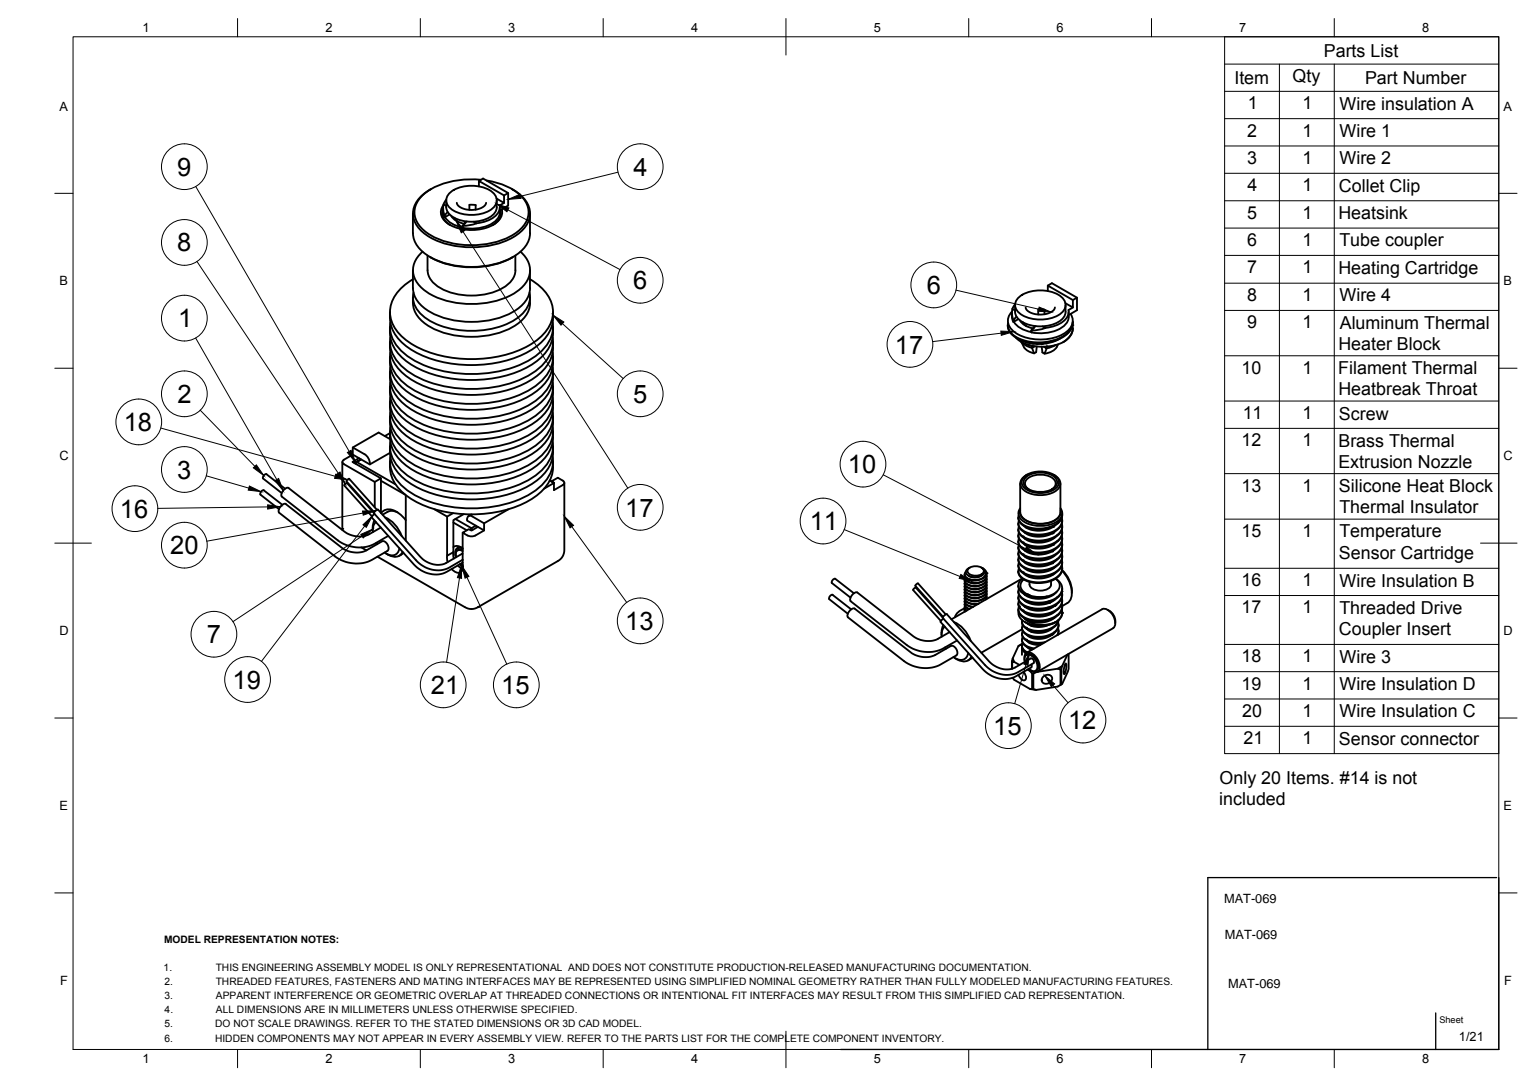
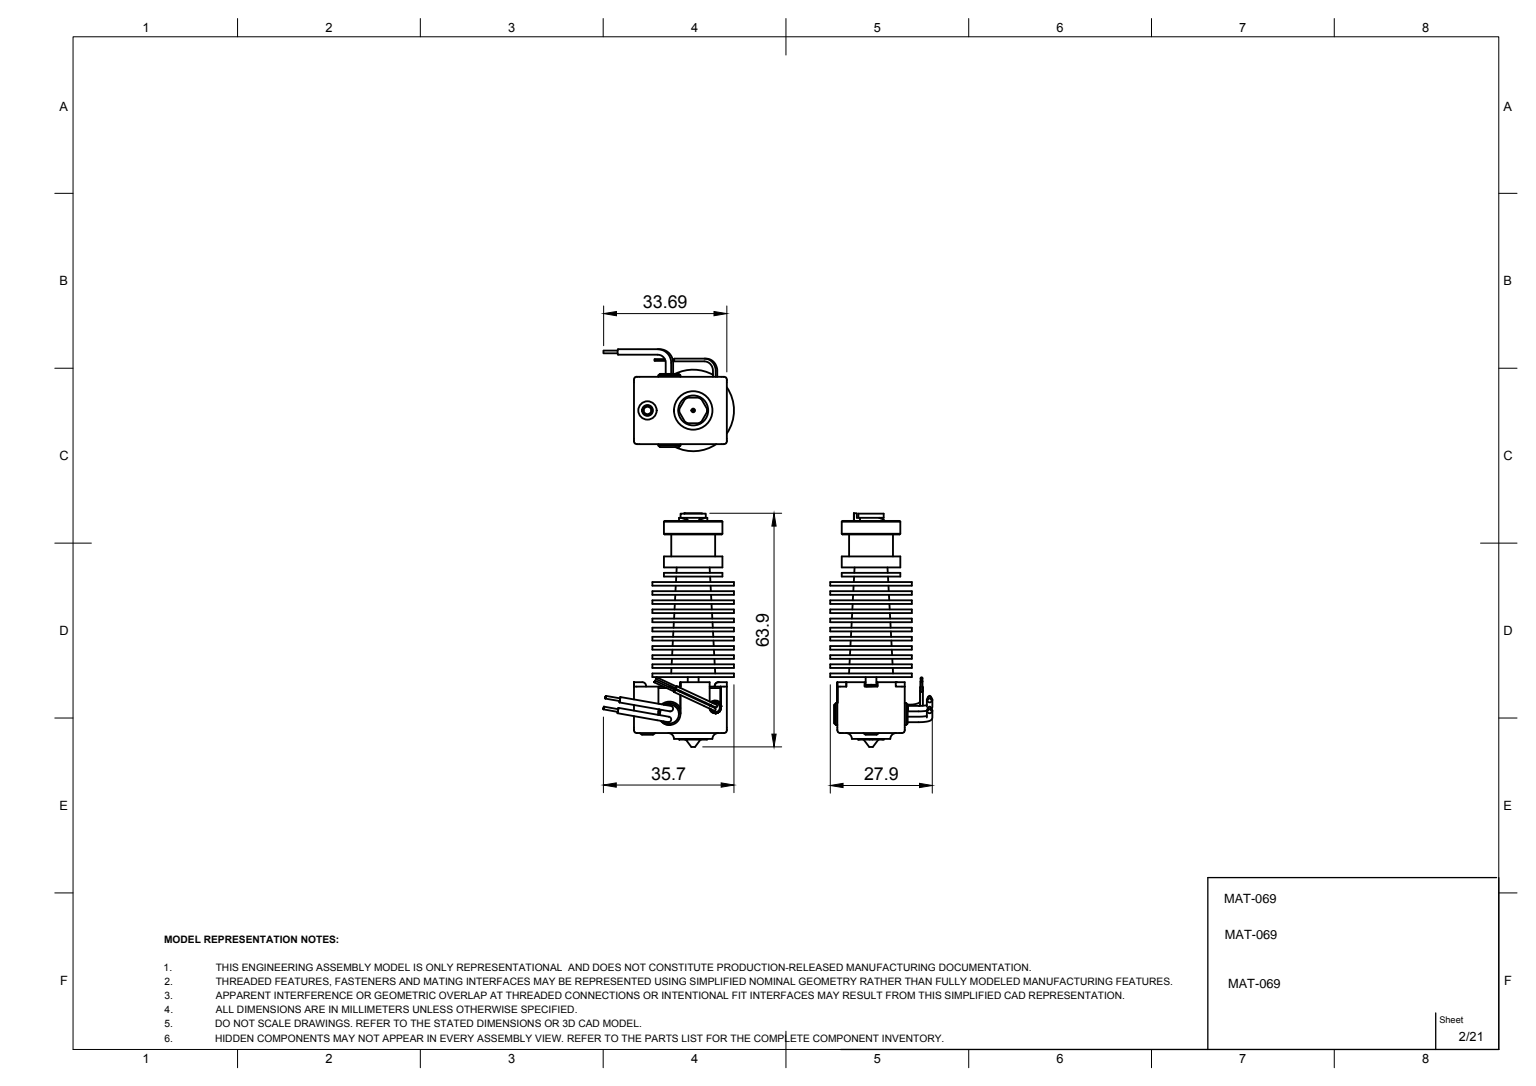
ISO-10303-21;
HEADER;
/* Generated by software containing ST-Developer
 * from STEP Tools, Inc. (www.steptools.com) 
 */

FILE_DESCRIPTION(
/* description */ ('CAx-IF Rec.Pracs.---Representation and Presentation of Product Manufa
cturing Information (PMI)---4.0---2014-10-13'),
/* implementation_level */ '2;1');

FILE_NAME(
/* name */ 'MAT-069',
/* time_stamp */ '2026-10-24T15:08:39-07:00',
/* author */ (''),
/* organization */ (''),
/* preprocessor_version */ 'ST-DEVELOPER v20.2',
/* originating_system */ 'Autodesk Translation Framework v15.17.0.0',
/* authorisation */ '');

FILE_SCHEMA (('AP242_MANAGED_MODEL_BASED_3D_ENGINEERING_MIM_LF { 1 0 10303 442 2 1 4 }'));
ENDSEC;

DATA;
#10=MECHANICAL_DESIGN_GEOMETRIC_PRESENTATION_REPRESENTATION('',(#820,#821,
#822,#823,#824,#825,#826,#827,#828,#829,#830,#831,#832,#833,#834,#835,#836,
#837,#838,#839),#50081);
#11=ITEM_DEFINED_TRANSFORMATION($,$,#10107,#11015);
#12=ITEM_DEFINED_TRANSFORMATION($,$,#10113,#11016);
#13=ITEM_DEFINED_TRANSFORMATION($,$,#10126,#11017);
#14=ITEM_DEFINED_TRANSFORMATION($,$,#10139,#11018);
#15=ITEM_DEFINED_TRANSFORMATION($,$,#10265,#11019);
#16=ITEM_DEFINED_TRANSFORMATION($,$,#10400,#11020);
#17=ITEM_DEFINED_TRANSFORMATION($,$,#10427,#11021);
#18=ITEM_DEFINED_TRANSFORMATION($,$,#10440,#11022);
#19=ITEM_DEFINED_TRANSFORMATION($,$,#10453,#11023);
#20=ITEM_DEFINED_TRANSFORMATION($,$,#10466,#11024);
#21=ITEM_DEFINED_TRANSFORMATION($,$,#10607,#11025);
#22=ITEM_DEFINED_TRANSFORMATION($,$,#10620,#11026);
#23=ITEM_DEFINED_TRANSFORMATION($,$,#10669,#11027);
#24=ITEM_DEFINED_TRANSFORMATION($,$,#10679,#11028);
#25=ITEM_DEFINED_TRANSFORMATION($,$,#10748,#11029);
#26=ITEM_DEFINED_TRANSFORMATION($,$,#10891,#11030);
#27=ITEM_DEFINED_TRANSFORMATION($,$,#10899,#11031);
#28=ITEM_DEFINED_TRANSFORMATION($,$,#10966,#11032);
#29=ITEM_DEFINED_TRANSFORMATION($,$,#10979,#11033);
#30=ITEM_DEFINED_TRANSFORMATION($,$,#10992,#11034);
#31=(
REPRESENTATION_RELATIONSHIP($,$,#50148,#50147)
REPRESENTATION_RELATIONSHIP_WITH_TRANSFORMATION(#11)
SHAPE_REPRESENTATION_RELATIONSHIP()
);
#32=(
REPRESENTATION_RELATIONSHIP($,$,#50149,#50147)
REPRESENTATION_RELATIONSHIP_WITH_TRANSFORMATION(#12)
SHAPE_REPRESENTATION_RELATIONSHIP()
);
#33=(
REPRESENTATION_RELATIONSHIP($,$,#50150,#50147)
REPRESENTATION_RELATIONSHIP_WITH_TRANSFORMATION(#13)
SHAPE_REPRESENTATION_RELATIONSHIP()
);
#34=(
REPRESENTATION_RELATIONSHIP($,$,#50151,#50147)
REPRESENTATION_RELATIONSHIP_WITH_TRANSFORMATION(#14)
SHAPE_REPRESENTATION_RELATIONSHIP()
);
#35=(
REPRESENTATION_RELATIONSHIP($,$,#50152,#50147)
REPRESENTATION_RELATIONSHIP_WITH_TRANSFORMATION(#15)
SHAPE_REPRESENTATION_RELATIONSHIP()
);
#36=(
REPRESENTATION_RELATIONSHIP($,$,#50153,#50147)
REPRESENTATION_RELATIONSHIP_WITH_TRANSFORMATION(#16)
SHAPE_REPRESENTATION_RELATIONSHIP()
);
#37=(
REPRESENTATION_RELATIONSHIP($,$,#50154,#50147)
REPRESENTATION_RELATIONSHIP_WITH_TRANSFORMATION(#17)
SHAPE_REPRESENTATION_RELATIONSHIP()
);
#38=(
REPRESENTATION_RELATIONSHIP($,$,#50155,#50147)
REPRESENTATION_RELATIONSHIP_WITH_TRANSFORMATION(#18)
SHAPE_REPRESENTATION_RELATIONSHIP()
);
#39=(
REPRESENTATION_RELATIONSHIP($,$,#50156,#50147)
REPRESENTATION_RELATIONSHIP_WITH_TRANSFORMATION(#19)
SHAPE_REPRESENTATION_RELATIONSHIP()
);
#40=(
REPRESENTATION_RELATIONSHIP($,$,#50157,#50147)
REPRESENTATION_RELATIONSHIP_WITH_TRANSFORMATION(#20)
SHAPE_REPRESENTATION_RELATIONSHIP()
);
#41=(
REPRESENTATION_RELATIONSHIP($,$,#50158,#50147)
REPRESENTATION_RELATIONSHIP_WITH_TRANSFORMATION(#21)
SHAPE_REPRESENTATION_RELATIONSHIP()
);
#42=(
REPRESENTATION_RELATIONSHIP($,$,#50159,#50147)
REPRESENTATION_RELATIONSHIP_WITH_TRANSFORMATION(#22)
SHAPE_REPRESENTATION_RELATIONSHIP()
);
#43=(
REPRESENTATION_RELATIONSHIP($,$,#50160,#50147)
REPRESENTATION_RELATIONSHIP_WITH_TRANSFORMATION(#23)
SHAPE_REPRESENTATION_RELATIONSHIP()
);
#44=(
REPRESENTATION_RELATIONSHIP($,$,#50161,#50147)
REPRESENTATION_RELATIONSHIP_WITH_TRANSFORMATION(#24)
SHAPE_REPRESENTATION_RELATIONSHIP()
);
#45=(
REPRESENTATION_RELATIONSHIP($,$,#50162,#50147)
REPRESENTATION_RELATIONSHIP_WITH_TRANSFORMATION(#25)
SHAPE_REPRESENTATION_RELATIONSHIP()
);
#46=(
REPRESENTATION_RELATIONSHIP($,$,#50163,#50147)
REPRESENTATION_RELATIONSHIP_WITH_TRANSFORMATION(#26)
SHAPE_REPRESENTATION_RELATIONSHIP()
);
#47=(
REPRESENTATION_RELATIONSHIP($,$,#50164,#50147)
REPRESENTATION_RELATIONSHIP_WITH_TRANSFORMATION(#27)
SHAPE_REPRESENTATION_RELATIONSHIP()
);
#48=(
REPRESENTATION_RELATIONSHIP($,$,#50165,#50147)
REPRESENTATION_RELATIONSHIP_WITH_TRANSFORMATION(#28)
SHAPE_REPRESENTATION_RELATIONSHIP()
);
#49=(
REPRESENTATION_RELATIONSHIP($,$,#50166,#50147)
REPRESENTATION_RELATIONSHIP_WITH_TRANSFORMATION(#29)
SHAPE_REPRESENTATION_RELATIONSHIP()
);
#50=(
REPRESENTATION_RELATIONSHIP($,$,#50167,#50147)
REPRESENTATION_RELATIONSHIP_WITH_TRANSFORMATION(#30)
SHAPE_REPRESENTATION_RELATIONSHIP()
);
#51=CONTEXT_DEPENDENT_SHAPE_REPRESENTATION(#31,#50127);
#52=CONTEXT_DEPENDENT_SHAPE_REPRESENTATION(#32,#50128);
#53=CONTEXT_DEPENDENT_SHAPE_REPRESENTATION(#33,#50129);
#54=CONTEXT_DEPENDENT_SHAPE_REPRESENTATION(#34,#50130);
#55=CONTEXT_DEPENDENT_SHAPE_REPRESENTATION(#35,#50131);
#56=CONTEXT_DEPENDENT_SHAPE_REPRESENTATION(#36,#50132);
#57=CONTEXT_DEPENDENT_SHAPE_REPRESENTATION(#37,#50133);
#58=CONTEXT_DEPENDENT_SHAPE_REPRESENTATION(#38,#50134);
#59=CONTEXT_DEPENDENT_SHAPE_REPRESENTATION(#39,#50135);
#60=CONTEXT_DEPENDENT_SHAPE_REPRESENTATION(#40,#50136);
#61=CONTEXT_DEPENDENT_SHAPE_REPRESENTATION(#41,#50137);
#62=CONTEXT_DEPENDENT_SHAPE_REPRESENTATION(#42,#50138);
#63=CONTEXT_DEPENDENT_SHAPE_REPRESENTATION(#43,#50139);
#64=CONTEXT_DEPENDENT_SHAPE_REPRESENTATION(#44,#50140);
#65=CONTEXT_DEPENDENT_SHAPE_REPRESENTATION(#45,#50141);
#66=CONTEXT_DEPENDENT_SHAPE_REPRESENTATION(#46,#50142);
#67=CONTEXT_DEPENDENT_SHAPE_REPRESENTATION(#47,#50143);
#68=CONTEXT_DEPENDENT_SHAPE_REPRESENTATION(#48,#50144);
#69=CONTEXT_DEPENDENT_SHAPE_REPRESENTATION(#49,#50145);
#70=CONTEXT_DEPENDENT_SHAPE_REPRESENTATION(#50,#50146);
#71=NEXT_ASSEMBLY_USAGE_OCCURRENCE('Sensor connector:1',
'Sensor connector:1','Sensor connector:1',#50169,#50170,
'Sensor connector:1');
#72=NEXT_ASSEMBLY_USAGE_OCCURRENCE('Wire Insulation D:1',
'Wire Insulation D:1','Wire Insulation D:1',#50169,#50171,
'Wire Insulation D:1');
#73=NEXT_ASSEMBLY_USAGE_OCCURRENCE('Wire Insulation C:1',
'Wire Insulation C:1','Wire Insulation C:1',#50169,#50172,
'Wire Insulation C:1');
#74=NEXT_ASSEMBLY_USAGE_OCCURRENCE('Tube coupler:1','Tube coupler:1',
'Tube coupler:1',#50169,#50173,'Tube coupler:1');
#75=NEXT_ASSEMBLY_USAGE_OCCURRENCE('Heatsink:1','Heatsink:1',
'Heatsink:1',#50169,#50174,'Heatsink:1');
#76=NEXT_ASSEMBLY_USAGE_OCCURRENCE('Collet Clip:1','Collet Clip:1',
'Collet Clip:1',#50169,#50175,'Collet Clip:1');
#77=NEXT_ASSEMBLY_USAGE_OCCURRENCE('Wire insulation A:1',
'Wire insulation A:1','Wire insulation A:1',#50169,#50176,
'Wire insulation A:1');
#78=NEXT_ASSEMBLY_USAGE_OCCURRENCE('Wire 2:1','Wire 2:1','Wire 2:1',#50169,
#50177,'Wire 2:1');
#79=NEXT_ASSEMBLY_USAGE_OCCURRENCE('Wire 1:1','Wire 1:1','Wire 1:1',#50169,
#50178,'Wire 1:1');
#80=NEXT_ASSEMBLY_USAGE_OCCURRENCE('Aluminum Thermal Heater Block:1',
'Aluminum Thermal Heater Block:1','Aluminum Thermal Heater Block:1',#50169,
#50179,'Aluminum Thermal Heater Block:1');
#81=NEXT_ASSEMBLY_USAGE_OCCURRENCE('Wire 4:1','Wire 4:1','Wire 4:1',#50169,
#50180,'Wire 4:1');
#82=NEXT_ASSEMBLY_USAGE_OCCURRENCE(
'Filament Thermal Heatbreak Throat:1',
'Filament Thermal Heatbreak Throat:1',
'Filament Thermal Heatbreak Throat:1',#50169,#50181,
'Filament Thermal Heatbreak Throat:1');
#83=NEXT_ASSEMBLY_USAGE_OCCURRENCE('Heating Cartridge:1',
'Heating Cartridge:1','Heating Cartridge:1',#50169,#50182,
'Heating Cartridge:1');
#84=NEXT_ASSEMBLY_USAGE_OCCURRENCE('Brass Thermal Extrusion Nozzle:1',
'Brass Thermal Extrusion Nozzle:1','Brass Thermal Extrusion Nozzle:1',#50169,
#50183,'Brass Thermal Extrusion Nozzle:1');
#85=NEXT_ASSEMBLY_USAGE_OCCURRENCE(
'Silicone Heat Block Thermal Insulator:1',
'Silicone Heat Block Thermal Insulator:1',
'Silicone Heat Block Thermal Insulator:1',#50169,#50184,
'Silicone Heat Block Thermal Insulator:1');
#86=NEXT_ASSEMBLY_USAGE_OCCURRENCE('Temperature Sensor Cartridge:1',
'Temperature Sensor Cartridge:1','Temperature Sensor Cartridge:1',#50169,
#50185,'Temperature Sensor Cartridge:1');
#87=NEXT_ASSEMBLY_USAGE_OCCURRENCE('Screw:1','Screw:1','Screw:1',#50169,
#50186,'Screw:1');
#88=NEXT_ASSEMBLY_USAGE_OCCURRENCE('Wire Insulation B:1',
'Wire Insulation B:1','Wire Insulation B:1',#50169,#50187,
'Wire Insulation B:1');
#89=NEXT_ASSEMBLY_USAGE_OCCURRENCE('Wire 3:1','Wire 3:1','Wire 3:1',#50169,
#50188,'Wire 3:1');
#90=NEXT_ASSEMBLY_USAGE_OCCURRENCE('Threaded Drive Coupler Insert:1',
'Threaded Drive Coupler Insert:1','Threaded Drive Coupler Insert:1',#50169,
#50189,'Threaded Drive Coupler Insert:1');
#91=(
BOUNDED_SURFACE()
B_SPLINE_SURFACE(1,2,((#48380,#48381,#48382,#48383,#48384,#48385,#48386,
#48387,#48388,#48389,#48390,#48391,#48392,#48393,#48394,#48395,#48396,#48397,
#48398,#48399,#48400,#48401,#48402,#48403,#48404,#48405,#48406,#48407,#48408,
#48409,#48410,#48411,#48412,#48413,#48414,#48415,#48416,#48417,#48418,#48419,
#48420,#48421,#48422,#48423,#48424,#48425,#48426,#48427,#48428,#48429,#48430,
#48431,#48432,#48433,#48434,#48435,#48436,#48437,#48438,#48439,#48440,#48441,
#48442,#48443,#48444,#48445,#48446,#48447,#48448,#48449,#48450,#48451,#48452,
#48453,#48454,#48455,#48456,#48457,#48458,#48459,#48460,#48461,#48462,#48463,
#48464,#48465,#48466,#48467,#48468,#48469,#48470,#48471,#48472,#48473,#48474,
#48475,#48476,#48477,#48478,#48479,#48480,#48481,#48482,#48483,#48484,#48485,
#48486,#48487,#48488,#48489,#48490,#48491,#48492,#48493,#48494,#48495,#48496,
#48497,#48498,#48499,#48500,#48501,#48502,#48503,#48504,#48505,#48506,#48507,
#48508,#48509,#48510,#48511,#48512,#48513,#48514,#48515,#48516,#48517,#48518,
#48519,#48520,#48521,#48522,#48523,#48524,#48525,#48526,#48527,#48528,#48529,
#48530,#48531,#48532,#48533,#48534,#48535,#48536,#48537,#48538,#48539,#48540,
#48541,#48542,#48543,#48544,#48545,#48546,#48547,#48548,#48549,#48550,#48551,
#48552,#48553,#48554,#48555,#48556,#48557,#48558,#48559,#48560,#48561,#48562,
#48563,#48564,#48565,#48566,#48567,#48568,#48569,#48570,#48571,#48572,#48573,
#48574,#48575,#48576,#48577,#48578),(#48579,#48580,#48581,#48582,#48583,
#48584,#48585,#48586,#48587,#48588,#48589,#48590,#48591,#48592,#48593,#48594,
#48595,#48596,#48597,#48598,#48599,#48600,#48601,#48602,#48603,#48604,#48605,
#48606,#48607,#48608,#48609,#48610,#48611,#48612,#48613,#48614,#48615,#48616,
#48617,#48618,#48619,#48620,#48621,#48622,#48623,#48624,#48625,#48626,#48627,
#48628,#48629,#48630,#48631,#48632,#48633,#48634,#48635,#48636,#48637,#48638,
#48639,#48640,#48641,#48642,#48643,#48644,#48645,#48646,#48647,#48648,#48649,
#48650,#48651,#48652,#48653,#48654,#48655,#48656,#48657,#48658,#48659,#48660,
#48661,#48662,#48663,#48664,#48665,#48666,#48667,#48668,#48669,#48670,#48671,
#48672,#48673,#48674,#48675,#48676,#48677,#48678,#48679,#48680,#48681,#48682,
#48683,#48684,#48685,#48686,#48687,#48688,#48689,#48690,#48691,#48692,#48693,
#48694,#48695,#48696,#48697,#48698,#48699,#48700,#48701,#48702,#48703,#48704,
#48705,#48706,#48707,#48708,#48709,#48710,#48711,#48712,#48713,#48714,#48715,
#48716,#48717,#48718,#48719,#48720,#48721,#48722,#48723,#48724,#48725,#48726,
#48727,#48728,#48729,#48730,#48731,#48732,#48733,#48734,#48735,#48736,#48737,
#48738,#48739,#48740,#48741,#48742,#48743,#48744,#48745,#48746,#48747,#48748,
#48749,#48750,#48751,#48752,#48753,#48754,#48755,#48756,#48757,#48758,#48759,
#48760,#48761,#48762,#48763,#48764,#48765,#48766,#48767,#48768,#48769,#48770,
#48771,#48772,#48773,#48774,#48775,#48776,#48777)),.UNSPECIFIED.,.F.,.F.,
 .F.)
B_SPLINE_SURFACE_WITH_KNOTS((2,2),(3,2,2,2,2,2,2,2,2,2,2,2,2,2,2,2,2,2,
2,2,2,2,2,2,2,2,2,2,2,2,2,2,2,2,2,2,2,2,2,2,2,2,2,2,2,2,2,2,2,2,2,2,2,2,
2,2,2,2,2,2,2,2,2,2,2,2,2,2,2,2,2,2,2,2,2,2,2,2,2,2,2,2,2,2,2,2,2,2,2,2,
2,2,2,2,2,2,2,2,2,3),(0.,1.00004093151987),(0.0295122414599334,0.0392156862745098,
0.0490196078431373,0.0588235294117647,0.0686274509803922,0.0784313725490196,
0.0882352941176471,0.0980392156862745,0.107843137254902,0.117647058823529,
0.127450980392157,0.137254901960784,0.147058823529412,0.156862745098039,
0.166666666666667,0.176470588235294,0.186274509803922,0.196078431372549,
0.205882352941176,0.215686274509804,0.225490196078431,0.235294117647059,
0.245098039215686,0.254901960784314,0.264705882352941,0.274509803921569,
0.284313725490196,0.294117647058824,0.303921568627451,0.313725490196078,
0.323529411764706,0.333333333333333,0.343137254901961,0.352941176470588,
0.362745098039216,0.372549019607843,0.382352941176471,0.392156862745098,
0.401960784313726,0.411764705882353,0.42156862745098,0.431372549019608,
0.441176470588235,0.450980392156863,0.46078431372549,0.470588235294118,
0.480392156862745,0.490196078431373,0.5,0.509803921568627,0.519607843137255,
0.529411764705882,0.53921568627451,0.549019607843137,0.558823529411765,
0.568627450980392,0.57843137254902,0.588235294117647,0.598039215686274,
0.607843137254902,0.617647058823529,0.627450980392157,0.637254901960784,
0.647058823529412,0.656862745098039,0.666666666666667,0.676470588235294,
0.686274509803922,0.696078431372549,0.705882352941177,0.715686274509804,
0.725490196078431,0.735294117647059,0.745098039215686,0.754901960784314,
0.764705882352941,0.774509803921569,0.784313725490196,0.794117647058823,
0.803921568627451,0.813725490196078,0.823529411764706,0.833333333333333,
0.843137254901961,0.852941176470588,0.862745098039216,0.872549019607843,
0.882352941176471,0.892156862745098,0.901960784313726,0.911764705882353,
0.92156862745098,0.931372549019608,0.941176470588235,0.950980392156863,
0.96078431372549,0.970588235294118,0.980392156862745,0.990196078431373,
0.998519452012734),.UNSPECIFIED.)
GEOMETRIC_REPRESENTATION_ITEM()
RATIONAL_B_SPLINE_SURFACE(((0.997282032040392,0.867398459704848,1.,0.866025403784439,
1.,0.866025403784439,1.,0.866025403784439,1.,0.866025403784439,1.,0.866025403784439,
1.,0.866025403784439,1.,0.866025403784439,1.,0.866025403784439,1.,0.866025403784439,
1.,0.866025403784439,1.,0.866025403784439,1.,0.866025403784439,1.,0.866025403784439,
1.,0.866025403784439,1.,0.866025403784439,1.,0.866025403784439,1.,0.866025403784439,
1.,0.866025403784439,1.,0.866025403784439,1.,0.866025403784439,1.,0.866025403784439,
1.,0.866025403784439,1.,0.866025403784439,1.,0.866025403784439,1.,0.866025403784439,
1.,0.866025403784439,1.,0.866025403784439,1.,0.866025403784439,1.,0.866025403784439,
1.,0.866025403784439,1.,0.866025403784439,1.,0.866025403784439,1.,0.866025403784439,
1.,0.866025403784439,1.,0.866025403784439,1.,0.866025403784439,1.,0.866025403784439,
1.,0.866025403784439,1.,0.866025403784439,1.,0.866025403784439,1.,0.866025403784439,
1.,0.866025403784439,1.,0.866025403784439,1.,0.866025403784439,1.,0.866025403784439,
1.,0.866025403784439,1.,0.866025403784439,1.,0.866025403784439,1.,0.866025403784439,
1.,0.866025403784439,1.,0.866025403784439,1.,0.866025403784439,1.,0.866025403784439,
1.,0.866025403784439,1.,0.866025403784439,1.,0.866025403784439,1.,0.866025403784439,
1.,0.866025403784439,1.,0.866025403784439,1.,0.866025403784439,1.,0.866025403784439,
1.,0.866025403784439,1.,0.866025403784439,1.,0.866025403784439,1.,0.866025403784439,
1.,0.866025403784439,1.,0.866025403784439,1.,0.866025403784439,1.,0.866025403784439,
1.,0.866025403784439,1.,0.866025403784439,1.,0.866025403784439,1.,0.866025403784439,
1.,0.866025403784439,1.,0.866025403784439,1.,0.866025403784439,1.,0.866025403784439,
1.,0.866025403784439,1.,0.866025403784439,1.,0.866025403784439,1.,0.866025403784439,
1.,0.866025403784439,1.,0.866025403784439,1.,0.866025403784439,1.,0.866025403784439,
1.,0.866025403784439,1.,0.866025403784439,1.,0.866025403784439,1.,0.866025403784439,
1.,0.866025403784439,1.,0.866025403784439,1.,0.866025403784439,1.,0.866025403784439,
1.,0.866025403784439,1.,0.866025403784439,1.,0.866025403784439,1.,0.866025403784439,
1.,0.886257697299162,0.965646208784519),(0.997282032040392,0.867398459704848,
1.,0.866025403784439,1.,0.866025403784439,1.,0.866025403784439,1.,0.866025403784439,
1.,0.866025403784439,1.,0.866025403784439,1.,0.866025403784439,1.,0.866025403784439,
1.,0.866025403784439,1.,0.866025403784439,1.,0.866025403784439,1.,0.866025403784439,
1.,0.866025403784439,1.,0.866025403784439,1.,0.866025403784439,1.,0.866025403784439,
1.,0.866025403784439,1.,0.866025403784439,1.,0.866025403784439,1.,0.866025403784439,
1.,0.866025403784439,1.,0.866025403784439,1.,0.866025403784439,1.,0.866025403784439,
1.,0.866025403784439,1.,0.866025403784439,1.,0.866025403784439,1.,0.866025403784439,
1.,0.866025403784439,1.,0.866025403784439,1.,0.866025403784439,1.,0.866025403784439,
1.,0.866025403784439,1.,0.866025403784439,1.,0.866025403784439,1.,0.866025403784439,
1.,0.866025403784439,1.,0.866025403784439,1.,0.866025403784439,1.,0.866025403784439,
1.,0.866025403784439,1.,0.866025403784439,1.,0.866025403784439,1.,0.866025403784439,
1.,0.866025403784439,1.,0.866025403784439,1.,0.866025403784439,1.,0.866025403784439,
1.,0.866025403784439,1.,0.866025403784439,1.,0.866025403784439,1.,0.866025403784439,
1.,0.866025403784439,1.,0.866025403784439,1.,0.866025403784439,1.,0.866025403784439,
1.,0.866025403784439,1.,0.866025403784439,1.,0.866025403784439,1.,0.866025403784439,
1.,0.866025403784439,1.,0.866025403784439,1.,0.866025403784439,1.,0.866025403784439,
1.,0.866025403784439,1.,0.866025403784439,1.,0.866025403784439,1.,0.866025403784439,
1.,0.866025403784439,1.,0.866025403784439,1.,0.866025403784439,1.,0.866025403784439,
1.,0.866025403784439,1.,0.866025403784439,1.,0.866025403784439,1.,0.866025403784439,
1.,0.866025403784439,1.,0.866025403784439,1.,0.866025403784439,1.,0.866025403784439,
1.,0.866025403784439,1.,0.866025403784439,1.,0.866025403784439,1.,0.866025403784439,
1.,0.866025403784439,1.,0.866025403784439,1.,0.866025403784439,1.,0.866025403784439,
1.,0.866025403784439,1.,0.866025403784439,1.,0.866025403784439,1.,0.866025403784439,
1.,0.866025403784439,1.,0.866025403784439,1.,0.866025403784439,1.,0.866025403784439,
1.,0.866025403784439,1.,0.886257697299162,0.965646208784519)))
REPRESENTATION_ITEM('')
SURFACE()
);
#92=(
BOUNDED_SURFACE()
B_SPLINE_SURFACE(1,2,((#48794,#48795,#48796,#48797,#48798,#48799,#48800,
#48801,#48802,#48803,#48804,#48805,#48806,#48807,#48808,#48809,#48810,#48811,
#48812,#48813,#48814,#48815,#48816,#48817,#48818,#48819,#48820,#48821,#48822,
#48823,#48824,#48825,#48826,#48827,#48828,#48829,#48830,#48831,#48832,#48833,
#48834,#48835,#48836,#48837,#48838,#48839,#48840,#48841,#48842,#48843,#48844,
#48845,#48846,#48847,#48848,#48849,#48850,#48851,#48852,#48853,#48854,#48855,
#48856,#48857,#48858,#48859,#48860,#48861,#48862,#48863,#48864,#48865,#48866,
#48867,#48868,#48869,#48870,#48871,#48872,#48873,#48874,#48875,#48876,#48877,
#48878,#48879,#48880,#48881,#48882,#48883,#48884,#48885,#48886,#48887,#48888,
#48889,#48890,#48891,#48892,#48893,#48894,#48895,#48896,#48897,#48898,#48899,
#48900,#48901,#48902,#48903,#48904,#48905,#48906,#48907,#48908,#48909,#48910,
#48911,#48912,#48913,#48914,#48915,#48916,#48917,#48918,#48919,#48920,#48921,
#48922,#48923,#48924,#48925,#48926,#48927,#48928,#48929,#48930,#48931,#48932,
#48933,#48934,#48935,#48936,#48937,#48938,#48939,#48940,#48941,#48942,#48943,
#48944,#48945,#48946,#48947,#48948,#48949,#48950,#48951,#48952,#48953,#48954,
#48955,#48956,#48957,#48958,#48959,#48960,#48961,#48962,#48963,#48964,#48965,
#48966,#48967,#48968,#48969,#48970,#48971,#48972,#48973,#48974,#48975,#48976,
#48977,#48978,#48979,#48980,#48981,#48982,#48983,#48984,#48985,#48986,#48987,
#48988),(#48989,#48990,#48991,#48992,#48993,#48994,#48995,#48996,#48997,
#48998,#48999,#49000,#49001,#49002,#49003,#49004,#49005,#49006,#49007,#49008,
#49009,#49010,#49011,#49012,#49013,#49014,#49015,#49016,#49017,#49018,#49019,
#49020,#49021,#49022,#49023,#49024,#49025,#49026,#49027,#49028,#49029,#49030,
#49031,#49032,#49033,#49034,#49035,#49036,#49037,#49038,#49039,#49040,#49041,
#49042,#49043,#49044,#49045,#49046,#49047,#49048,#49049,#49050,#49051,#49052,
#49053,#49054,#49055,#49056,#49057,#49058,#49059,#49060,#49061,#49062,#49063,
#49064,#49065,#49066,#49067,#49068,#49069,#49070,#49071,#49072,#49073,#49074,
#49075,#49076,#49077,#49078,#49079,#49080,#49081,#49082,#49083,#49084,#49085,
#49086,#49087,#49088,#49089,#49090,#49091,#49092,#49093,#49094,#49095,#49096,
#49097,#49098,#49099,#49100,#49101,#49102,#49103,#49104,#49105,#49106,#49107,
#49108,#49109,#49110,#49111,#49112,#49113,#49114,#49115,#49116,#49117,#49118,
#49119,#49120,#49121,#49122,#49123,#49124,#49125,#49126,#49127,#49128,#49129,
#49130,#49131,#49132,#49133,#49134,#49135,#49136,#49137,#49138,#49139,#49140,
#49141,#49142,#49143,#49144,#49145,#49146,#49147,#49148,#49149,#49150,#49151,
#49152,#49153,#49154,#49155,#49156,#49157,#49158,#49159,#49160,#49161,#49162,
#49163,#49164,#49165,#49166,#49167,#49168,#49169,#49170,#49171,#49172,#49173,
#49174,#49175,#49176,#49177,#49178,#49179,#49180,#49181,#49182,#49183)),
 .UNSPECIFIED.,.F.,.F.,.F.)
B_SPLINE_SURFACE_WITH_KNOTS((2,2),(3,2,2,2,2,2,2,2,2,2,2,2,2,2,2,2,2,2,
2,2,2,2,2,2,2,2,2,2,2,2,2,2,2,2,2,2,2,2,2,2,2,2,2,2,2,2,2,2,2,2,2,2,2,2,
2,2,2,2,2,2,2,2,2,2,2,2,2,2,2,2,2,2,2,2,2,2,2,2,2,2,2,2,2,2,2,2,2,2,2,2,
2,2,2,2,2,2,2,3),(-4.46693850465293E-5,1.00004466937728),(0.0222318908269079,
0.0294117647058824,0.0392156862745098,0.0490196078431373,0.0588235294117647,
0.0686274509803922,0.0784313725490196,0.0882352941176471,0.0980392156862745,
0.107843137254902,0.117647058823529,0.127450980392157,0.137254901960784,
0.147058823529412,0.156862745098039,0.166666666666667,0.176470588235294,
0.186274509803922,0.196078431372549,0.205882352941176,0.215686274509804,
0.225490196078431,0.235294117647059,0.245098039215686,0.254901960784314,
0.264705882352941,0.274509803921569,0.284313725490196,0.294117647058824,
0.303921568627451,0.313725490196078,0.323529411764706,0.333333333333333,
0.343137254901961,0.352941176470588,0.362745098039216,0.372549019607843,
0.382352941176471,0.392156862745098,0.401960784313726,0.411764705882353,
0.42156862745098,0.431372549019608,0.441176470588235,0.450980392156863,
0.46078431372549,0.470588235294118,0.480392156862745,0.490196078431373,
0.5,0.509803921568627,0.519607843137255,0.529411764705882,0.53921568627451,
0.549019607843137,0.558823529411765,0.568627450980392,0.57843137254902,
0.588235294117647,0.598039215686274,0.607843137254902,0.617647058823529,
0.627450980392157,0.637254901960784,0.647058823529412,0.656862745098039,
0.666666666666667,0.676470588235294,0.686274509803922,0.696078431372549,
0.705882352941177,0.715686274509804,0.725490196078431,0.735294117647059,
0.745098039215686,0.754901960784314,0.764705882352941,0.774509803921569,
0.784313725490196,0.794117647058823,0.803921568627451,0.813725490196078,
0.823529411764706,0.833333333333333,0.843137254901961,0.852941176470588,
0.862745098039216,0.872549019607843,0.882352941176471,0.892156862745098,
0.901960784313726,0.911764705882353,0.92156862745098,0.931372549019608,
0.941176470588235,0.950980392156863,0.96078431372549,0.968975690801275),
 .UNSPECIFIED.)
GEOMETRIC_REPRESENTATION_ITEM()
RATIONAL_B_SPLINE_SURFACE(((0.947477990343754,0.901884088210946,1.,0.866025403784439,
1.,0.866025403784439,1.,0.866025403784439,1.,0.866025403784439,1.,0.866025403784439,
1.,0.866025403784439,1.,0.866025403784439,1.,0.866025403784439,1.,0.866025403784439,
1.,0.866025403784439,1.,0.866025403784439,1.,0.866025403784439,1.,0.866025403784439,
1.,0.866025403784439,1.,0.866025403784439,1.,0.866025403784439,1.,0.866025403784439,
1.,0.866025403784439,1.,0.866025403784439,1.,0.866025403784439,1.,0.866025403784439,
1.,0.866025403784439,1.,0.866025403784439,1.,0.866025403784439,1.,0.866025403784439,
1.,0.866025403784439,1.,0.866025403784439,1.,0.866025403784439,1.,0.866025403784439,
1.,0.866025403784439,1.,0.866025403784439,1.,0.866025403784439,1.,0.866025403784439,
1.,0.866025403784439,1.,0.866025403784439,1.,0.866025403784439,1.,0.866025403784439,
1.,0.866025403784439,1.,0.866025403784439,1.,0.866025403784439,1.,0.866025403784439,
1.,0.866025403784439,1.,0.866025403784439,1.,0.866025403784439,1.,0.866025403784439,
1.,0.866025403784439,1.,0.866025403784439,1.,0.866025403784439,1.,0.866025403784439,
1.,0.866025403784439,1.,0.866025403784439,1.,0.866025403784439,1.,0.866025403784439,
1.,0.866025403784439,1.,0.866025403784439,1.,0.866025403784439,1.,0.866025403784439,
1.,0.866025403784439,1.,0.866025403784439,1.,0.866025403784439,1.,0.866025403784439,
1.,0.866025403784439,1.,0.866025403784439,1.,0.866025403784439,1.,0.866025403784439,
1.,0.866025403784439,1.,0.866025403784439,1.,0.866025403784439,1.,0.866025403784439,
1.,0.866025403784439,1.,0.866025403784439,1.,0.866025403784439,1.,0.866025403784439,
1.,0.866025403784439,1.,0.866025403784439,1.,0.866025403784439,1.,0.866025403784439,
1.,0.866025403784439,1.,0.866025403784439,1.,0.866025403784439,1.,0.866025403784439,
1.,0.866025403784439,1.,0.866025403784439,1.,0.866025403784439,1.,0.866025403784439,
1.,0.866025403784439,1.,0.866025403784439,1.,0.866025403784439,1.,0.866025403784439,
1.,0.866025403784439,1.,0.866025403784439,1.,0.866025403784439,1.,0.866025403784439,
1.,0.866025403784439,1.,0.866025403784439,1.,0.888061483509882,0.963176808986156),
(0.947477990343754,0.901884088210946,1.,0.866025403784439,1.,0.866025403784439,
1.,0.866025403784439,1.,0.866025403784439,1.,0.866025403784439,1.,0.866025403784439,
1.,0.866025403784439,1.,0.866025403784439,1.,0.866025403784439,1.,0.866025403784439,
1.,0.866025403784439,1.,0.866025403784439,1.,0.866025403784439,1.,0.866025403784439,
1.,0.866025403784439,1.,0.866025403784439,1.,0.866025403784439,1.,0.866025403784439,
1.,0.866025403784439,1.,0.866025403784439,1.,0.866025403784439,1.,0.866025403784439,
1.,0.866025403784439,1.,0.866025403784439,1.,0.866025403784439,1.,0.866025403784439,
1.,0.866025403784439,1.,0.866025403784439,1.,0.866025403784439,1.,0.866025403784439,
1.,0.866025403784439,1.,0.866025403784439,1.,0.866025403784439,1.,0.866025403784439,
1.,0.866025403784439,1.,0.866025403784439,1.,0.866025403784439,1.,0.866025403784439,
1.,0.866025403784439,1.,0.866025403784439,1.,0.866025403784439,1.,0.866025403784439,
1.,0.866025403784439,1.,0.866025403784439,1.,0.866025403784439,1.,0.866025403784439,
1.,0.866025403784439,1.,0.866025403784439,1.,0.866025403784439,1.,0.866025403784439,
1.,0.866025403784439,1.,0.866025403784439,1.,0.866025403784439,1.,0.866025403784439,
1.,0.866025403784439,1.,0.866025403784439,1.,0.866025403784439,1.,0.866025403784439,
1.,0.866025403784439,1.,0.866025403784439,1.,0.866025403784439,1.,0.866025403784439,
1.,0.866025403784439,1.,0.866025403784439,1.,0.866025403784439,1.,0.866025403784439,
1.,0.866025403784439,1.,0.866025403784439,1.,0.866025403784439,1.,0.866025403784439,
1.,0.866025403784439,1.,0.866025403784439,1.,0.866025403784439,1.,0.866025403784439,
1.,0.866025403784439,1.,0.866025403784439,1.,0.866025403784439,1.,0.866025403784439,
1.,0.866025403784439,1.,0.866025403784439,1.,0.866025403784439,1.,0.866025403784439,
1.,0.866025403784439,1.,0.866025403784439,1.,0.866025403784439,1.,0.866025403784439,
1.,0.866025403784439,1.,0.866025403784439,1.,0.866025403784439,1.,0.866025403784439,
1.,0.866025403784439,1.,0.866025403784439,1.,0.866025403784439,1.,0.866025403784439,
1.,0.866025403784439,1.,0.888061483509882,0.963176808986156)))
REPRESENTATION_ITEM('')
SURFACE()
);
#93=SPHERICAL_SURFACE('',#10942,0.00317192226735973);
#94=B_SPLINE_SURFACE_WITH_KNOTS('',3,3,((#16932,#16933,#16934,#16935,#16936,
#16937,#16938,#16939,#16940,#16941,#16942,#16943,#16944,#16945,#16946,#16947,
#16948,#16949,#16950,#16951,#16952,#16953,#16954,#16955,#16956,#16957,#16958,
#16959,#16960,#16961,#16962,#16963,#16964,#16965,#16966,#16967,#16968,#16969,
#16970,#16971,#16972,#16973,#16974,#16975,#16976,#16977,#16978,#16979,#16980,
#16981,#16982,#16983,#16984,#16985,#16986,#16987,#16988,#16989,#16990,#16991,
#16992,#16993,#16994,#16995,#16996,#16997,#16998,#16999,#17000,#17001,#17002,
#17003,#17004,#17005,#17006,#17007,#17008,#17009,#17010,#17011,#17012,#17013,
#17014,#17015,#17016,#17017,#17018,#17019,#17020,#17021,#17022,#17023,#17024),
(#17025,#17026,#17027,#17028,#17029,#17030,#17031,#17032,#17033,#17034,
#17035,#17036,#17037,#17038,#17039,#17040,#17041,#17042,#17043,#17044,#17045,
#17046,#17047,#17048,#17049,#17050,#17051,#17052,#17053,#17054,#17055,#17056,
#17057,#17058,#17059,#17060,#17061,#17062,#17063,#17064,#17065,#17066,#17067,
#17068,#17069,#17070,#17071,#17072,#17073,#17074,#17075,#17076,#17077,#17078,
#17079,#17080,#17081,#17082,#17083,#17084,#17085,#17086,#17087,#17088,#17089,
#17090,#17091,#17092,#17093,#17094,#17095,#17096,#17097,#17098,#17099,#17100,
#17101,#17102,#17103,#17104,#17105,#17106,#17107,#17108,#17109,#17110,#17111,
#17112,#17113,#17114,#17115,#17116,#17117),(#17118,#17119,#17120,#17121,
#17122,#17123,#17124,#17125,#17126,#17127,#17128,#17129,#17130,#17131,#17132,
#17133,#17134,#17135,#17136,#17137,#17138,#17139,#17140,#17141,#17142,#17143,
#17144,#17145,#17146,#17147,#17148,#17149,#17150,#17151,#17152,#17153,#17154,
#17155,#17156,#17157,#17158,#17159,#17160,#17161,#17162,#17163,#17164,#17165,
#17166,#17167,#17168,#17169,#17170,#17171,#17172,#17173,#17174,#17175,#17176,
#17177,#17178,#17179,#17180,#17181,#17182,#17183,#17184,#17185,#17186,#17187,
#17188,#17189,#17190,#17191,#17192,#17193,#17194,#17195,#17196,#17197,#17198,
#17199,#17200,#17201,#17202,#17203,#17204,#17205,#17206,#17207,#17208,#17209,
#17210),(#17211,#17212,#17213,#17214,#17215,#17216,#17217,#17218,#17219,
#17220,#17221,#17222,#17223,#17224,#17225,#17226,#17227,#17228,#17229,#17230,
#17231,#17232,#17233,#17234,#17235,#17236,#17237,#17238,#17239,#17240,#17241,
#17242,#17243,#17244,#17245,#17246,#17247,#17248,#17249,#17250,#17251,#17252,
#17253,#17254,#17255,#17256,#17257,#17258,#17259,#17260,#17261,#17262,#17263,
#17264,#17265,#17266,#17267,#17268,#17269,#17270,#17271,#17272,#17273,#17274,
#17275,#17276,#17277,#17278,#17279,#17280,#17281,#17282,#17283,#17284,#17285,
#17286,#17287,#17288,#17289,#17290,#17291,#17292,#17293,#17294,#17295,#17296,
#17297,#17298,#17299,#17300,#17301,#17302,#17303)),.UNSPECIFIED.,.F.,.F.,
 .F.,(4,4),(4,1,1,1,1,1,1,1,1,1,1,1,1,1,1,1,1,1,1,1,1,1,1,1,1,1,1,1,1,1,
1,1,1,1,1,1,1,1,1,1,1,1,1,1,1,1,1,1,1,1,1,1,1,1,1,1,1,1,1,1,1,1,1,1,1,1,
1,1,1,1,1,1,1,1,1,1,1,1,1,1,1,1,1,1,1,1,1,1,1,1,4),(-0.000398919436546387,
0.0651101464894062),(10.2099830649134,11.2099710040949,12.2097658840232,
13.2095607639514,14.2093556438797,15.2091505238079,16.2089454037362,17.2087402836644,
18.2085351635927,19.208330043521,20.2081249234492,21.2079198033775,22.2077146833057,
23.207509563234,24.2073044431622,25.2070993230905,26.2068942030187,27.206689082947,
28.2064839628752,29.2062788428035,30.2060737227317,31.20586860266,32.2056634825882,
33.2054583625165,34.2052532424447,35.205048122373,36.2048430023012,37.2046378822295,
38.2044327621577,39.204227642086,40.2040225220142,41.2038174019425,42.2036122818707,
43.203407161799,44.2032020417273,45.2029969216555,46.2027918015838,47.202586681512,
48.2023815614403,49.2021764413685,50.2019713212968,51.201766201225,52.2015610811533,
53.2013559610815,54.2011508410098,55.200945720938,56.2007406008663,57.2005354807945,
58.2003303607228,59.200125240651,60.1999201205793,61.1997150005075,62.1995098804358,
63.199304760364,64.1990996402923,65.1988945202205,66.1986894001488,67.1984842800771,
68.1982791600053,69.1980740399336,70.1978689198618,71.1976637997901,72.1974586797183,
73.1972535596466,74.1970484395748,75.1968433195031,76.1966381994313,77.1964330793596,
78.1962279592878,79.1960228392161,80.1958177191443,81.1956125990726,82.1954074790008,
83.1952023589291,84.1949972388573,85.1947921187856,86.1945869987138,87.1943818786421,
88.1941767585704,89.1939716384986,90.1937665184269,91.1935613983551,92.1933562782833,
93.1931511582116,94.1929460381399,95.1927409180681,96.1925357979964,97.1923306779246,
98.1921255578529,99.1919204377811,100.192067891578),.UNSPECIFIED.);
#95=B_SPLINE_SURFACE_WITH_KNOTS('',3,3,((#17371,#17372,#17373,#17374,#17375,
#17376,#17377,#17378,#17379,#17380,#17381,#17382,#17383,#17384,#17385,#17386,
#17387,#17388,#17389,#17390,#17391,#17392,#17393,#17394,#17395,#17396,#17397,
#17398,#17399,#17400,#17401,#17402,#17403,#17404,#17405,#17406,#17407,#17408,
#17409,#17410,#17411,#17412,#17413,#17414,#17415,#17416,#17417,#17418,#17419,
#17420,#17421,#17422,#17423,#17424,#17425,#17426,#17427,#17428,#17429,#17430,
#17431,#17432,#17433,#17434,#17435,#17436,#17437,#17438,#17439,#17440,#17441,
#17442,#17443,#17444,#17445,#17446,#17447,#17448,#17449,#17450,#17451,#17452,
#17453,#17454,#17455,#17456,#17457,#17458,#17459,#17460,#17461,#17462,#17463),
(#17464,#17465,#17466,#17467,#17468,#17469,#17470,#17471,#17472,#17473,
#17474,#17475,#17476,#17477,#17478,#17479,#17480,#17481,#17482,#17483,#17484,
#17485,#17486,#17487,#17488,#17489,#17490,#17491,#17492,#17493,#17494,#17495,
#17496,#17497,#17498,#17499,#17500,#17501,#17502,#17503,#17504,#17505,#17506,
#17507,#17508,#17509,#17510,#17511,#17512,#17513,#17514,#17515,#17516,#17517,
#17518,#17519,#17520,#17521,#17522,#17523,#17524,#17525,#17526,#17527,#17528,
#17529,#17530,#17531,#17532,#17533,#17534,#17535,#17536,#17537,#17538,#17539,
#17540,#17541,#17542,#17543,#17544,#17545,#17546,#17547,#17548,#17549,#17550,
#17551,#17552,#17553,#17554,#17555,#17556),(#17557,#17558,#17559,#17560,
#17561,#17562,#17563,#17564,#17565,#17566,#17567,#17568,#17569,#17570,#17571,
#17572,#17573,#17574,#17575,#17576,#17577,#17578,#17579,#17580,#17581,#17582,
#17583,#17584,#17585,#17586,#17587,#17588,#17589,#17590,#17591,#17592,#17593,
#17594,#17595,#17596,#17597,#17598,#17599,#17600,#17601,#17602,#17603,#17604,
#17605,#17606,#17607,#17608,#17609,#17610,#17611,#17612,#17613,#17614,#17615,
#17616,#17617,#17618,#17619,#17620,#17621,#17622,#17623,#17624,#17625,#17626,
#17627,#17628,#17629,#17630,#17631,#17632,#17633,#17634,#17635,#17636,#17637,
#17638,#17639,#17640,#17641,#17642,#17643,#17644,#17645,#17646,#17647,#17648,
#17649),(#17650,#17651,#17652,#17653,#17654,#17655,#17656,#17657,#17658,
#17659,#17660,#17661,#17662,#17663,#17664,#17665,#17666,#17667,#17668,#17669,
#17670,#17671,#17672,#17673,#17674,#17675,#17676,#17677,#17678,#17679,#17680,
#17681,#17682,#17683,#17684,#17685,#17686,#17687,#17688,#17689,#17690,#17691,
#17692,#17693,#17694,#17695,#17696,#17697,#17698,#17699,#17700,#17701,#17702,
#17703,#17704,#17705,#17706,#17707,#17708,#17709,#17710,#17711,#17712,#17713,
#17714,#17715,#17716,#17717,#17718,#17719,#17720,#17721,#17722,#17723,#17724,
#17725,#17726,#17727,#17728,#17729,#17730,#17731,#17732,#17733,#17734,#17735,
#17736,#17737,#17738,#17739,#17740,#17741,#17742)),.UNSPECIFIED.,.F.,.F.,
 .F.,(4,4),(4,1,1,1,1,1,1,1,1,1,1,1,1,1,1,1,1,1,1,1,1,1,1,1,1,1,1,1,1,1,
1,1,1,1,1,1,1,1,1,1,1,1,1,1,1,1,1,1,1,1,1,1,1,1,1,1,1,1,1,1,1,1,1,1,1,1,
1,1,1,1,1,1,1,1,1,1,1,1,1,1,1,1,1,1,1,1,1,1,1,1,4),(-0.00100526872732246,
0.0646023829588572),(13.6909080459636,14.6908132548486,15.6906081347769,
16.6904030147051,17.6901978946334,18.6899927745616,19.6897876544899,20.6895825344181,
21.6893774143464,22.6891722942746,23.6889671742029,24.6887620541311,25.6885569340594,
26.6883518139876,27.6881466939159,28.6879415738441,29.6877364537724,30.6875313337007,
31.6873262136289,32.6871210935572,33.6869159734854,34.6867108534137,35.6865057333419,
36.6863006132702,37.6860954931984,38.6858903731267,39.6856852530549,40.6854801329832,
41.6852750129114,42.6850698928397,43.6848647727679,44.6846596526962,45.6844545326244,
46.6842494125527,47.6840442924809,48.6838391724092,49.6836340523375,50.6834289322657,
51.683223812194,52.6830186921222,53.6828135720505,54.6826084519787,55.682403331907,
56.6821982118352,57.6819930917635,58.6817879716917,59.68158285162,60.6813777315482,
61.6811726114765,62.6809674914047,63.680762371333,64.6805572512612,65.6803521311895,
66.6801470111178,67.679941891046,68.6797367709743,69.6795316509025,70.6793265308308,
71.679121410759,72.6789162906873,73.6787111706155,74.6785060505438,75.678300930472,
76.6780958104003,77.6778906903285,78.6776855702568,79.677480450185,80.6772753301133,
81.6770702100415,82.6768650899698,83.676659969898,84.6764548498263,85.6762497297545,
86.6760446096828,87.6758394896111,88.6756343695393,89.6754292494676,90.6752241293958,
91.6750190093241,92.6748138892523,93.6746087691806,94.6744036491088,95.6741985290371,
96.6739934089653,97.6737882888936,98.6735831688218,99.6733780487501,100.673172928678,
101.672967808607,102.672762688535,103.67278623601),.UNSPECIFIED.);
#96=B_SPLINE_SURFACE_WITH_KNOTS('',3,3,((#29778,#29779,#29780,#29781,#29782,
#29783,#29784,#29785,#29786,#29787,#29788,#29789,#29790,#29791,#29792,#29793,
#29794,#29795,#29796,#29797,#29798,#29799,#29800,#29801,#29802,#29803,#29804,
#29805,#29806,#29807,#29808,#29809,#29810,#29811,#29812,#29813,#29814,#29815,
#29816,#29817,#29818,#29819,#29820,#29821,#29822,#29823,#29824,#29825,#29826,
#29827,#29828,#29829,#29830,#29831,#29832,#29833,#29834,#29835,#29836,#29837,
#29838,#29839,#29840,#29841,#29842,#29843,#29844,#29845,#29846,#29847,#29848,
#29849,#29850,#29851,#29852,#29853,#29854,#29855,#29856,#29857,#29858,#29859,
#29860,#29861,#29862),(#29863,#29864,#29865,#29866,#29867,#29868,#29869,
#29870,#29871,#29872,#29873,#29874,#29875,#29876,#29877,#29878,#29879,#29880,
#29881,#29882,#29883,#29884,#29885,#29886,#29887,#29888,#29889,#29890,#29891,
#29892,#29893,#29894,#29895,#29896,#29897,#29898,#29899,#29900,#29901,#29902,
#29903,#29904,#29905,#29906,#29907,#29908,#29909,#29910,#29911,#29912,#29913,
#29914,#29915,#29916,#29917,#29918,#29919,#29920,#29921,#29922,#29923,#29924,
#29925,#29926,#29927,#29928,#29929,#29930,#29931,#29932,#29933,#29934,#29935,
#29936,#29937,#29938,#29939,#29940,#29941,#29942,#29943,#29944,#29945,#29946,
#29947),(#29948,#29949,#29950,#29951,#29952,#29953,#29954,#29955,#29956,
#29957,#29958,#29959,#29960,#29961,#29962,#29963,#29964,#29965,#29966,#29967,
#29968,#29969,#29970,#29971,#29972,#29973,#29974,#29975,#29976,#29977,#29978,
#29979,#29980,#29981,#29982,#29983,#29984,#29985,#29986,#29987,#29988,#29989,
#29990,#29991,#29992,#29993,#29994,#29995,#29996,#29997,#29998,#29999,#30000,
#30001,#30002,#30003,#30004,#30005,#30006,#30007,#30008,#30009,#30010,#30011,
#30012,#30013,#30014,#30015,#30016,#30017,#30018,#30019,#30020,#30021,#30022,
#30023,#30024,#30025,#30026,#30027,#30028,#30029,#30030,#30031,#30032),
(#30033,#30034,#30035,#30036,#30037,#30038,#30039,#30040,#30041,#30042,
#30043,#30044,#30045,#30046,#30047,#30048,#30049,#30050,#30051,#30052,#30053,
#30054,#30055,#30056,#30057,#30058,#30059,#30060,#30061,#30062,#30063,#30064,
#30065,#30066,#30067,#30068,#30069,#30070,#30071,#30072,#30073,#30074,#30075,
#30076,#30077,#30078,#30079,#30080,#30081,#30082,#30083,#30084,#30085,#30086,
#30087,#30088,#30089,#30090,#30091,#30092,#30093,#30094,#30095,#30096,#30097,
#30098,#30099,#30100,#30101,#30102,#30103,#30104,#30105,#30106,#30107,#30108,
#30109,#30110,#30111,#30112,#30113,#30114,#30115,#30116,#30117)),
 .UNSPECIFIED.,.F.,.F.,.F.,(4,4),(4,1,1,1,1,1,1,1,1,1,1,1,1,1,1,1,1,1,1,
1,1,1,1,1,1,1,1,1,1,1,1,1,1,1,1,1,1,1,1,1,1,1,1,1,1,1,1,1,1,1,1,1,1,1,1,
1,1,1,1,1,1,1,1,1,1,1,1,1,1,1,1,1,1,1,1,1,1,1,1,1,1,1,4),(-0.000229032876373949,
0.0325052131810458),(10.2100639933856,11.2101668347381,12.2101575453093,
13.2101482558806,14.2101389664519,15.2101296770232,16.2101203875945,17.2101110981658,
18.2101018087371,19.2100925193084,20.2100832298797,21.210073940451,22.2100646510223,
23.2100553615935,24.2100460721648,25.2100367827361,26.2100274933074,27.2100182038787,
28.21000891445,29.2099996250213,30.2099903355926,31.2099810461639,32.2099717567352,
33.2099624673065,34.2099531778778,35.209943888449,36.2099345990203,37.2099253095916,
38.2099160201629,39.2099067307342,40.2098974413055,41.2098881518768,42.2098788624481,
43.2098695730194,44.2098602835907,45.209850994162,46.2098417047333,47.2098324153045,
48.2098231258758,49.2098138364471,50.2098045470184,51.2097952575897,52.209785968161,
53.2097766787323,54.2097673893036,55.2097580998749,56.2097488104462,57.2097395210175,
58.2097302315887,59.20972094216,60.2097116527313,61.2097023633026,62.2096930738739,
63.2096837844452,64.2096744950165,65.2096652055878,66.2096559161591,67.2096466267304,
68.2096373373017,69.209628047873,70.2096187584443,71.2096094690155,72.2096001795868,
73.2095908901581,74.2095816007294,75.2095723113007,76.209563021872,77.2095537324433,
78.2095444430146,79.2095351535859,80.2095258641572,81.2095165747285,82.2095072852998,
83.209497995871,84.2094887064423,85.2094794170136,86.2094701275849,87.2094608381562,
88.2094515487275,89.2094422592988,90.2094329698701,91.2094236804414,92.2094929101791),
 .UNSPECIFIED.);
#97=B_SPLINE_SURFACE_WITH_KNOTS('',3,3,((#30146,#30147,#30148,#30149,#30150,
#30151,#30152,#30153,#30154,#30155,#30156,#30157,#30158,#30159,#30160,#30161,
#30162,#30163,#30164,#30165,#30166,#30167,#30168,#30169,#30170,#30171,#30172,
#30173,#30174,#30175,#30176,#30177,#30178,#30179,#30180,#30181,#30182,#30183,
#30184,#30185,#30186,#30187,#30188,#30189,#30190,#30191,#30192,#30193,#30194,
#30195,#30196,#30197,#30198,#30199,#30200,#30201,#30202,#30203,#30204,#30205,
#30206,#30207,#30208,#30209,#30210,#30211,#30212,#30213,#30214,#30215,#30216,
#30217,#30218,#30219,#30220,#30221,#30222,#30223,#30224,#30225,#30226,#30227,
#30228,#30229,#30230),(#30231,#30232,#30233,#30234,#30235,#30236,#30237,
#30238,#30239,#30240,#30241,#30242,#30243,#30244,#30245,#30246,#30247,#30248,
#30249,#30250,#30251,#30252,#30253,#30254,#30255,#30256,#30257,#30258,#30259,
#30260,#30261,#30262,#30263,#30264,#30265,#30266,#30267,#30268,#30269,#30270,
#30271,#30272,#30273,#30274,#30275,#30276,#30277,#30278,#30279,#30280,#30281,
#30282,#30283,#30284,#30285,#30286,#30287,#30288,#30289,#30290,#30291,#30292,
#30293,#30294,#30295,#30296,#30297,#30298,#30299,#30300,#30301,#30302,#30303,
#30304,#30305,#30306,#30307,#30308,#30309,#30310,#30311,#30312,#30313,#30314,
#30315),(#30316,#30317,#30318,#30319,#30320,#30321,#30322,#30323,#30324,
#30325,#30326,#30327,#30328,#30329,#30330,#30331,#30332,#30333,#30334,#30335,
#30336,#30337,#30338,#30339,#30340,#30341,#30342,#30343,#30344,#30345,#30346,
#30347,#30348,#30349,#30350,#30351,#30352,#30353,#30354,#30355,#30356,#30357,
#30358,#30359,#30360,#30361,#30362,#30363,#30364,#30365,#30366,#30367,#30368,
#30369,#30370,#30371,#30372,#30373,#30374,#30375,#30376,#30377,#30378,#30379,
#30380,#30381,#30382,#30383,#30384,#30385,#30386,#30387,#30388,#30389,#30390,
#30391,#30392,#30393,#30394,#30395,#30396,#30397,#30398,#30399,#30400),
(#30401,#30402,#30403,#30404,#30405,#30406,#30407,#30408,#30409,#30410,
#30411,#30412,#30413,#30414,#30415,#30416,#30417,#30418,#30419,#30420,#30421,
#30422,#30423,#30424,#30425,#30426,#30427,#30428,#30429,#30430,#30431,#30432,
#30433,#30434,#30435,#30436,#30437,#30438,#30439,#30440,#30441,#30442,#30443,
#30444,#30445,#30446,#30447,#30448,#30449,#30450,#30451,#30452,#30453,#30454,
#30455,#30456,#30457,#30458,#30459,#30460,#30461,#30462,#30463,#30464,#30465,
#30466,#30467,#30468,#30469,#30470,#30471,#30472,#30473,#30474,#30475,#30476,
#30477,#30478,#30479,#30480,#30481,#30482,#30483,#30484,#30485)),
 .UNSPECIFIED.,.F.,.F.,.F.,(4,4),(4,1,1,1,1,1,1,1,1,1,1,1,1,1,1,1,1,1,1,
1,1,1,1,1,1,1,1,1,1,1,1,1,1,1,1,1,1,1,1,1,1,1,1,1,1,1,1,1,1,1,1,1,1,1,1,
1,1,1,1,1,1,1,1,1,1,1,1,1,1,1,1,1,1,1,1,1,1,1,1,1,1,1,4),(-0.000337093536336005,
0.0325391625776436),(13.6871942222869,14.6873814867633,15.6873721973346,
16.6873629079059,17.6873536184772,18.6873443290484,19.6873350396197,20.687325750191,
21.6873164607623,22.6873071713336,23.6872978819049,24.6872885924762,25.6872793030475,
26.6872700136188,27.6872607241901,28.6872514347614,29.6872421453326,30.6872328559039,
31.6872235664752,32.6872142770465,33.6872049876178,34.6871956981891,35.6871864087604,
36.6871771193317,37.687167829903,38.6871585404743,39.6871492510456,40.6871399616169,
41.6871306721881,42.6871213827594,43.6871120933307,44.687102803902,45.6870935144733,
46.6870842250446,47.6870749356159,48.6870656461872,49.6870563567585,50.6870470673298,
51.6870377779011,52.6870284884724,53.6870191990436,54.6870099096149,55.6870006201862,
56.6869913307575,57.6869820413288,58.6869727519001,59.6869634624714,60.6869541730427,
61.686944883614,62.6869355941853,63.6869263047566,64.6869170153279,65.6869077258991,
66.6868984364704,67.6868891470417,68.686879857613,69.6868705681843,70.6868612787556,
71.6868519893269,72.6868426998982,73.6868334104695,74.6868241210408,75.6868148316121,
76.6868055421834,77.6867962527546,78.6867869633259,79.6867776738972,80.6867683844685,
81.6867590950398,82.6867498056111,83.6867405161824,84.6867312267537,85.686721937325,
86.6867126478963,87.6867033584676,88.6866940690389,89.6866847796101,90.6866754901814,
91.6866662007527,92.686656911324,93.6866476218953,94.6866383324666,95.6868551020536),
 .UNSPECIFIED.);
#98=B_SPLINE_SURFACE_WITH_KNOTS('',3,3,((#30688,#30689,#30690,#30691,#30692,
#30693,#30694,#30695,#30696,#30697,#30698,#30699,#30700,#30701,#30702,#30703,
#30704,#30705,#30706,#30707,#30708,#30709,#30710,#30711,#30712,#30713,#30714,
#30715,#30716,#30717,#30718,#30719,#30720,#30721,#30722,#30723,#30724,#30725,
#30726,#30727,#30728,#30729,#30730,#30731,#30732,#30733,#30734,#30735,#30736,
#30737,#30738,#30739,#30740,#30741,#30742,#30743,#30744,#30745,#30746,#30747,
#30748,#30749,#30750,#30751,#30752,#30753,#30754,#30755,#30756),(#30757,
#30758,#30759,#30760,#30761,#30762,#30763,#30764,#30765,#30766,#30767,#30768,
#30769,#30770,#30771,#30772,#30773,#30774,#30775,#30776,#30777,#30778,#30779,
#30780,#30781,#30782,#30783,#30784,#30785,#30786,#30787,#30788,#30789,#30790,
#30791,#30792,#30793,#30794,#30795,#30796,#30797,#30798,#30799,#30800,#30801,
#30802,#30803,#30804,#30805,#30806,#30807,#30808,#30809,#30810,#30811,#30812,
#30813,#30814,#30815,#30816,#30817,#30818,#30819,#30820,#30821,#30822,#30823,
#30824,#30825),(#30826,#30827,#30828,#30829,#30830,#30831,#30832,#30833,
#30834,#30835,#30836,#30837,#30838,#30839,#30840,#30841,#30842,#30843,#30844,
#30845,#30846,#30847,#30848,#30849,#30850,#30851,#30852,#30853,#30854,#30855,
#30856,#30857,#30858,#30859,#30860,#30861,#30862,#30863,#30864,#30865,#30866,
#30867,#30868,#30869,#30870,#30871,#30872,#30873,#30874,#30875,#30876,#30877,
#30878,#30879,#30880,#30881,#30882,#30883,#30884,#30885,#30886,#30887,#30888,
#30889,#30890,#30891,#30892,#30893,#30894),(#30895,#30896,#30897,#30898,
#30899,#30900,#30901,#30902,#30903,#30904,#30905,#30906,#30907,#30908,#30909,
#30910,#30911,#30912,#30913,#30914,#30915,#30916,#30917,#30918,#30919,#30920,
#30921,#30922,#30923,#30924,#30925,#30926,#30927,#30928,#30929,#30930,#30931,
#30932,#30933,#30934,#30935,#30936,#30937,#30938,#30939,#30940,#30941,#30942,
#30943,#30944,#30945,#30946,#30947,#30948,#30949,#30950,#30951,#30952,#30953,
#30954,#30955,#30956,#30957,#30958,#30959,#30960,#30961,#30962,#30963)),
 .UNSPECIFIED.,.F.,.F.,.F.,(4,4),(4,1,1,1,1,1,1,1,1,1,1,1,1,1,1,1,1,1,1,
1,1,1,1,1,1,1,1,1,1,1,1,1,1,1,1,1,1,1,1,1,1,1,1,1,1,1,1,1,1,1,1,1,1,1,1,
1,1,1,1,1,1,1,1,1,1,1,4),(-0.000882682909917588,0.0581163152088491),(13.8937860366664,
14.8831634638169,15.8721630239192,16.8611625840214,17.8501621441237,18.8391617042259,
19.8281612643282,20.8171608244304,21.8061603845326,22.7951599446349,23.7841595047371,
24.7731590648394,25.7621586249416,26.7511581850439,27.7401577451461,28.7291573052483,
29.7181568653506,30.7071564254528,31.6961559855551,32.6851555456573,33.6741551057596,
34.6631546658618,35.652154225964,36.6411537860663,37.6301533461685,38.6191529062708,
39.608152466373,40.5971520264753,41.5861515865775,42.5751511466798,43.564150706782,
44.5531502668842,45.5421498269865,46.5311493870887,47.520148947191,48.5091485072932,
49.4981480673955,50.4871476274977,51.4761471875999,52.4651467477022,53.4541463078044,
54.4431458679067,55.4321454280089,56.4211449881112,57.4101445482134,58.3991441083156,
59.3881436684179,60.3771432285201,61.3661427886224,62.3551423487246,63.3441419088269,
64.3331414689291,65.3221410290313,66.3111405891336,67.3001401492358,68.2891397093381,
69.2781392694403,70.2671388295426,71.2561383896448,72.245137949747,73.2341375098493,
74.2231370699515,75.2121366300538,76.201136190156,77.1901357502583,78.1791353103605,
79.1681348704628),.UNSPECIFIED.);
#99=B_SPLINE_SURFACE_WITH_KNOTS('',3,3,((#31557,#31558,#31559,#31560,#31561,
#31562,#31563,#31564,#31565,#31566,#31567,#31568,#31569,#31570,#31571,#31572,
#31573,#31574,#31575,#31576,#31577,#31578,#31579,#31580,#31581,#31582,#31583,
#31584,#31585,#31586,#31587,#31588,#31589,#31590,#31591,#31592,#31593,#31594,
#31595,#31596,#31597,#31598,#31599,#31600,#31601,#31602,#31603,#31604,#31605,
#31606,#31607,#31608,#31609,#31610,#31611,#31612,#31613,#31614,#31615,#31616,
#31617,#31618,#31619,#31620,#31621,#31622,#31623,#31624,#31625),(#31626,
#31627,#31628,#31629,#31630,#31631,#31632,#31633,#31634,#31635,#31636,#31637,
#31638,#31639,#31640,#31641,#31642,#31643,#31644,#31645,#31646,#31647,#31648,
#31649,#31650,#31651,#31652,#31653,#31654,#31655,#31656,#31657,#31658,#31659,
#31660,#31661,#31662,#31663,#31664,#31665,#31666,#31667,#31668,#31669,#31670,
#31671,#31672,#31673,#31674,#31675,#31676,#31677,#31678,#31679,#31680,#31681,
#31682,#31683,#31684,#31685,#31686,#31687,#31688,#31689,#31690,#31691,#31692,
#31693,#31694),(#31695,#31696,#31697,#31698,#31699,#31700,#31701,#31702,
#31703,#31704,#31705,#31706,#31707,#31708,#31709,#31710,#31711,#31712,#31713,
#31714,#31715,#31716,#31717,#31718,#31719,#31720,#31721,#31722,#31723,#31724,
#31725,#31726,#31727,#31728,#31729,#31730,#31731,#31732,#31733,#31734,#31735,
#31736,#31737,#31738,#31739,#31740,#31741,#31742,#31743,#31744,#31745,#31746,
#31747,#31748,#31749,#31750,#31751,#31752,#31753,#31754,#31755,#31756,#31757,
#31758,#31759,#31760,#31761,#31762,#31763),(#31764,#31765,#31766,#31767,
#31768,#31769,#31770,#31771,#31772,#31773,#31774,#31775,#31776,#31777,#31778,
#31779,#31780,#31781,#31782,#31783,#31784,#31785,#31786,#31787,#31788,#31789,
#31790,#31791,#31792,#31793,#31794,#31795,#31796,#31797,#31798,#31799,#31800,
#31801,#31802,#31803,#31804,#31805,#31806,#31807,#31808,#31809,#31810,#31811,
#31812,#31813,#31814,#31815,#31816,#31817,#31818,#31819,#31820,#31821,#31822,
#31823,#31824,#31825,#31826,#31827,#31828,#31829,#31830,#31831,#31832)),
 .UNSPECIFIED.,.F.,.F.,.F.,(4,4),(4,1,1,1,1,1,1,1,1,1,1,1,1,1,1,1,1,1,1,
1,1,1,1,1,1,1,1,1,1,1,1,1,1,1,1,1,1,1,1,1,1,1,1,1,1,1,1,1,1,1,1,1,1,1,1,
1,1,1,1,1,1,1,1,1,1,1,4),(-0.000390001319482014,0.0587333122782212),(10.2099729995397,
11.199175684269,12.1881752443713,13.1771748044735,14.1661743645758,15.155173924678,
16.1441734847802,17.1331730448825,18.1221726049847,19.111172165087,20.1001717251892,
21.0891712852915,22.0781708453937,23.0671704054959,24.0561699655982,25.0451695257004,
26.0341690858027,27.0231686459049,28.0121682060072,29.0011677661094,29.9901673262116,
30.9791668863139,31.9681664464161,32.9571660065184,33.9461655666206,34.9351651267229,
35.9241646868251,36.9131642469273,37.9021638070296,38.8911633671318,39.8801629272341,
40.8691624873363,41.8581620474386,42.8471616075408,43.836161167643,44.8251607277453,
45.8141602878475,46.8031598479498,47.792159408052,48.7811589681543,49.7701585282565,
50.7591580883588,51.748157648461,52.7371572085632,53.7261567686655,54.7151563287677,
55.70415588887,56.6931554489722,57.6821550090744,58.6711545691767,59.6601541292789,
60.6491536893812,61.6381532494834,62.6271528095857,63.6161523696879,64.6051519297902,
65.5941514898924,66.5831510499946,67.5721506100969,68.5611501701991,69.5501497303014,
70.5391492904036,71.5281488505059,72.5171484106081,73.5061479707103,74.4951475308126,
75.484582158383),.UNSPECIFIED.);
#100=B_SPLINE_SURFACE_WITH_KNOTS('',3,3,((#33783,#33784,#33785,#33786,#33787,
#33788,#33789,#33790,#33791,#33792,#33793,#33794,#33795,#33796,#33797,#33798,
#33799,#33800,#33801,#33802,#33803,#33804,#33805,#33806,#33807,#33808,#33809,
#33810,#33811,#33812,#33813,#33814,#33815,#33816,#33817,#33818,#33819,#33820,
#33821,#33822,#33823,#33824,#33825,#33826,#33827,#33828,#33829,#33830,#33831,
#33832,#33833,#33834,#33835,#33836),(#33837,#33838,#33839,#33840,#33841,
#33842,#33843,#33844,#33845,#33846,#33847,#33848,#33849,#33850,#33851,#33852,
#33853,#33854,#33855,#33856,#33857,#33858,#33859,#33860,#33861,#33862,#33863,
#33864,#33865,#33866,#33867,#33868,#33869,#33870,#33871,#33872,#33873,#33874,
#33875,#33876,#33877,#33878,#33879,#33880,#33881,#33882,#33883,#33884,#33885,
#33886,#33887,#33888,#33889,#33890),(#33891,#33892,#33893,#33894,#33895,
#33896,#33897,#33898,#33899,#33900,#33901,#33902,#33903,#33904,#33905,#33906,
#33907,#33908,#33909,#33910,#33911,#33912,#33913,#33914,#33915,#33916,#33917,
#33918,#33919,#33920,#33921,#33922,#33923,#33924,#33925,#33926,#33927,#33928,
#33929,#33930,#33931,#33932,#33933,#33934,#33935,#33936,#33937,#33938,#33939,
#33940,#33941,#33942,#33943,#33944),(#33945,#33946,#33947,#33948,#33949,
#33950,#33951,#33952,#33953,#33954,#33955,#33956,#33957,#33958,#33959,#33960,
#33961,#33962,#33963,#33964,#33965,#33966,#33967,#33968,#33969,#33970,#33971,
#33972,#33973,#33974,#33975,#33976,#33977,#33978,#33979,#33980,#33981,#33982,
#33983,#33984,#33985,#33986,#33987,#33988,#33989,#33990,#33991,#33992,#33993,
#33994,#33995,#33996,#33997,#33998)),.UNSPECIFIED.,.F.,.F.,.F.,(4,4),(4,
1,1,1,1,1,1,1,1,1,1,1,1,1,1,1,1,1,1,1,1,1,1,1,1,1,1,1,1,1,1,1,1,1,1,1,1,
1,1,1,1,1,1,1,1,1,1,1,1,1,1,4),(-0.000427176962040987,0.0325519917386635),
(13.6872368315967,14.6740326940116,15.6606746118312,16.6473165296507,17.6339584474703,
18.6206003652899,19.6072422831094,20.593884200929,21.5805261187486,22.5671680365682,
23.5538099543877,24.5404518722073,25.5270937900269,26.5137357078464,27.500377625666,
28.4870195434856,29.4736614613051,30.4603033791247,31.4469452969443,32.4335872147639,
33.4202291325834,34.406871050403,35.3935129682226,36.3801548860421,37.3667968038617,
38.3534387216813,39.3400806395008,40.3267225573204,41.31336447514,42.3000063929596,
43.2866483107791,44.2732902285987,45.2599321464183,46.2465740642378,47.2332159820574,
48.219857899877,49.2064998176965,50.1931417355161,51.1797836533357,52.1664255711553,
53.1530674889748,54.1397094067944,55.126351324614,56.1129932424335,57.0996351602531,
58.0862770780727,59.0729189958922,60.0595609137118,61.0462028315314,62.032844749351,
63.0194866671705,64.0063577917107),.UNSPECIFIED.);
#101=B_SPLINE_SURFACE_WITH_KNOTS('',3,3,((#34172,#34173,#34174,#34175,#34176,
#34177,#34178,#34179,#34180,#34181,#34182,#34183,#34184,#34185,#34186,#34187,
#34188,#34189,#34190,#34191,#34192,#34193,#34194,#34195,#34196,#34197,#34198,
#34199,#34200,#34201,#34202,#34203,#34204,#34205,#34206,#34207,#34208,#34209,
#34210,#34211,#34212,#34213,#34214,#34215,#34216,#34217,#34218,#34219,#34220,
#34221,#34222,#34223,#34224,#34225),(#34226,#34227,#34228,#34229,#34230,
#34231,#34232,#34233,#34234,#34235,#34236,#34237,#34238,#34239,#34240,#34241,
#34242,#34243,#34244,#34245,#34246,#34247,#34248,#34249,#34250,#34251,#34252,
#34253,#34254,#34255,#34256,#34257,#34258,#34259,#34260,#34261,#34262,#34263,
#34264,#34265,#34266,#34267,#34268,#34269,#34270,#34271,#34272,#34273,#34274,
#34275,#34276,#34277,#34278,#34279),(#34280,#34281,#34282,#34283,#34284,
#34285,#34286,#34287,#34288,#34289,#34290,#34291,#34292,#34293,#34294,#34295,
#34296,#34297,#34298,#34299,#34300,#34301,#34302,#34303,#34304,#34305,#34306,
#34307,#34308,#34309,#34310,#34311,#34312,#34313,#34314,#34315,#34316,#34317,
#34318,#34319,#34320,#34321,#34322,#34323,#34324,#34325,#34326,#34327,#34328,
#34329,#34330,#34331,#34332,#34333),(#34334,#34335,#34336,#34337,#34338,
#34339,#34340,#34341,#34342,#34343,#34344,#34345,#34346,#34347,#34348,#34349,
#34350,#34351,#34352,#34353,#34354,#34355,#34356,#34357,#34358,#34359,#34360,
#34361,#34362,#34363,#34364,#34365,#34366,#34367,#34368,#34369,#34370,#34371,
#34372,#34373,#34374,#34375,#34376,#34377,#34378,#34379,#34380,#34381,#34382,
#34383,#34384,#34385,#34386,#34387)),.UNSPECIFIED.,.F.,.F.,.F.,(4,4),(4,
1,1,1,1,1,1,1,1,1,1,1,1,1,1,1,1,1,1,1,1,1,1,1,1,1,1,1,1,1,1,1,1,1,1,1,1,
1,1,1,1,1,1,1,1,1,1,1,1,1,1,4),(-0.000290371553175226,0.0325162600682668),
(10.2100759344954,11.2038007070197,12.1974252898726,13.1910498727256,14.1846744555785,
15.1782990384314,16.1719236212843,17.1655482041372,18.1591727869901,19.152797369843,
20.146421952696,21.1400465355489,22.1336711184018,23.1272957012547,24.1209202841076,
25.1145448669605,26.1081694498134,27.1017940326664,28.0954186155193,29.0890431983722,
30.0826677812251,31.076292364078,32.0699169469309,33.0635415297839,34.0571661126368,
35.0507906954897,36.0444152783426,37.0380398611955,38.0316644440484,39.0252890269013,
40.0189136097543,41.0125381926072,42.0061627754601,42.999787358313,43.9934119411659,
44.9870365240188,45.9806611068718,46.9742856897247,47.9679102725776,48.9615348554305,
49.9551594382834,50.9487840211363,51.9424086039892,52.9360331868422,53.9296577696951,
54.923282352548,55.9169069354009,56.9105315182538,57.9041561011067,58.8977806839596,
59.8914052668126,60.8850348774998),.UNSPECIFIED.);
#102=B_SPLINE_SURFACE_WITH_KNOTS('',3,3,((#34609,#34610,#34611,#34612,#34613),
(#34614,#34615,#34616,#34617,#34618),(#34619,#34620,#34621,#34622,#34623),
(#34624,#34625,#34626,#34627,#34628)),.UNSPECIFIED.,.F.,.F.,.F.,(4,4),(4,
1,4),(0.,0.032160890827504),(68.4560911973857,69.0589356637105,69.6617801300352),
 .UNSPECIFIED.);
#103=B_SPLINE_SURFACE_WITH_KNOTS('',3,3,((#34647,#34648,#34649,#34650,#34651),
(#34652,#34653,#34654,#34655,#34656),(#34657,#34658,#34659,#34660,#34661),
(#34662,#34663,#34664,#34665,#34666)),.UNSPECIFIED.,.F.,.F.,.F.,(4,4),(4,
1,4),(-9.07170059861442E-6,0.0322908342399317),(61.7440410216514,62.7372907531955,
63.7305404920565),.UNSPECIFIED.);
#104=B_SPLINE_SURFACE_WITH_KNOTS('',3,3,((#34693,#34694,#34695,#34696,#34697),
(#34698,#34699,#34700,#34701,#34702),(#34703,#34704,#34705,#34706,#34707),
(#34708,#34709,#34710,#34711,#34712)),.UNSPECIFIED.,.F.,.F.,.F.,(4,4),(4,
1,4),(-0.000103109978180118,0.0323481470425964),(64.9669593015238,65.8588193203942,
66.7505475116691),.UNSPECIFIED.);
#105=B_SPLINE_SURFACE_WITH_KNOTS('',3,3,((#34737,#34738,#34739,#34740,#34741),
(#34742,#34743,#34744,#34745,#34746),(#34747,#34748,#34749,#34750,#34751),
(#34752,#34753,#34754,#34755,#34756)),.UNSPECIFIED.,.F.,.F.,.F.,(4,4),(4,
1,4),(0.00156261713707751,0.032191282069214),(65.1886793093356,65.9220033054732,
66.6553273016042),.UNSPECIFIED.);
#106=B_SPLINE_SURFACE_WITH_KNOTS('',3,3,((#39360,#39361,#39362,#39363,#39364,
#39365,#39366,#39367,#39368,#39369,#39370,#39371,#39372,#39373,#39374,#39375,
#39376,#39377,#39378,#39379,#39380,#39381,#39382,#39383,#39384,#39385,#39386,
#39387,#39388,#39389,#39390,#39391,#39392,#39393,#39394,#39395,#39396,#39397,
#39398,#39399,#39400,#39401,#39402,#39403,#39404,#39405,#39406,#39407,#39408,
#39409,#39410,#39411,#39412,#39413,#39414,#39415,#39416,#39417,#39418,#39419,
#39420,#39421,#39422,#39423,#39424,#39425,#39426),(#39427,#39428,#39429,
#39430,#39431,#39432,#39433,#39434,#39435,#39436,#39437,#39438,#39439,#39440,
#39441,#39442,#39443,#39444,#39445,#39446,#39447,#39448,#39449,#39450,#39451,
#39452,#39453,#39454,#39455,#39456,#39457,#39458,#39459,#39460,#39461,#39462,
#39463,#39464,#39465,#39466,#39467,#39468,#39469,#39470,#39471,#39472,#39473,
#39474,#39475,#39476,#39477,#39478,#39479,#39480,#39481,#39482,#39483,#39484,
#39485,#39486,#39487,#39488,#39489,#39490,#39491,#39492,#39493),(#39494,
#39495,#39496,#39497,#39498,#39499,#39500,#39501,#39502,#39503,#39504,#39505,
#39506,#39507,#39508,#39509,#39510,#39511,#39512,#39513,#39514,#39515,#39516,
#39517,#39518,#39519,#39520,#39521,#39522,#39523,#39524,#39525,#39526,#39527,
#39528,#39529,#39530,#39531,#39532,#39533,#39534,#39535,#39536,#39537,#39538,
#39539,#39540,#39541,#39542,#39543,#39544,#39545,#39546,#39547,#39548,#39549,
#39550,#39551,#39552,#39553,#39554,#39555,#39556,#39557,#39558,#39559,#39560),
(#39561,#39562,#39563,#39564,#39565,#39566,#39567,#39568,#39569,#39570,
#39571,#39572,#39573,#39574,#39575,#39576,#39577,#39578,#39579,#39580,#39581,
#39582,#39583,#39584,#39585,#39586,#39587,#39588,#39589,#39590,#39591,#39592,
#39593,#39594,#39595,#39596,#39597,#39598,#39599,#39600,#39601,#39602,#39603,
#39604,#39605,#39606,#39607,#39608,#39609,#39610,#39611,#39612,#39613,#39614,
#39615,#39616,#39617,#39618,#39619,#39620,#39621,#39622,#39623,#39624,#39625,
#39626,#39627)),.UNSPECIFIED.,.F.,.F.,.F.,(4,4),(4,1,1,1,1,1,1,1,1,1,1,
1,1,1,1,1,1,1,1,1,1,1,1,1,1,1,1,1,1,1,1,1,1,1,1,1,1,1,1,1,1,1,1,1,1,1,1,
1,1,1,1,1,1,1,1,1,1,1,1,1,1,1,1,1,4),(-0.000386239467008404,0.0586069165862638),
(7.06837814145609,8.05903683580502,9.04949020103305,10.0399435662611,11.0303969314891,
12.0208502967171,13.0113036619452,14.0017570271732,14.9922103924013,15.9826637576293,
16.9731171228573,17.9635704880854,18.9540238533134,19.9444772185414,20.9349305837695,
21.9253839489975,22.9158373142255,23.9062906794536,24.8967440446816,25.8871974099096,
26.8776507751377,27.8681041403657,28.8585575055937,29.8490108708218,30.8394642360498,
31.8299176012778,32.8203709665059,33.8108243317339,34.8012776969619,35.79173106219,
36.782184427418,37.772637792646,38.7630911578741,39.7535445231021,40.7439978883301,
41.7344512535582,42.7249046187862,43.7153579840142,44.7058113492423,45.6962647144703,
46.6867180796983,47.6771714449264,48.6676248101544,49.6580781753824,50.6485315406105,
51.6389849058385,52.6294382710665,53.6198916362946,54.6103450015226,55.6007983667506,
56.5912517319787,57.5817050972067,58.5721584624347,59.5626118276628,60.5530651928908,
61.5435185581188,62.5339719233469,63.5244252885749,64.5148786538029,65.505332019031,
66.495785384259,67.486238749487,68.4766921147151,69.4671454799431,70.4577594577278),
 .UNSPECIFIED.);
#107=B_SPLINE_SURFACE_WITH_KNOTS('',3,3,((#39674,#39675,#39676,#39677,#39678,
#39679,#39680,#39681,#39682,#39683,#39684,#39685,#39686,#39687,#39688,#39689,
#39690,#39691,#39692,#39693,#39694,#39695,#39696,#39697,#39698,#39699,#39700,
#39701,#39702,#39703,#39704,#39705,#39706,#39707,#39708,#39709,#39710,#39711,
#39712,#39713,#39714,#39715,#39716,#39717,#39718,#39719,#39720,#39721,#39722,
#39723,#39724,#39725,#39726,#39727,#39728,#39729,#39730,#39731,#39732,#39733,
#39734,#39735,#39736,#39737,#39738,#39739,#39740),(#39741,#39742,#39743,
#39744,#39745,#39746,#39747,#39748,#39749,#39750,#39751,#39752,#39753,#39754,
#39755,#39756,#39757,#39758,#39759,#39760,#39761,#39762,#39763,#39764,#39765,
#39766,#39767,#39768,#39769,#39770,#39771,#39772,#39773,#39774,#39775,#39776,
#39777,#39778,#39779,#39780,#39781,#39782,#39783,#39784,#39785,#39786,#39787,
#39788,#39789,#39790,#39791,#39792,#39793,#39794,#39795,#39796,#39797,#39798,
#39799,#39800,#39801,#39802,#39803,#39804,#39805,#39806,#39807),(#39808,
#39809,#39810,#39811,#39812,#39813,#39814,#39815,#39816,#39817,#39818,#39819,
#39820,#39821,#39822,#39823,#39824,#39825,#39826,#39827,#39828,#39829,#39830,
#39831,#39832,#39833,#39834,#39835,#39836,#39837,#39838,#39839,#39840,#39841,
#39842,#39843,#39844,#39845,#39846,#39847,#39848,#39849,#39850,#39851,#39852,
#39853,#39854,#39855,#39856,#39857,#39858,#39859,#39860,#39861,#39862,#39863,
#39864,#39865,#39866,#39867,#39868,#39869,#39870,#39871,#39872,#39873,#39874),
(#39875,#39876,#39877,#39878,#39879,#39880,#39881,#39882,#39883,#39884,
#39885,#39886,#39887,#39888,#39889,#39890,#39891,#39892,#39893,#39894,#39895,
#39896,#39897,#39898,#39899,#39900,#39901,#39902,#39903,#39904,#39905,#39906,
#39907,#39908,#39909,#39910,#39911,#39912,#39913,#39914,#39915,#39916,#39917,
#39918,#39919,#39920,#39921,#39922,#39923,#39924,#39925,#39926,#39927,#39928,
#39929,#39930,#39931,#39932,#39933,#39934,#39935,#39936,#39937,#39938,#39939,
#39940,#39941)),.UNSPECIFIED.,.F.,.F.,.F.,(4,4),(4,1,1,1,1,1,1,1,1,1,1,
1,1,1,1,1,1,1,1,1,1,1,1,1,1,1,1,1,1,1,1,1,1,1,1,1,1,1,1,1,1,1,1,1,1,1,1,
1,1,1,1,1,1,1,1,1,1,1,1,1,1,1,1,1,4),(-0.00577350269189626,0.0581188424251775),
(10.7523816656495,11.7430246153529,12.733477980581,13.723931345809,14.714384711037,
15.7048380762651,16.6952914414931,17.6857448067211,18.6761981719492,19.6666515371772,
20.6571049024052,21.6475582676333,22.6380116328613,23.6284649980893,24.6189183633174,
25.6093717285454,26.5998250937734,27.5902784590015,28.5807318242295,29.5711851894575,
30.5616385546856,31.5520919199136,32.5425452851416,33.5329986503697,34.5234520155977,
35.5139053808257,36.5043587460538,37.4948121112818,38.4852654765099,39.4757188417379,
40.4661722069659,41.4566255721939,42.447078937422,43.43753230265,44.4279856678781,
45.4184390331061,46.4088923983341,47.3993457635622,48.3897991287902,49.3802524940182,
50.3707058592463,51.3611592244743,52.3516125897023,53.3420659549304,54.3325193201584,
55.3229726853864,56.3134260506145,57.3038794158425,58.2943327810705,59.2847861462986,
60.2752395115266,61.2656928767546,62.2561462419827,63.2465996072107,64.2370529724387,
65.2275063376668,66.2179597028948,67.2084130681228,68.1988664333509,69.1893197985789,
70.1797731638069,71.170226529035,72.160679894263,73.151133259491,74.1417901888294),
 .UNSPECIFIED.);
#108=B_SPLINE_SURFACE_WITH_KNOTS('',3,3,((#40005,#40006,#40007,#40008,#40009,
#40010,#40011,#40012,#40013,#40014,#40015,#40016,#40017,#40018,#40019,#40020,
#40021,#40022,#40023,#40024,#40025,#40026,#40027,#40028,#40029,#40030,#40031,
#40032,#40033,#40034,#40035,#40036,#40037,#40038,#40039),(#40040,#40041,
#40042,#40043,#40044,#40045,#40046,#40047,#40048,#40049,#40050,#40051,#40052,
#40053,#40054,#40055,#40056,#40057,#40058,#40059,#40060,#40061,#40062,#40063,
#40064,#40065,#40066,#40067,#40068,#40069,#40070,#40071,#40072,#40073,#40074),
(#40075,#40076,#40077,#40078,#40079,#40080,#40081,#40082,#40083,#40084,
#40085,#40086,#40087,#40088,#40089,#40090,#40091,#40092,#40093,#40094,#40095,
#40096,#40097,#40098,#40099,#40100,#40101,#40102,#40103,#40104,#40105,#40106,
#40107,#40108,#40109),(#40110,#40111,#40112,#40113,#40114,#40115,#40116,
#40117,#40118,#40119,#40120,#40121,#40122,#40123,#40124,#40125,#40126,#40127,
#40128,#40129,#40130,#40131,#40132,#40133,#40134,#40135,#40136,#40137,#40138,
#40139,#40140,#40141,#40142,#40143,#40144)),.UNSPECIFIED.,.F.,.F.,.F.,(4,
4),(4,1,1,1,1,1,1,1,1,1,1,1,1,1,1,1,1,1,1,1,1,1,1,1,1,1,1,1,1,1,1,1,4),
(-0.000393287427394601,0.0585773552985969),(7.06836282084679,8.0677424967863,
9.06690152299556,10.0660605492048,11.0652195754141,12.0643786016233,13.0635376278326,
14.0626966540418,15.0618556802511,16.0610147064604,17.0601737326696,18.0593327588789,
19.0584917850881,20.0576508112974,21.0568098375066,22.0559688637159,23.0551278899252,
24.0542869161344,25.0534459423437,26.0526049685529,27.0517639947622,28.0509230209714,
29.0500820471807,30.04924107339,31.0484000995992,32.0475591258085,33.0467181520177,
34.045877178227,35.0450362044363,36.0441952306455,37.0433542568548,38.042513283064,
39.0418309313306),.UNSPECIFIED.);
#109=B_SPLINE_SURFACE_WITH_KNOTS('',3,3,((#40284,#40285,#40286,#40287,#40288,
#40289,#40290,#40291,#40292,#40293,#40294,#40295,#40296,#40297,#40298,#40299,
#40300,#40301,#40302,#40303,#40304,#40305,#40306,#40307,#40308,#40309,#40310,
#40311,#40312,#40313,#40314,#40315,#40316,#40317,#40318),(#40319,#40320,
#40321,#40322,#40323,#40324,#40325,#40326,#40327,#40328,#40329,#40330,#40331,
#40332,#40333,#40334,#40335,#40336,#40337,#40338,#40339,#40340,#40341,#40342,
#40343,#40344,#40345,#40346,#40347,#40348,#40349,#40350,#40351,#40352,#40353),
(#40354,#40355,#40356,#40357,#40358,#40359,#40360,#40361,#40362,#40363,
#40364,#40365,#40366,#40367,#40368,#40369,#40370,#40371,#40372,#40373,#40374,
#40375,#40376,#40377,#40378,#40379,#40380,#40381,#40382,#40383,#40384,#40385,
#40386,#40387,#40388),(#40389,#40390,#40391,#40392,#40393,#40394,#40395,
#40396,#40397,#40398,#40399,#40400,#40401,#40402,#40403,#40404,#40405,#40406,
#40407,#40408,#40409,#40410,#40411,#40412,#40413,#40414,#40415,#40416,#40417,
#40418,#40419,#40420,#40421,#40422,#40423)),.UNSPECIFIED.,.F.,.F.,.F.,(4,
4),(4,1,1,1,1,1,1,1,1,1,1,1,1,1,1,1,1,1,1,1,1,1,1,1,1,1,1,1,1,1,1,1,4),
(-0.000893816201826896,0.0581534486591829),(10.7523808111136,11.7517302763342,
12.7508893025435,13.7500483287527,14.749207354962,15.7483663811713,16.7475254073805,
17.7466844335898,18.745843459799,19.7450024860083,20.7441615122175,21.7433205384268,
22.742479564636,23.7416385908453,24.7407976170546,25.7399566432638,26.7391156694731,
27.7382746956823,28.7374337218916,29.7365927481009,30.7357517743101,31.7349108005194,
32.7340698267286,33.7332288529379,34.7323878791471,35.7315469053564,36.7307059315657,
37.7298649577749,38.7290239839842,39.7281830101934,40.7273420364027,41.7265010626119,
42.7258669660187),.UNSPECIFIED.);
#110=B_SPLINE_SURFACE_WITH_KNOTS('',3,3,((#42024,#42025,#42026,#42027,#42028,
#42029,#42030,#42031,#42032,#42033),(#42034,#42035,#42036,#42037,#42038,
#42039,#42040,#42041,#42042,#42043),(#42044,#42045,#42046,#42047,#42048,
#42049,#42050,#42051,#42052,#42053),(#42054,#42055,#42056,#42057,#42058,
#42059,#42060,#42061,#42062,#42063),(#42064,#42065,#42066,#42067,#42068,
#42069,#42070,#42071,#42072,#42073),(#42074,#42075,#42076,#42077,#42078,
#42079,#42080,#42081,#42082,#42083),(#42084,#42085,#42086,#42087,#42088,
#42089,#42090,#42091,#42092,#42093)),.UNSPECIFIED.,.F.,.T.,.F.,(4,1,1,1,
4),(4,1,1,1,1,1,1,4),(-5.25936583692706E-5,0.285714285714286,0.5,0.785714285714286,
1.0342278679463),(-3.14159265358979,-2.24399475256414,-1.34639685153848,
-0.448798950512828,0.448798950512828,1.34639685153848,2.24399475256414,
3.14159265358979),.UNSPECIFIED.);
#111=B_SPLINE_SURFACE_WITH_KNOTS('',3,3,((#43523,#43524,#43525,#43526,#43527,
#43528,#43529,#43530,#43531,#43532),(#43533,#43534,#43535,#43536,#43537,
#43538,#43539,#43540,#43541,#43542),(#43543,#43544,#43545,#43546,#43547,
#43548,#43549,#43550,#43551,#43552),(#43553,#43554,#43555,#43556,#43557,
#43558,#43559,#43560,#43561,#43562),(#43563,#43564,#43565,#43566,#43567,
#43568,#43569,#43570,#43571,#43572),(#43573,#43574,#43575,#43576,#43577,
#43578,#43579,#43580,#43581,#43582),(#43583,#43584,#43585,#43586,#43587,
#43588,#43589,#43590,#43591,#43592)),.UNSPECIFIED.,.F.,.T.,.F.,(4,1,1,1,
4),(4,1,1,1,1,1,1,4),(0.,0.285714285714286,0.5,0.785714285714286,1.0345115737164),
(-9.42477796076937,-8.52718005974372,-7.62958215871806,-6.73198425769241,
-5.83438635666675,-4.9367884556411,-4.03919055461544,-3.14159265358979),
 .UNSPECIFIED.);
#112=B_SPLINE_SURFACE_WITH_KNOTS('',3,3,((#43768,#43769,#43770,#43771,#43772,
#43773,#43774,#43775,#43776,#43777),(#43778,#43779,#43780,#43781,#43782,
#43783,#43784,#43785,#43786,#43787),(#43788,#43789,#43790,#43791,#43792,
#43793,#43794,#43795,#43796,#43797),(#43798,#43799,#43800,#43801,#43802,
#43803,#43804,#43805,#43806,#43807),(#43808,#43809,#43810,#43811,#43812,
#43813,#43814,#43815,#43816,#43817),(#43818,#43819,#43820,#43821,#43822,
#43823,#43824,#43825,#43826,#43827),(#43828,#43829,#43830,#43831,#43832,
#43833,#43834,#43835,#43836,#43837)),.UNSPECIFIED.,.F.,.T.,.F.,(4,1,1,1,
4),(4,1,1,1,1,1,1,4),(-0.0291943928156984,0.285714285714286,0.571428571428571,
0.785714285714286,1.),(-3.14159265358979,-2.24399475256414,-1.34639685153848,
-0.448798950512828,0.448798950512828,1.34639685153848,2.24399475256414,
3.14159265358979),.UNSPECIFIED.);
#113=B_SPLINE_SURFACE_WITH_KNOTS('',3,3,((#43991,#43992,#43993,#43994,#43995,
#43996,#43997,#43998,#43999,#44000,#44001,#44002,#44003,#44004,#44005,#44006,
#44007,#44008,#44009,#44010,#44011,#44012,#44013,#44014,#44015,#44016,#44017,
#44018,#44019,#44020,#44021,#44022,#44023,#44024,#44025,#44026,#44027,#44028,
#44029,#44030,#44031,#44032),(#44033,#44034,#44035,#44036,#44037,#44038,
#44039,#44040,#44041,#44042,#44043,#44044,#44045,#44046,#44047,#44048,#44049,
#44050,#44051,#44052,#44053,#44054,#44055,#44056,#44057,#44058,#44059,#44060,
#44061,#44062,#44063,#44064,#44065,#44066,#44067,#44068,#44069,#44070,#44071,
#44072,#44073,#44074),(#44075,#44076,#44077,#44078,#44079,#44080,#44081,
#44082,#44083,#44084,#44085,#44086,#44087,#44088,#44089,#44090,#44091,#44092,
#44093,#44094,#44095,#44096,#44097,#44098,#44099,#44100,#44101,#44102,#44103,
#44104,#44105,#44106,#44107,#44108,#44109,#44110,#44111,#44112,#44113,#44114,
#44115,#44116),(#44117,#44118,#44119,#44120,#44121,#44122,#44123,#44124,
#44125,#44126,#44127,#44128,#44129,#44130,#44131,#44132,#44133,#44134,#44135,
#44136,#44137,#44138,#44139,#44140,#44141,#44142,#44143,#44144,#44145,#44146,
#44147,#44148,#44149,#44150,#44151,#44152,#44153,#44154,#44155,#44156,#44157,
#44158)),.UNSPECIFIED.,.F.,.F.,.F.,(4,4),(4,1,1,1,1,1,1,1,1,1,1,1,1,1,1,
1,1,1,1,1,1,1,1,1,1,1,1,1,1,1,1,1,1,1,1,1,1,1,1,4),(-0.000319347032471544,
0.058673081183855),(8.32512525661541,9.30615063831745,10.287080744622,11.2680108509265,
12.248940957231,13.2298710635355,14.21080116984,15.1917312761445,16.172661382449,
17.1535914887535,18.134521595058,19.1154517013625,20.096381807667,21.0773119139715,
22.0582420202761,23.0391721265806,24.0201022328851,25.0010323391896,25.9819624454941,
26.9628925517986,27.9438226581031,28.9247527644076,29.9056828707121,30.8866129770166,
31.8675430833211,32.8484731896256,33.8294032959301,34.8103334022347,35.7912635085392,
36.7721936148437,37.7531237211482,38.7340538274527,39.7149839337572,40.6959140400617,
41.6768441463662,42.6577742526707,43.6387043589752,44.6196344652797,45.6005645715842,
46.5816623403953),.UNSPECIFIED.);
#114=B_SPLINE_SURFACE_WITH_KNOTS('',3,3,((#44258,#44259,#44260,#44261,#44262,
#44263,#44264,#44265,#44266,#44267,#44268,#44269,#44270,#44271,#44272,#44273,
#44274,#44275,#44276,#44277,#44278,#44279,#44280,#44281,#44282,#44283,#44284,
#44285,#44286,#44287,#44288,#44289,#44290,#44291,#44292,#44293,#44294,#44295,
#44296,#44297,#44298,#44299),(#44300,#44301,#44302,#44303,#44304,#44305,
#44306,#44307,#44308,#44309,#44310,#44311,#44312,#44313,#44314,#44315,#44316,
#44317,#44318,#44319,#44320,#44321,#44322,#44323,#44324,#44325,#44326,#44327,
#44328,#44329,#44330,#44331,#44332,#44333,#44334,#44335,#44336,#44337,#44338,
#44339,#44340,#44341),(#44342,#44343,#44344,#44345,#44346,#44347,#44348,
#44349,#44350,#44351,#44352,#44353,#44354,#44355,#44356,#44357,#44358,#44359,
#44360,#44361,#44362,#44363,#44364,#44365,#44366,#44367,#44368,#44369,#44370,
#44371,#44372,#44373,#44374,#44375,#44376,#44377,#44378,#44379,#44380,#44381,
#44382,#44383),(#44384,#44385,#44386,#44387,#44388,#44389,#44390,#44391,
#44392,#44393,#44394,#44395,#44396,#44397,#44398,#44399,#44400,#44401,#44402,
#44403,#44404,#44405,#44406,#44407,#44408,#44409,#44410,#44411,#44412,#44413,
#44414,#44415,#44416,#44417,#44418,#44419,#44420,#44421,#44422,#44423,#44424,
#44425)),.UNSPECIFIED.,.F.,.F.,.F.,(4,4),(4,1,1,1,1,1,1,1,1,1,1,1,1,1,1,
1,1,1,1,1,1,1,1,1,1,1,1,1,1,1,1,1,1,1,1,1,1,1,1,4),(-0.000918461422766351,
0.0581489398467419),(12.0088396942433,12.9901384178654,13.9710685241699,
14.9519986304744,15.9329287367789,16.9138588430834,17.8947889493879,18.8757190556924,
19.8566491619969,20.8375792683014,21.8185093746059,22.7994394809105,23.780369587215,
24.7612996935195,25.742229799824,26.7231599061285,27.704090012433,28.6850201187375,
29.665950225042,30.6468803313465,31.627810437651,32.6087405439555,33.58967065026,
34.5706007565645,35.5515308628691,36.5324609691736,37.5133910754781,38.4943211817826,
39.4752512880871,40.4561813943916,41.4371115006961,42.4180416070006,43.3989717133051,
44.3799018196096,45.3608319259141,46.3417620322186,47.3226921385232,48.3036222448277,
49.2845523511322,50.2660355937093),.UNSPECIFIED.);
#115=B_SPLINE_SURFACE_WITH_KNOTS('',3,3,((#44428,#44429,#44430,#44431,#44432,
#44433),(#44434,#44435,#44436,#44437,#44438,#44439),(#44440,#44441,#44442,
#44443,#44444,#44445),(#44446,#44447,#44448,#44449,#44450,#44451),(#44452,
#44453,#44454,#44455,#44456,#44457),(#44458,#44459,#44460,#44461,#44462,
#44463)),.UNSPECIFIED.,.F.,.F.,.F.,(4,1,1,4),(4,1,1,4),(0.,0.333333333333333,
0.666666666666667,1.00005609897907),(-5.60989790777921E-5,0.333333333333333,
0.666666666666667,1.00005609897908),.UNSPECIFIED.);
#116=B_SPLINE_SURFACE_WITH_KNOTS('',3,3,((#44482,#44483,#44484,#44485,#44486,
#44487),(#44488,#44489,#44490,#44491,#44492,#44493),(#44494,#44495,#44496,
#44497,#44498,#44499),(#44500,#44501,#44502,#44503,#44504,#44505),(#44506,
#44507,#44508,#44509,#44510,#44511),(#44512,#44513,#44514,#44515,#44516,
#44517)),.UNSPECIFIED.,.F.,.F.,.F.,(4,1,1,4),(4,1,1,4),(-5.60989790420212E-5,
0.333333333333333,0.666666666666667,1.00005609897904),(0.,0.333333333333333,
0.666666666666667,1.00005609897904),.UNSPECIFIED.);
#117=B_SPLINE_SURFACE_WITH_KNOTS('',3,3,((#44528,#44529,#44530,#44531,#44532,
#44533),(#44534,#44535,#44536,#44537,#44538,#44539),(#44540,#44541,#44542,
#44543,#44544,#44545),(#44546,#44547,#44548,#44549,#44550,#44551),(#44552,
#44553,#44554,#44555,#44556,#44557),(#44558,#44559,#44560,#44561,#44562,
#44563)),.UNSPECIFIED.,.F.,.F.,.F.,(4,1,1,4),(4,1,1,4),(0.,0.333333333333333,
0.666666666666667,1.00005609897908),(-5.60989790915146E-5,0.333333333333333,
0.666666666666667,1.00005609897909),.UNSPECIFIED.);
#118=B_SPLINE_SURFACE_WITH_KNOTS('',3,3,((#44574,#44575,#44576,#44577,#44578,
#44579),(#44580,#44581,#44582,#44583,#44584,#44585),(#44586,#44587,#44588,
#44589,#44590,#44591),(#44592,#44593,#44594,#44595,#44596,#44597),(#44598,
#44599,#44600,#44601,#44602,#44603),(#44604,#44605,#44606,#44607,#44608,
#44609)),.UNSPECIFIED.,.F.,.F.,.F.,(4,1,1,4),(4,1,1,4),(-5.60989790792135E-5,
0.333333333333333,0.666666666666667,1.00005609897908),(0.,0.333333333333333,
0.666666666666667,1.00005609897907),.UNSPECIFIED.);
#119=B_SPLINE_SURFACE_WITH_KNOTS('',3,3,((#44620,#44621,#44622,#44623,#44624,
#44625),(#44626,#44627,#44628,#44629,#44630,#44631),(#44632,#44633,#44634,
#44635,#44636,#44637),(#44638,#44639,#44640,#44641,#44642,#44643),(#44644,
#44645,#44646,#44647,#44648,#44649),(#44650,#44651,#44652,#44653,#44654,
#44655)),.UNSPECIFIED.,.F.,.F.,.F.,(4,1,1,4),(4,1,1,4),(0.,0.333333333333333,
0.666666666666667,1.00005609897905),(-5.60989790491253E-5,0.333333333333333,
0.666666666666667,1.00005609897905),.UNSPECIFIED.);
#120=B_SPLINE_SURFACE_WITH_KNOTS('',3,3,((#44666,#44667,#44668,#44669,#44670,
#44671),(#44672,#44673,#44674,#44675,#44676,#44677),(#44678,#44679,#44680,
#44681,#44682,#44683),(#44684,#44685,#44686,#44687,#44688,#44689),(#44690,
#44691,#44692,#44693,#44694,#44695),(#44696,#44697,#44698,#44699,#44700,
#44701)),.UNSPECIFIED.,.F.,.F.,.F.,(4,1,1,4),(4,1,1,4),(0.,0.333333333333333,
0.666666666666667,1.00005609897395),(-5.60989810489178E-5,0.333333333333333,
0.666666666666667,1.00005609898105),.UNSPECIFIED.);
#121=B_SPLINE_SURFACE_WITH_KNOTS('',3,3,((#44720,#44721,#44722,#44723,#44724,
#44725),(#44726,#44727,#44728,#44729,#44730,#44731),(#44732,#44733,#44734,
#44735,#44736,#44737),(#44738,#44739,#44740,#44741,#44742,#44743),(#44744,
#44745,#44746,#44747,#44748,#44749),(#44750,#44751,#44752,#44753,#44754,
#44755)),.UNSPECIFIED.,.F.,.F.,.F.,(4,1,1,4),(4,1,1,4),(-5.60989793261701E-5,
0.333333333333333,0.666666666666667,1.00005609897933),(0.,0.333333333333333,
0.666666666666667,1.00005609896406),.UNSPECIFIED.);
#122=B_SPLINE_SURFACE_WITH_KNOTS('',3,3,((#44766,#44767,#44768,#44769,#44770,
#44771),(#44772,#44773,#44774,#44775,#44776,#44777),(#44778,#44779,#44780,
#44781,#44782,#44783),(#44784,#44785,#44786,#44787,#44788,#44789),(#44790,
#44791,#44792,#44793,#44794,#44795),(#44796,#44797,#44798,#44799,#44800,
#44801)),.UNSPECIFIED.,.F.,.F.,.F.,(4,1,1,4),(4,1,1,4),(0.,0.333333333333333,
0.666666666666667,1.00005609897906),(-5.60989790758371E-5,0.333333333333333,
0.666666666666667,1.00005609897907),.UNSPECIFIED.);
#123=B_SPLINE_SURFACE_WITH_KNOTS('',3,3,((#44812,#44813,#44814,#44815,#44816,
#44817),(#44818,#44819,#44820,#44821,#44822,#44823),(#44824,#44825,#44826,
#44827,#44828,#44829),(#44830,#44831,#44832,#44833,#44834,#44835),(#44836,
#44837,#44838,#44839,#44840,#44841),(#44842,#44843,#44844,#44845,#44846,
#44847)),.UNSPECIFIED.,.F.,.F.,.F.,(4,1,1,4),(4,1,1,4),(-5.60989790925808E-5,
0.333333333333333,0.666666666666667,1.00005609897909),(0.,0.333333333333333,
0.666666666666667,1.00005609897908),.UNSPECIFIED.);
#124=B_SPLINE_SURFACE_WITH_KNOTS('',3,3,((#44858,#44859,#44860,#44861,#44862,
#44863),(#44864,#44865,#44866,#44867,#44868,#44869),(#44870,#44871,#44872,
#44873,#44874,#44875),(#44876,#44877,#44878,#44879,#44880,#44881),(#44882,
#44883,#44884,#44885,#44886,#44887),(#44888,#44889,#44890,#44891,#44892,
#44893)),.UNSPECIFIED.,.F.,.F.,.F.,(4,1,1,4),(4,1,1,4),(0.,0.333333333333333,
0.666666666666667,1.00005609896405),(-5.60989793186213E-5,0.333333333333333,
0.666666666666667,1.00005609897932),.UNSPECIFIED.);
#125=B_SPLINE_SURFACE_WITH_KNOTS('',3,3,((#44904,#44905,#44906,#44907,#44908,
#44909),(#44910,#44911,#44912,#44913,#44914,#44915),(#44916,#44917,#44918,
#44919,#44920,#44921),(#44922,#44923,#44924,#44925,#44926,#44927),(#44928,
#44929,#44930,#44931,#44932,#44933),(#44934,#44935,#44936,#44937,#44938,
#44939)),.UNSPECIFIED.,.F.,.F.,.F.,(4,1,1,4),(4,1,1,4),(0.,0.333333333333333,
0.666666666666667,1.00005609896408),(-5.60989793518835E-5,0.333333333333333,
0.666666666666667,1.00005609897935),.UNSPECIFIED.);
#126=B_SPLINE_SURFACE_WITH_KNOTS('',3,3,((#44958,#44959,#44960,#44961,#44962,
#44963),(#44964,#44965,#44966,#44967,#44968,#44969),(#44970,#44971,#44972,
#44973,#44974,#44975),(#44976,#44977,#44978,#44979,#44980,#44981),(#44982,
#44983,#44984,#44985,#44986,#44987),(#44988,#44989,#44990,#44991,#44992,
#44993)),.UNSPECIFIED.,.F.,.F.,.F.,(4,1,1,4),(4,1,1,4),(-5.60989810425424E-5,
0.333333333333333,0.666666666666667,1.00005609898105),(0.,0.333333333333333,
0.666666666666667,1.00005609897395),.UNSPECIFIED.);
#127=B_SPLINE_SURFACE_WITH_KNOTS('',3,3,((#45004,#45005,#45006,#45007,#45008,
#45009),(#45010,#45011,#45012,#45013,#45014,#45015),(#45016,#45017,#45018,
#45019,#45020,#45021),(#45022,#45023,#45024,#45025,#45026,#45027),(#45028,
#45029,#45030,#45031,#45032,#45033),(#45034,#45035,#45036,#45037,#45038,
#45039)),.UNSPECIFIED.,.F.,.F.,.F.,(4,1,1,4),(4,1,1,4),(0.,0.333333333333333,
0.666666666666667,1.00005609897391),(-5.60989809954259E-5,0.333333333333333,
0.666666666666667,1.000056098981),.UNSPECIFIED.);
#128=B_SPLINE_SURFACE_WITH_KNOTS('',3,3,((#45050,#45051,#45052,#45053,#45054,
#45055),(#45056,#45057,#45058,#45059,#45060,#45061),(#45062,#45063,#45064,
#45065,#45066,#45067),(#45068,#45069,#45070,#45071,#45072,#45073),(#45074,
#45075,#45076,#45077,#45078,#45079),(#45080,#45081,#45082,#45083,#45084,
#45085)),.UNSPECIFIED.,.F.,.F.,.F.,(4,1,1,4),(4,1,1,4),(-5.60989793233286E-5,
0.333333333333333,0.666666666666667,1.00005609897932),(0.,0.333333333333333,
0.666666666666667,1.00005609896406),.UNSPECIFIED.);
#129=B_SPLINE_SURFACE_WITH_KNOTS('',3,3,((#45096,#45097,#45098,#45099,#45100,
#45101),(#45102,#45103,#45104,#45105,#45106,#45107),(#45108,#45109,#45110,
#45111,#45112,#45113),(#45114,#45115,#45116,#45117,#45118,#45119),(#45120,
#45121,#45122,#45123,#45124,#45125),(#45126,#45127,#45128,#45129,#45130,
#45131)),.UNSPECIFIED.,.F.,.F.,.F.,(4,1,1,4),(4,1,1,4),(0.,0.333333333333333,
0.666666666666667,1.0000560989791),(-5.60989791002414E-5,0.333333333333333,
0.666666666666667,1.0000560989791),.UNSPECIFIED.);
#130=B_SPLINE_SURFACE_WITH_KNOTS('',3,3,((#45142,#45143,#45144,#45145,#45146,
#45147),(#45148,#45149,#45150,#45151,#45152,#45153),(#45154,#45155,#45156,
#45157,#45158,#45159),(#45160,#45161,#45162,#45163,#45164,#45165),(#45166,
#45167,#45168,#45169,#45170,#45171),(#45172,#45173,#45174,#45175,#45176,
#45177)),.UNSPECIFIED.,.F.,.F.,.F.,(4,1,1,4),(4,1,1,4),(0.,0.333333333333333,
0.666666666666667,1.00005609896409),(-5.60989793533921E-5,0.333333333333333,
0.666666666666667,1.00005609897935),.UNSPECIFIED.);
#131=B_SPLINE_SURFACE_WITH_KNOTS('',3,3,((#45196,#45197,#45198,#45199,#45200,
#45201),(#45202,#45203,#45204,#45205,#45206,#45207),(#45208,#45209,#45210,
#45211,#45212,#45213),(#45214,#45215,#45216,#45217,#45218,#45219),(#45220,
#45221,#45222,#45223,#45224,#45225),(#45226,#45227,#45228,#45229,#45230,
#45231)),.UNSPECIFIED.,.F.,.F.,.F.,(4,1,1,4),(4,1,1,4),(-5.60989810493619E-5,
0.333333333333333,0.666666666666667,1.00005609898105),(0.,0.333333333333333,
0.666666666666667,1.00005609897395),.UNSPECIFIED.);
#132=B_SPLINE_SURFACE_WITH_KNOTS('',3,3,((#45242,#45243,#45244,#45245,#45246,
#45247),(#45248,#45249,#45250,#45251,#45252,#45253),(#45254,#45255,#45256,
#45257,#45258,#45259),(#45260,#45261,#45262,#45263,#45264,#45265),(#45266,
#45267,#45268,#45269,#45270,#45271),(#45272,#45273,#45274,#45275,#45276,
#45277)),.UNSPECIFIED.,.F.,.F.,.F.,(4,1,1,4),(4,1,1,4),(0.,0.333333333333333,
0.666666666666667,1.00005609895074),(-5.60989812701836E-5,0.333333333333333,
0.666666666666667,1.00005609898127),.UNSPECIFIED.);
#133=B_SPLINE_SURFACE_WITH_KNOTS('',3,3,((#45288,#45289,#45290,#45291,#45292,
#45293),(#45294,#45295,#45296,#45297,#45298,#45299),(#45300,#45301,#45302,
#45303,#45304,#45305),(#45306,#45307,#45308,#45309,#45310,#45311),(#45312,
#45313,#45314,#45315,#45316,#45317),(#45318,#45319,#45320,#45321,#45322,
#45323)),.UNSPECIFIED.,.F.,.F.,.F.,(4,1,1,4),(4,1,1,4),(-5.60989812733151E-5,
0.333333333333333,0.666666666666667,1.00005609898127),(0.,0.333333333333333,
0.666666666666667,1.00005609895075),.UNSPECIFIED.);
#134=B_SPLINE_SURFACE_WITH_KNOTS('',3,3,((#45334,#45335,#45336,#45337,#45338,
#45339),(#45340,#45341,#45342,#45343,#45344,#45345),(#45346,#45347,#45348,
#45349,#45350,#45351),(#45352,#45353,#45354,#45355,#45356,#45357),(#45358,
#45359,#45360,#45361,#45362,#45363),(#45364,#45365,#45366,#45367,#45368,
#45369)),.UNSPECIFIED.,.F.,.F.,.F.,(4,1,1,4),(4,1,1,4),(0.,0.333333333333333,
0.666666666666667,1.00005609897395),(-5.60989810488734E-5,0.333333333333333,
0.666666666666667,1.00005609898105),.UNSPECIFIED.);
#135=B_SPLINE_SURFACE_WITH_KNOTS('',3,3,((#45380,#45381,#45382,#45383,#45384,
#45385),(#45386,#45387,#45388,#45389,#45390,#45391),(#45392,#45393,#45394,
#45395,#45396,#45397),(#45398,#45399,#45400,#45401,#45402,#45403),(#45404,
#45405,#45406,#45407,#45408,#45409),(#45410,#45411,#45412,#45413,#45414,
#45415)),.UNSPECIFIED.,.F.,.F.,.F.,(4,1,1,4),(4,1,1,4),(-5.60989793545037E-5,
0.333333333333333,0.666666666666667,1.00005609897935),(0.,0.333333333333333,
0.666666666666667,1.00005609896409),.UNSPECIFIED.);
#136=B_SPLINE_SURFACE_WITH_KNOTS('',3,3,((#45425,#45426,#45427,#45428,#45429,
#45430),(#45431,#45432,#45433,#45434,#45435,#45436),(#45437,#45438,#45439,
#45440,#45441,#45442),(#45443,#45444,#45445,#45446,#45447,#45448),(#45449,
#45450,#45451,#45452,#45453,#45454),(#45455,#45456,#45457,#45458,#45459,
#45460)),.UNSPECIFIED.,.F.,.F.,.F.,(4,1,1,4),(4,1,1,4),(-5.60989790782798E-5,
0.333333333333333,0.666666666666667,1.00005609897908),(0.,0.333333333333333,
0.666666666666667,1.00005609897908),.UNSPECIFIED.);
#137=B_SPLINE_SURFACE_WITH_KNOTS('',3,3,((#45473,#45474,#45475,#45476,#45477,
#45478),(#45479,#45480,#45481,#45482,#45483,#45484),(#45485,#45486,#45487,
#45488,#45489,#45490),(#45491,#45492,#45493,#45494,#45495,#45496),(#45497,
#45498,#45499,#45500,#45501,#45502),(#45503,#45504,#45505,#45506,#45507,
#45508)),.UNSPECIFIED.,.F.,.F.,.F.,(4,1,1,4),(4,1,1,4),(-5.60989810261355E-5,
0.333333333333333,0.666666666666667,1.00005609898103),(0.,0.333333333333333,
0.666666666666667,1.00005609897399),.UNSPECIFIED.);
#138=B_SPLINE_SURFACE_WITH_KNOTS('',3,3,((#45518,#45519,#45520,#45521,#45522,
#45523),(#45524,#45525,#45526,#45527,#45528,#45529),(#45530,#45531,#45532,
#45533,#45534,#45535),(#45536,#45537,#45538,#45539,#45540,#45541),(#45542,
#45543,#45544,#45545,#45546,#45547),(#45548,#45549,#45550,#45551,#45552,
#45553)),.UNSPECIFIED.,.F.,.F.,.F.,(4,1,1,4),(4,1,1,4),(-5.6098979101063E-5,
0.333333333333333,0.666666666666667,1.0000560989791),(0.,0.333333333333333,
0.666666666666667,1.0000560989791),.UNSPECIFIED.);
#139=B_SPLINE_SURFACE_WITH_KNOTS('',3,3,((#49898,#49899,#49900,#49901,#49902,
#49903,#49904,#49905,#49906,#49907,#49908,#49909,#49910,#49911),(#49912,
#49913,#49914,#49915,#49916,#49917,#49918,#49919,#49920,#49921,#49922,#49923,
#49924,#49925),(#49926,#49927,#49928,#49929,#49930,#49931,#49932,#49933,
#49934,#49935,#49936,#49937,#49938,#49939),(#49940,#49941,#49942,#49943,
#49944,#49945,#49946,#49947,#49948,#49949,#49950,#49951,#49952,#49953)),
 .UNSPECIFIED.,.F.,.F.,.F.,(4,4),(4,1,1,1,1,1,1,1,1,1,1,4),(-0.000475468026429485,
0.0667497669206857),(7.06827384690996,8.03224682715675,8.99591018373647,
9.95957354031619,10.9232368968959,11.8869002534756,12.8505636100553,13.8142269666351,
14.7778903232148,15.7415536797945,16.7052170363742,17.6690343848084),
 .UNSPECIFIED.);
#140=B_SPLINE_SURFACE_WITH_KNOTS('',3,3,((#49960,#49961,#49962,#49963,#49964,
#49965,#49966,#49967,#49968,#49969,#49970,#49971,#49972,#49973),(#49974,
#49975,#49976,#49977,#49978,#49979,#49980,#49981,#49982,#49983,#49984,#49985,
#49986,#49987),(#49988,#49989,#49990,#49991,#49992,#49993,#49994,#49995,
#49996,#49997,#49998,#49999,#50000,#50001),(#50002,#50003,#50004,#50005,
#50006,#50007,#50008,#50009,#50010,#50011,#50012,#50013,#50014,#50015)),
 .UNSPECIFIED.,.F.,.F.,.F.,(4,4),(4,1,1,1,1,1,1,1,1,1,1,4),(-0.000976054051980672,
0.0662815922873265),(10.4983829434381,11.4623026957119,12.4259660522916,
13.3896294088713,14.353292765451,15.3169561220308,16.2806194786105,17.2442828351902,
18.2079461917699,19.1716095483496,20.1352729049293,21.0993547069101),
 .UNSPECIFIED.);
#141=B_SPLINE_CURVE_WITH_KNOTS('',3,(#13868,#13869,#13870,#13871,#13872,
#13873,#13874,#13875,#13876,#13877,#13878,#13879,#13880,#13881,#13882,#13883,
#13884,#13885,#13886,#13887,#13888,#13889,#13890,#13891,#13892,#13893,#13894,
#13895,#13896,#13897,#13898,#13899,#13900,#13901,#13902,#13903,#13904,#13905,
#13906,#13907,#13908,#13909,#13910,#13911,#13912,#13913,#13914,#13915,#13916,
#13917,#13918,#13919,#13920,#13921,#13922,#13923,#13924,#13925,#13926,#13927,
#13928,#13929,#13930,#13931,#13932,#13933,#13934),.UNSPECIFIED.,.F.,.F.,
(4,3,3,3,3,3,3,3,3,3,3,3,3,3,3,3,3,3,3,3,3,3,4),(1.25156093680116E-6,0.0883500955934641,
0.103030521980099,0.125,0.211544670578705,0.25,0.26221619397553,0.334021572169558,
0.375,0.421693572098901,0.485226135902788,0.5,0.5625,0.577874060665358,
0.625,0.710303391755808,0.734738255635071,0.75,0.836904432795506,0.875,
0.895553090245324,0.965961016411946,0.99999868984544),.UNSPECIFIED.);
#142=B_SPLINE_CURVE_WITH_KNOTS('',3,(#13936,#13937,#13938,#13939,#13940,
#13941,#13942,#13943,#13944,#13945,#13946,#13947,#13948,#13949,#13950,#13951,
#13952,#13953,#13954,#13955,#13956,#13957,#13958,#13959,#13960,#13961,#13962,
#13963,#13964,#13965,#13966,#13967,#13968,#13969,#13970,#13971,#13972,#13973,
#13974,#13975,#13976,#13977,#13978,#13979,#13980,#13981,#13982,#13983,#13984),
 .UNSPECIFIED.,.F.,.F.,(4,3,3,3,3,3,3,3,3,3,3,3,3,3,3,3,4),(0.,0.0880924990179859,
0.125,0.211469534154412,0.25,0.336789345136967,0.375,0.461773033582195,
0.5,0.586773033582203,0.625,0.711789345136965,0.75,0.836469534154423,0.875,
0.963092499017944,1.),.UNSPECIFIED.);
#143=B_SPLINE_CURVE_WITH_KNOTS('',3,(#13986,#13987,#13988,#13989,#13990,
#13991,#13992,#13993,#13994,#13995,#13996,#13997,#13998,#13999,#14000,#14001,
#14002,#14003,#14004,#14005,#14006,#14007,#14008,#14009,#14010,#14011,#14012,
#14013,#14014,#14015,#14016,#14017,#14018,#14019,#14020,#14021,#14022,#14023,
#14024,#14025,#14026,#14027,#14028,#14029,#14030,#14031,#14032,#14033,#14034),
 .UNSPECIFIED.,.F.,.F.,(4,3,3,3,3,3,3,3,3,3,3,3,3,3,3,3,4),(0.,0.0881024108360804,
0.125,0.211479598204264,0.25,0.336799405951737,0.375,0.461783076602685,
0.5,0.586783076602703,0.625,0.711799405951738,0.75,0.836479598204259,0.875,
0.963102410836136,1.),.UNSPECIFIED.);
#144=B_SPLINE_CURVE_WITH_KNOTS('',3,(#14036,#14037,#14038,#14039,#14040,
#14041,#14042,#14043,#14044,#14045,#14046,#14047,#14048,#14049,#14050,#14051,
#14052,#14053,#14054,#14055,#14056,#14057,#14058,#14059,#14060,#14061,#14062,
#14063,#14064,#14065,#14066,#14067,#14068,#14069,#14070,#14071,#14072,#14073,
#14074,#14075,#14076,#14077,#14078,#14079,#14080,#14081,#14082,#14083,#14084),
 .UNSPECIFIED.,.F.,.F.,(4,3,3,3,3,3,3,3,3,3,3,3,3,3,3,3,4),(0.,0.0880833098674038,
0.125,0.211460203849926,0.25,0.336780017823431,0.375,0.461763722773403,
0.5,0.586763722773395,0.625,0.71178001782344,0.75,0.836460203849939,0.875,
0.963083309867389,1.),.UNSPECIFIED.);
#145=B_SPLINE_CURVE_WITH_KNOTS('',3,(#14086,#14087,#14088,#14089,#14090,
#14091,#14092,#14093,#14094,#14095,#14096,#14097,#14098,#14099,#14100,#14101,
#14102,#14103,#14104,#14105,#14106,#14107,#14108,#14109,#14110,#14111,#14112,
#14113,#14114,#14115,#14116,#14117,#14118,#14119,#14120,#14121,#14122,#14123,
#14124,#14125,#14126,#14127,#14128,#14129,#14130,#14131,#14132,#14133,#14134),
 .UNSPECIFIED.,.F.,.F.,(4,3,3,3,3,3,3,3,3,3,3,3,3,3,3,3,4),(1.38656343410957E-7,
0.0880826036576598,0.125,0.211459358145887,0.25,0.336779172390087,0.375,
0.461762878836428,0.5,0.586762878836416,0.625,0.711779172390097,0.75,0.836459358145886,
0.875,0.963082476958599,1.),.UNSPECIFIED.);
#146=B_SPLINE_CURVE_WITH_KNOTS('',3,(#14136,#14137,#14138,#14139,#14140,
#14141,#14142,#14143,#14144,#14145,#14146,#14147,#14148,#14149,#14150,#14151,
#14152,#14153,#14154,#14155,#14156,#14157,#14158,#14159,#14160,#14161,#14162,
#14163,#14164,#14165,#14166,#14167,#14168,#14169,#14170,#14171,#14172,#14173,
#14174,#14175,#14176,#14177,#14178,#14179,#14180,#14181,#14182,#14183,#14184),
 .UNSPECIFIED.,.F.,.F.,(4,3,3,3,3,3,3,3,3,3,3,3,3,3,3,3,4),(0.,0.0881011169934676,
0.125,0.211478284491326,0.25,0.336798092661633,0.375,0.461781765634862,
0.5,0.586781765634871,0.625,0.711798092661628,0.75,0.836478284491337,0.875,
0.963101116993472,1.),.UNSPECIFIED.);
#147=B_SPLINE_CURVE_WITH_KNOTS('',3,(#14186,#14187,#14188,#14189,#14190,
#14191,#14192,#14193,#14194,#14195,#14196,#14197,#14198,#14199,#14200,#14201,
#14202,#14203,#14204,#14205,#14206,#14207,#14208,#14209,#14210,#14211,#14212,
#14213,#14214,#14215,#14216,#14217,#14218,#14219,#14220,#14221,#14222,#14223,
#14224,#14225,#14226,#14227,#14228,#14229,#14230,#14231,#14232,#14233,#14234),
 .UNSPECIFIED.,.F.,.F.,(4,3,3,3,3,3,3,3,3,3,3,3,3,3,3,3,4),(0.,0.0880934980383074,
0.125,0.211470548519371,0.25,0.336790359176268,0.375,0.461774045827613,
0.5,0.586774045827619,0.625,0.711790359176272,0.75,0.836470548519377,0.875,
0.963093498038292,1.),.UNSPECIFIED.);
#148=B_SPLINE_CURVE_WITH_KNOTS('',3,(#14236,#14237,#14238,#14239,#14240,
#14241,#14242,#14243,#14244,#14245,#14246,#14247,#14248,#14249,#14250,#14251,
#14252,#14253,#14254,#14255,#14256,#14257,#14258,#14259,#14260,#14261,#14262,
#14263,#14264,#14265,#14266,#14267,#14268,#14269,#14270,#14271,#14272,#14273,
#14274,#14275,#14276,#14277,#14278,#14279,#14280,#14281,#14282,#14283,#14284),
 .UNSPECIFIED.,.F.,.F.,(4,3,3,3,3,3,3,3,3,3,3,3,3,3,3,3,4),(1.23038810336374E-6,
0.0880827430507262,0.125,0.211461811736442,0.25,0.336784839496599,0.375,
0.461710040665769,0.5,0.586886602165314,0.625,0.711701462151024,0.75,0.836461636546894,
0.875,0.963080200121549,0.999998752114935),.UNSPECIFIED.);
#149=B_SPLINE_CURVE_WITH_KNOTS('',3,(#14286,#14287,#14288,#14289,#14290,
#14291,#14292,#14293,#14294,#14295,#14296,#14297,#14298,#14299,#14300,#14301,
#14302,#14303,#14304,#14305,#14306,#14307,#14308,#14309,#14310,#14311,#14312,
#14313,#14314,#14315,#14316,#14317,#14318,#14319,#14320,#14321,#14322,#14323,
#14324,#14325,#14326,#14327,#14328,#14329,#14330,#14331,#14332,#14333,#14334),
 .UNSPECIFIED.,.F.,.F.,(4,3,3,3,3,3,3,3,3,3,3,3,3,3,3,3,4),(0.,0.0880920072316036,
0.125,0.211469034814287,0.25,0.336788845957097,0.375,0.46177253528545,0.5,
0.586772535285452,0.625,0.711788845957101,0.75,0.836469034814284,0.875,
0.963092007231635,1.),.UNSPECIFIED.);
#150=B_SPLINE_CURVE_WITH_KNOTS('',3,(#14336,#14337,#14338,#14339,#14340,
#14341,#14342,#14343,#14344,#14345,#14346,#14347,#14348,#14349,#14350,#14351,
#14352,#14353,#14354,#14355,#14356,#14357,#14358,#14359,#14360,#14361,#14362,
#14363,#14364,#14365,#14366,#14367,#14368,#14369,#14370,#14371,#14372,#14373,
#14374,#14375,#14376,#14377,#14378,#14379,#14380,#14381,#14382,#14383,#14384),
 .UNSPECIFIED.,.F.,.F.,(4,3,3,3,3,3,3,3,3,3,3,3,3,3,3,3,4),(0.,0.0881029814297449,
0.125,0.211480177560658,0.25,0.33679998512162,0.375,0.461783654748482,0.5,
0.586783654748484,0.625,0.711799985121625,0.75,0.836480177560661,0.875,
0.963102981429744,1.),.UNSPECIFIED.);
#151=B_SPLINE_CURVE_WITH_KNOTS('',3,(#14386,#14387,#14388,#14389,#14390,
#14391,#14392),.UNSPECIFIED.,.F.,.F.,(4,1,1,1,4),(0.,0.25,0.5,0.75,1.),
 .UNSPECIFIED.);
#152=B_SPLINE_CURVE_WITH_KNOTS('',3,(#14396,#14397,#14398,#14399,#14400,
#14401,#14402,#14403,#14404,#14405,#14406,#14407,#14408,#14409,#14410,#14411,
#14412,#14413,#14414,#14415,#14416,#14417,#14418,#14419,#14420,#14421,#14422,
#14423,#14424,#14425,#14426,#14427,#14428,#14429,#14430,#14431,#14432),
 .UNSPECIFIED.,.F.,.F.,(4,3,3,3,3,3,3,3,3,3,3,3,4),(0.,0.125,0.23032997709698,
0.25,0.375,0.46468733129745,0.5,0.625,0.699111355030774,0.75,0.875,0.933549171352441,
1.),.UNSPECIFIED.);
#153=B_SPLINE_CURVE_WITH_KNOTS('',3,(#14434,#14435,#14436,#14437,#14438,
#14439,#14440,#14441,#14442,#14443,#14444,#14445,#14446,#14447,#14448,#14449,
#14450,#14451,#14452,#14453,#14454,#14455,#14456,#14457,#14458,#14459,#14460,
#14461,#14462,#14463,#14464,#14465,#14466,#14467,#14468,#14469,#14470,#14471,
#14472,#14473,#14474,#14475,#14476,#14477,#14478,#14479,#14480,#14481,#14482),
 .UNSPECIFIED.,.F.,.F.,(4,3,3,3,3,3,3,3,3,3,3,3,3,3,3,3,4),(7.72207807885717E-7,
0.0880871484364614,0.125,0.211463406241229,0.25,0.336781091047344,0.375,
0.461774857659637,0.5,0.586773708011755,0.625,0.711753540165089,0.75,0.836456686852539,
0.875,0.963077282795441,0.999999115125707),.UNSPECIFIED.);
#154=B_SPLINE_CURVE_WITH_KNOTS('',3,(#14484,#14485,#14486,#14487,#14488,
#14489,#14490,#14491,#14492,#14493,#14494,#14495,#14496,#14497,#14498,#14499,
#14500,#14501,#14502,#14503,#14504,#14505,#14506,#14507,#14508,#14509,#14510,
#14511,#14512,#14513,#14514,#14515,#14516,#14517,#14518,#14519,#14520,#14521,
#14522,#14523,#14524,#14525,#14526,#14527,#14528,#14529,#14530,#14531,#14532),
 .UNSPECIFIED.,.F.,.F.,(4,3,3,3,3,3,3,3,3,3,3,3,3,3,3,3,4),(0.,0.088088017626471,
0.125,0.211464983927167,0.25,0.336784796369337,0.375,0.461768492862693,
0.5,0.586768492862716,0.625,0.711784796369325,0.75,0.836464983927168,0.875,
0.96308801762646,1.),.UNSPECIFIED.);
#155=B_SPLINE_CURVE_WITH_KNOTS('',3,(#14534,#14535,#14536,#14537,#14538,
#14539,#14540,#14541,#14542,#14543,#14544,#14545,#14546,#14547,#14548,#14549,
#14550,#14551,#14552,#14553,#14554,#14555,#14556,#14557,#14558,#14559,#14560,
#14561,#14562,#14563,#14564,#14565,#14566,#14567,#14568,#14569,#14570,#14571,
#14572,#14573,#14574,#14575,#14576,#14577,#14578,#14579,#14580,#14581,#14582),
 .UNSPECIFIED.,.F.,.F.,(4,3,3,3,3,3,3,3,3,3,3,3,3,3,3,3,4),(0.,0.0881042788052708,
0.125,0.211481494860136,0.25,0.336801301996907,0.375,0.461784969295354,
0.5,0.586784969295344,0.625,0.711801301996906,0.75,0.836481494860131,0.875,
0.963104278805279,1.),.UNSPECIFIED.);
#156=B_SPLINE_CURVE_WITH_KNOTS('',3,(#14584,#14585,#14586,#14587,#14588,
#14589,#14590,#14591,#14592,#14593,#14594,#14595,#14596,#14597,#14598,#14599,
#14600,#14601,#14602,#14603,#14604,#14605,#14606,#14607,#14608,#14609,#14610,
#14611,#14612,#14613,#14614,#14615,#14616,#14617,#14618,#14619,#14620,#14621,
#14622,#14623,#14624,#14625,#14626,#14627,#14628,#14629,#14630,#14631,#14632),
 .UNSPECIFIED.,.F.,.F.,(4,3,3,3,3,3,3,3,3,3,3,3,3,3,3,3,4),(0.,0.0880886602034345,
0.125,0.211465636374609,0.25,0.336785448607603,0.375,0.461769143946861,
0.5,0.586769143946859,0.625,0.711785448607598,0.75,0.83646563637461,0.875,
0.963088660203419,1.),.UNSPECIFIED.);
#157=B_SPLINE_CURVE_WITH_KNOTS('',3,(#14634,#14635,#14636,#14637,#14638,
#14639,#14640,#14641,#14642,#14643,#14644,#14645,#14646,#14647,#14648,#14649,
#14650,#14651,#14652,#14653,#14654,#14655,#14656,#14657,#14658,#14659,#14660,
#14661,#14662,#14663,#14664,#14665,#14666,#14667,#14668,#14669,#14670,#14671,
#14672,#14673,#14674,#14675,#14676,#14677,#14678,#14679,#14680,#14681,#14682,
#14683,#14684,#14685,#14686,#14687,#14688,#14689,#14690,#14691,#14692,#14693,
#14694,#14695,#14696,#14697,#14698,#14699,#14700,#14701,#14702,#14703,#14704,
#14705,#14706,#14707,#14708,#14709),.UNSPECIFIED.,.F.,.F.,(4,3,3,3,3,3,
3,3,3,3,3,3,3,3,3,3,3,3,3,3,3,3,3,3,3,4),(9.70948605131889E-7,0.0875075598981359,
0.125,0.211923873410919,0.25,0.3125,0.375,0.40625,0.4375,0.46875,0.484375,
0.4921875,0.5,0.5078125,0.515625,0.53125,0.5625,0.59375,0.625,0.6875,0.75,
0.8125,0.875,0.9375,0.995806240197456,0.999999425592883),.UNSPECIFIED.);
#158=B_SPLINE_CURVE_WITH_KNOTS('',3,(#14711,#14712,#14713,#14714,#14715,
#14716,#14717,#14718,#14719,#14720,#14721,#14722,#14723,#14724,#14725,#14726,
#14727,#14728,#14729,#14730,#14731,#14732,#14733,#14734,#14735,#14736,#14737,
#14738,#14739,#14740,#14741,#14742,#14743,#14744,#14745,#14746,#14747,#14748,
#14749,#14750,#14751,#14752,#14753,#14754,#14755,#14756,#14757,#14758,#14759),
 .UNSPECIFIED.,.F.,.F.,(4,3,3,3,3,3,3,3,3,3,3,3,3,3,3,3,4),(0.,0.088095309895002,
0.125,0.211472388204989,0.25,0.336792198271045,0.375,0.461775881669146,
0.5,0.586775881669135,0.625,0.711792198271046,0.75,0.836472388204994,0.875,
0.963095309894954,1.),.UNSPECIFIED.);
#159=B_SPLINE_CURVE_WITH_KNOTS('',3,(#14761,#14762,#14763,#14764,#14765,
#14766,#14767,#14768,#14769,#14770,#14771,#14772,#14773,#14774,#14775,#14776,
#14777,#14778,#14779,#14780,#14781,#14782,#14783,#14784,#14785,#14786,#14787,
#14788,#14789,#14790,#14791,#14792,#14793,#14794,#14795,#14796,#14797,#14798,
#14799,#14800,#14801,#14802,#14803,#14804,#14805,#14806,#14807,#14808,#14809),
 .UNSPECIFIED.,.F.,.F.,(4,3,3,3,3,3,3,3,3,3,3,3,3,3,3,3,4),(0.,0.088096458191059,
0.125,0.211473554137782,0.25,0.336793363829213,0.375,0.461777045165672,
0.5,0.586777045165651,0.625,0.711793363829219,0.75,0.836473554137771,0.875,
0.963096458191102,1.),.UNSPECIFIED.);
#160=B_SPLINE_CURVE_WITH_KNOTS('',3,(#14811,#14812,#14813,#14814,#14815,
#14816,#14817,#14818,#14819,#14820,#14821,#14822,#14823,#14824,#14825,#14826,
#14827,#14828,#14829,#14830,#14831,#14832,#14833,#14834,#14835,#14836,#14837,
#14838,#14839,#14840,#14841,#14842,#14843,#14844,#14845,#14846,#14847,#14848,
#14849,#14850,#14851,#14852,#14853,#14854,#14855,#14856,#14857,#14858,#14859),
 .UNSPECIFIED.,.F.,.F.,(4,3,3,3,3,3,3,3,3,3,3,3,3,3,3,3,4),(6.48233978329073E-7,
0.088087481714971,0.125,0.211463563406532,0.25,0.336780768905252,0.375,
0.461780695889845,0.5,0.586763634796104,0.625,0.711758226647009,0.75,0.836456256382313,
0.875,0.963077038983795,0.9999992074512),.UNSPECIFIED.);
#161=B_SPLINE_CURVE_WITH_KNOTS('',3,(#14861,#14862,#14863,#14864,#14865,
#14866,#14867,#14868,#14869,#14870,#14871,#14872,#14873,#14874,#14875,#14876,
#14877,#14878,#14879,#14880,#14881,#14882,#14883,#14884,#14885,#14886,#14887,
#14888,#14889,#14890,#14891,#14892,#14893,#14894,#14895,#14896,#14897,#14898,
#14899,#14900,#14901,#14902,#14903,#14904,#14905,#14906,#14907,#14908,#14909),
 .UNSPECIFIED.,.F.,.F.,(4,3,3,3,3,3,3,3,3,3,3,3,3,3,3,3,4),(0.,0.0880873565129711,
0.125,0.211464312658339,0.25,0.33678412531568,0.375,0.461767822996489,0.5,
0.586767822996495,0.625,0.711784125315678,0.75,0.836464312658332,0.875,
0.963087356512997,1.),.UNSPECIFIED.);
#162=B_SPLINE_CURVE_WITH_KNOTS('',3,(#14911,#14912,#14913,#14914,#14915,
#14916,#14917,#14918,#14919,#14920,#14921,#14922,#14923,#14924,#14925,#14926,
#14927,#14928,#14929,#14930,#14931,#14932,#14933,#14934,#14935,#14936,#14937,
#14938,#14939,#14940,#14941,#14942,#14943,#14944,#14945,#14946,#14947,#14948,
#14949,#14950,#14951,#14952,#14953,#14954,#14955,#14956,#14957,#14958,#14959),
 .UNSPECIFIED.,.F.,.F.,(4,3,3,3,3,3,3,3,3,3,3,3,3,3,3,3,4),(0.,0.0881042076361416,
0.125,0.211481422598089,0.25,0.336801229758134,0.375,0.461784897184286,
0.5,0.586784897184306,0.625,0.71180122975812,0.75,0.836481422598088,0.875,
0.963104207636176,1.),.UNSPECIFIED.);
#163=B_SPLINE_CURVE_WITH_KNOTS('',3,(#14961,#14962,#14963,#14964,#14965,
#14966,#14967,#14968,#14969,#14970,#14971,#14972,#14973,#14974,#14975,#14976,
#14977,#14978,#14979,#14980,#14981,#14982,#14983,#14984,#14985,#14986,#14987,
#14988,#14989,#14990,#14991,#14992,#14993,#14994,#14995,#14996,#14997,#14998,
#14999,#15000,#15001,#15002,#15003,#15004,#15005,#15006,#15007,#15008,#15009),
 .UNSPECIFIED.,.F.,.F.,(4,3,3,3,3,3,3,3,3,3,3,3,3,3,3,3,4),(0.,0.0880892870445733,
0.125,0.21146627284444,0.25,0.336786084873347,0.375,0.461769779086792,0.5,
0.586769779086777,0.625,0.711786084873348,0.75,0.836466272844441,0.875,
0.963089287044564,1.),.UNSPECIFIED.);
#164=B_SPLINE_CURVE_WITH_KNOTS('',3,(#15011,#15012,#15013,#15014,#15015,
#15016,#15017,#15018,#15019,#15020,#15021,#15022,#15023,#15024,#15025,#15026,
#15027,#15028,#15029,#15030,#15031,#15032,#15033,#15034,#15035,#15036,#15037,
#15038,#15039,#15040,#15041,#15042,#15043,#15044,#15045,#15046,#15047,#15048,
#15049,#15050,#15051,#15052,#15053,#15054,#15055,#15056,#15057,#15058,#15059,
#15060,#15061,#15062,#15063,#15064,#15065,#15066,#15067,#15068,#15069,#15070,
#15071,#15072,#15073,#15074,#15075,#15076,#15077,#15078,#15079,#15080,#15081,
#15082,#15083),.UNSPECIFIED.,.F.,.F.,(4,3,3,3,3,3,3,3,3,3,3,3,3,3,3,3,3,
3,3,3,3,3,3,3,4),(1.04553770632841E-6,0.0875080165836233,0.125,0.211924214406689,
0.25,0.3125,0.375,0.40625,0.4375,0.46875,0.484375,0.4921875,0.5,0.5078125,
0.515625,0.53125,0.5625,0.59375,0.625,0.6875,0.75,0.8125,0.875,0.9375,0.999999334390892),
 .UNSPECIFIED.);
#165=B_SPLINE_CURVE_WITH_KNOTS('',3,(#15085,#15086,#15087,#15088,#15089,
#15090,#15091,#15092,#15093,#15094,#15095,#15096,#15097,#15098,#15099,#15100,
#15101,#15102,#15103,#15104,#15105,#15106,#15107,#15108,#15109,#15110,#15111,
#15112,#15113,#15114,#15115,#15116,#15117,#15118,#15119,#15120,#15121,#15122,
#15123,#15124,#15125,#15126,#15127,#15128,#15129,#15130,#15131,#15132,#15133),
 .UNSPECIFIED.,.F.,.F.,(4,3,3,3,3,3,3,3,3,3,3,3,3,3,3,3,4),(0.,0.0880950608203889,
0.125,0.211472135304815,0.25,0.33679194545211,0.375,0.461775629297404,0.5,
0.58677562929742,0.625,0.711791945452102,0.75,0.836472135304814,0.875,0.963095060820362,
1.),.UNSPECIFIED.);
#166=B_SPLINE_CURVE_WITH_KNOTS('',3,(#15135,#15136,#15137,#15138,#15139,
#15140,#15141,#15142,#15143,#15144,#15145,#15146,#15147,#15148,#15149,#15150,
#15151,#15152,#15153),.UNSPECIFIED.,.F.,.F.,(4,3,3,3,3,3,4),(0.,0.00857368461051335,
0.25,0.5,0.504408674649204,0.75,1.),.UNSPECIFIED.);
#167=B_SPLINE_CURVE_WITH_KNOTS('',3,(#15157,#15158,#15159,#15160,#15161,
#15162,#15163,#15164,#15165,#15166,#15167,#15168,#15169,#15170,#15171,#15172,
#15173,#15174,#15175,#15176,#15177,#15178,#15179,#15180,#15181,#15182,#15183,
#15184,#15185,#15186,#15187,#15188,#15189,#15190),.UNSPECIFIED.,.F.,.F.,
(4,3,3,3,3,3,3,3,3,3,3,4),(0.,0.158394062068541,0.25,0.282388204951903,
0.404806937739057,0.5,0.569551910301168,0.654806937739066,0.75,0.856807890509175,
0.908394062068542,1.),.UNSPECIFIED.);
#168=B_SPLINE_CURVE_WITH_KNOTS('',3,(#15192,#15193,#15194,#15195,#15196,
#15197,#15198,#15199,#15200,#15201,#15202,#15203,#15204,#15205,#15206,#15207,
#15208,#15209,#15210,#15211,#15212,#15213,#15214,#15215,#15216,#15217,#15218,
#15219,#15220,#15221,#15222,#15223,#15224,#15225,#15226,#15227,#15228,#15229,
#15230,#15231,#15232,#15233,#15234,#15235,#15236,#15237,#15238,#15239,#15240),
 .UNSPECIFIED.,.F.,.F.,(4,3,3,3,3,3,3,3,3,3,3,3,3,3,3,3,4),(3.26471858241762E-8,
0.0880825316349779,0.125,0.21145938337219,0.25,0.336779197608326,0.375,
0.461762904010005,0.5,0.586762904010012,0.625,0.711779197608325,0.75,0.836459383372186,
0.875,0.963082501803219,1.),.UNSPECIFIED.);
#169=B_SPLINE_CURVE_WITH_KNOTS('',3,(#15242,#15243,#15244,#15245,#15246,
#15247,#15248,#15249,#15250,#15251,#15252,#15253,#15254,#15255,#15256,#15257,
#15258,#15259,#15260,#15261,#15262,#15263,#15264,#15265,#15266,#15267,#15268,
#15269,#15270,#15271,#15272,#15273,#15274,#15275,#15276,#15277,#15278,#15279,
#15280,#15281,#15282,#15283,#15284,#15285,#15286,#15287,#15288,#15289,#15290),
 .UNSPECIFIED.,.F.,.F.,(4,3,3,3,3,3,3,3,3,3,3,3,3,3,3,3,4),(0.,0.0881017307290489,
0.125,0.211478907652486,0.25,0.336798715622224,0.375,0.461782387493885,
0.5,0.586782387493868,0.625,0.711798715622233,0.75,0.836478907652487,0.875,
0.963101730729054,1.),.UNSPECIFIED.);
#170=B_SPLINE_CURVE_WITH_KNOTS('',3,(#15291,#15292,#15293,#15294,#15295,
#15296,#15297,#15298,#15299,#15300,#15301,#15302,#15303,#15304,#15305,#15306,
#15307,#15308,#15309,#15310,#15311,#15312,#15313,#15314,#15315,#15316,#15317,
#15318,#15319,#15320,#15321,#15322,#15323,#15324,#15325,#15326,#15327,#15328,
#15329,#15330,#15331,#15332,#15333,#15334,#15335,#15336,#15337,#15338,#15339),
 .UNSPECIFIED.,.F.,.F.,(4,3,3,3,3,3,3,3,3,3,3,3,3,3,3,3,4),(0.,0.0880930729141991,
0.125,0.211470116865539,0.25,0.336789927661028,0.375,0.461773615075734,
0.5,0.586773615075741,0.625,0.711789927661028,0.75,0.836470116865545,0.875,
0.963093072914204,1.),.UNSPECIFIED.);
#171=B_SPLINE_CURVE_WITH_KNOTS('',3,(#15343,#15344,#15345,#15346,#15347,
#15348,#15349,#15350,#15351,#15352,#15353,#15354,#15355,#15356,#15357,#15358,
#15359,#15360,#15361,#15362,#15363,#15364,#15365,#15366,#15367,#15368,#15369,
#15370,#15371,#15372,#15373,#15374,#15375,#15376,#15377,#15378,#15379,#15380,
#15381,#15382,#15383,#15384,#15385,#15386,#15387,#15388,#15389,#15390,#15391,
#15392,#15393,#15394,#15395,#15396,#15397,#15398,#15399,#15400,#15401,#15402,
#15403,#15404,#15405,#15406,#15407,#15408,#15409,#15410,#15411,#15412,#15413,
#15414,#15415,#15416,#15417,#15418),.UNSPECIFIED.,.F.,.F.,(4,3,3,3,3,3,
3,3,3,3,3,3,3,3,3,3,3,3,3,3,3,3,3,3,3,4),(7.93458957479051E-7,0.0919827770270099,
0.125,0.21636947259665,0.25,0.3125,0.375,0.40625,0.4375,0.46875,0.484375,
0.4921875,0.5,0.5078125,0.515625,0.53125,0.5625,0.59375,0.625,0.6875,0.75,
0.8125,0.875,0.9375,0.992573279862854,0.999999611514097),.UNSPECIFIED.);
#172=B_SPLINE_CURVE_WITH_KNOTS('',3,(#15420,#15421,#15422,#15423,#15424,
#15425,#15426,#15427,#15428,#15429,#15430,#15431,#15432,#15433,#15434,#15435,
#15436,#15437,#15438,#15439,#15440,#15441,#15442,#15443,#15444,#15445,#15446,
#15447,#15448,#15449,#15450,#15451,#15452,#15453,#15454,#15455,#15456,#15457,
#15458,#15459,#15460,#15461,#15462,#15463,#15464,#15465,#15466,#15467,#15468),
 .UNSPECIFIED.,.F.,.F.,(4,3,3,3,3,3,3,3,3,3,3,3,3,3,3,3,4),(0.,0.0926028564089548,
0.125,0.215896935943174,0.25,0.341233104859871,0.375,0.466215951447718,
0.5,0.591215951447998,0.625,0.716233104860131,0.75,0.840896935943215,0.875,
0.967602856408858,1.),.UNSPECIFIED.);
#173=B_SPLINE_CURVE_WITH_KNOTS('',3,(#15470,#15471,#15472,#15473,#15474,
#15475,#15476,#15477,#15478,#15479,#15480,#15481,#15482,#15483,#15484,#15485,
#15486,#15487,#15488,#15489,#15490,#15491,#15492,#15493,#15494,#15495,#15496,
#15497,#15498,#15499,#15500,#15501,#15502,#15503,#15504,#15505,#15506,#15507,
#15508,#15509,#15510,#15511,#15512,#15513,#15514,#15515,#15516,#15517,#15518),
 .UNSPECIFIED.,.F.,.F.,(4,3,3,3,3,3,3,3,3,3,3,3,3,3,3,3,4),(0.,0.0926016482516165,
0.125,0.215895709229479,0.25,0.341231878540584,0.375,0.466214727297818,
0.5,0.591214727297569,0.625,0.716231878540515,0.75,0.840895709229348,0.875,
0.967601648251421,1.),.UNSPECIFIED.);
#174=B_SPLINE_CURVE_WITH_KNOTS('',3,(#15520,#15521,#15522,#15523,#15524,
#15525,#15526,#15527,#15528,#15529,#15530,#15531,#15532,#15533,#15534,#15535,
#15536,#15537,#15538,#15539,#15540,#15541,#15542,#15543,#15544,#15545,#15546,
#15547,#15548,#15549,#15550,#15551,#15552,#15553),.UNSPECIFIED.,.F.,.F.,
(4,2,2,2,2,2,2,2,2,2,2,2,2,2,2,2,4),(8.60008680714194E-7,0.0925922496141415,
0.125,0.215885936189025,0.25,0.341220868711526,0.375,0.466201529424218,
0.5,0.59123334097936,0.625,0.71618155918904,0.75,0.84088010118624,0.875,
0.967583301320753,0.99999903411916),.UNSPECIFIED.);
#175=B_SPLINE_CURVE_WITH_KNOTS('',3,(#15555,#15556,#15557,#15558,#15559,
#15560,#15561,#15562,#15563,#15564,#15565,#15566,#15567,#15568,#15569,#15570,
#15571,#15572,#15573,#15574,#15575,#15576,#15577,#15578,#15579,#15580,#15581,
#15582,#15583,#15584,#15585,#15586,#15587,#15588,#15589,#15590,#15591,#15592,
#15593,#15594,#15595,#15596,#15597,#15598,#15599,#15600,#15601,#15602,#15603),
 .UNSPECIFIED.,.F.,.F.,(4,3,3,3,3,3,3,3,3,3,3,3,3,3,3,3,4),(0.,0.0925946446316686,
0.125,0.215888598034351,0.25,0.341224769627743,0.375,0.466207630961137,
0.5,0.591207630961336,0.625,0.716224769627659,0.75,0.840888598034289,0.875,
0.967594644631377,1.),.UNSPECIFIED.);
#176=B_SPLINE_CURVE_WITH_KNOTS('',3,(#15605,#15606,#15607,#15608,#15609,
#15610,#15611,#15612,#15613,#15614,#15615,#15616,#15617,#15618,#15619,#15620,
#15621,#15622,#15623,#15624,#15625,#15626,#15627,#15628,#15629,#15630,#15631,
#15632,#15633,#15634,#15635,#15636,#15637,#15638,#15639,#15640,#15641,#15642,
#15643,#15644,#15645,#15646,#15647,#15648,#15649,#15650,#15651,#15652,#15653),
 .UNSPECIFIED.,.F.,.F.,(4,3,3,3,3,3,3,3,3,3,3,3,3,3,3,3,4),(0.,0.0926110770714553,
0.125,0.215905282857406,0.25,0.341241449089134,0.375,0.466224280920412,
0.5,0.591224280920756,0.625,0.716241449088887,0.75,0.840905282857528,0.875,
0.967611077071527,1.),.UNSPECIFIED.);
#177=B_SPLINE_CURVE_WITH_KNOTS('',3,(#15655,#15656,#15657,#15658,#15659,
#15660,#15661,#15662,#15663,#15664,#15665,#15666,#15667,#15668,#15669,#15670,
#15671,#15672,#15673,#15674,#15675,#15676,#15677,#15678,#15679,#15680,#15681,
#15682,#15683,#15684,#15685,#15686,#15687,#15688,#15689,#15690,#15691,#15692,
#15693,#15694,#15695,#15696,#15697,#15698,#15699,#15700,#15701,#15702,#15703),
 .UNSPECIFIED.,.F.,.F.,(4,3,3,3,3,3,3,3,3,3,3,3,3,3,3,3,4),(0.,0.0925939685908668,
0.125,0.215887911608834,0.25,0.341224083422187,0.375,0.466206945970056,
0.5,0.591206945970017,0.625,0.716224083422156,0.75,0.840887911608889,0.875,
0.967593968591154,1.),.UNSPECIFIED.);
#178=B_SPLINE_CURVE_WITH_KNOTS('',3,(#15705,#15706,#15707,#15708,#15709,
#15710,#15711,#15712,#15713,#15714,#15715,#15716,#15717,#15718,#15719,#15720,
#15721,#15722,#15723,#15724,#15725,#15726,#15727,#15728,#15729,#15730,#15731,
#15732,#15733,#15734,#15735,#15736,#15737,#15738,#15739,#15740,#15741,#15742,
#15743,#15744,#15745,#15746,#15747,#15748,#15749,#15750,#15751,#15752,#15753,
#15754,#15755,#15756,#15757,#15758,#15759,#15760,#15761,#15762,#15763,#15764,
#15765,#15766,#15767,#15768,#15769,#15770,#15771,#15772,#15773,#15774,#15775,
#15776,#15777,#15778,#15779,#15780),.UNSPECIFIED.,.F.,.F.,(4,3,3,3,3,3,
3,3,3,3,3,3,3,3,3,3,3,3,3,3,3,3,3,3,3,4),(8.85984697358488E-7,0.0919833162888678,
0.125,0.216369876637167,0.25,0.3125,0.375,0.40625,0.4375,0.46875,0.484375,
0.4921875,0.5,0.5078125,0.515625,0.53125,0.5625,0.59375,0.625,0.6875,0.75,
0.8125,0.875,0.9375,0.995501429491965,0.999999512663293),.UNSPECIFIED.);
#179=B_SPLINE_CURVE_WITH_KNOTS('',3,(#15782,#15783,#15784,#15785,#15786,
#15787,#15788,#15789,#15790,#15791,#15792,#15793,#15794,#15795,#15796,#15797,
#15798,#15799,#15800,#15801,#15802,#15803,#15804,#15805,#15806,#15807,#15808,
#15809,#15810,#15811,#15812,#15813,#15814,#15815,#15816,#15817,#15818,#15819,
#15820,#15821,#15822,#15823,#15824,#15825,#15826,#15827,#15828,#15829,#15830),
 .UNSPECIFIED.,.F.,.F.,(4,3,3,3,3,3,3,3,3,3,3,3,3,3,3,3,4),(0.,0.0926016640197792,
0.125,0.215895725240053,0.25,0.341231894546074,0.375,0.466214743274479,
0.5,0.591214743274513,0.625,0.71623189454608,0.75,0.840895725240135,0.875,
0.96760166401992,0.99999999999941),.UNSPECIFIED.);
#180=B_SPLINE_CURVE_WITH_KNOTS('',3,(#15834,#15835,#15836,#15837,#15838,
#15839,#15840),.UNSPECIFIED.,.F.,.F.,(4,3,4),(3.02475966928685E-5,0.761300445681502,
0.999991310305325),.UNSPECIFIED.);
#181=B_SPLINE_CURVE_WITH_KNOTS('',3,(#15842,#15843,#15844,#15845,#15846,
#15847,#15848,#15849,#15850,#15851,#15852,#15853,#15854,#15855,#15856,#15857,
#15858,#15859,#15860,#15861,#15862,#15863,#15864,#15865,#15866,#15867,#15868,
#15869,#15870,#15871,#15872,#15873,#15874,#15875,#15876,#15877,#15878,#15879,
#15880,#15881,#15882,#15883,#15884,#15885,#15886,#15887,#15888,#15889,#15890),
 .UNSPECIFIED.,.F.,.F.,(4,3,3,3,3,3,3,3,3,3,3,3,3,3,3,3,4),(0.,0.0926097133311401,
0.125,0.215903898174036,0.25,0.341240064851683,0.375,0.466222899130803,
0.5,0.591222899130775,0.625,0.716240064851504,0.75,0.840903898174011,0.875,
0.967609713331501,1.),.UNSPECIFIED.);
#182=B_SPLINE_CURVE_WITH_KNOTS('',3,(#15892,#15893,#15894,#15895,#15896,
#15897,#15898,#15899,#15900,#15901,#15902,#15903,#15904,#15905,#15906,#15907,
#15908,#15909,#15910,#15911,#15912,#15913,#15914,#15915,#15916,#15917,#15918,
#15919,#15920,#15921,#15922,#15923,#15924,#15925,#15926,#15927,#15928,#15929,
#15930,#15931,#15932,#15933,#15934,#15935,#15936,#15937,#15938,#15939,#15940),
 .UNSPECIFIED.,.F.,.F.,(4,3,3,3,3,3,3,3,3,3,3,3,3,3,3,3,4),(0.,0.0925981673177476,
0.125,0.215892174830268,0.25,0.3412283452762,0.375,0.466211200283384,0.5,
0.591211200283569,0.625,0.716228345276186,0.75,0.840892174830337,0.875,
0.967598167317428,1.),.UNSPECIFIED.);
#183=B_SPLINE_CURVE_WITH_KNOTS('',3,(#15942,#15943,#15944,#15945,#15946,
#15947,#15948,#15949,#15950,#15951,#15952,#15953,#15954,#15955,#15956,#15957,
#15958,#15959,#15960,#15961,#15962,#15963,#15964,#15965,#15966,#15967,#15968,
#15969,#15970,#15971,#15972,#15973,#15974,#15975,#15976,#15977,#15978,#15979,
#15980,#15981,#15982,#15983,#15984,#15985,#15986,#15987,#15988,#15989,#15990,
#15991,#15992,#15993),.UNSPECIFIED.,.F.,.F.,(4,3,3,3,3,3,3,3,3,3,3,3,3,
3,3,3,3,4),(1.25053720846655E-6,0.0929545115982379,0.125,0.215420114878467,
0.25,0.339746875247112,0.375,0.4375,0.496741821459526,0.5,0.5625,0.625,
0.722152298803526,0.75,0.8373366708814,0.875,0.959989006508124,0.999998883500357),
 .UNSPECIFIED.);
#184=B_SPLINE_CURVE_WITH_KNOTS('',3,(#15995,#15996,#15997,#15998,#15999,
#16000,#16001,#16002,#16003,#16004,#16005,#16006,#16007,#16008,#16009,#16010,
#16011,#16012,#16013,#16014,#16015,#16016,#16017,#16018,#16019,#16020,#16021,
#16022,#16023,#16024,#16025,#16026,#16027,#16028,#16029,#16030,#16031,#16032,
#16033,#16034,#16035,#16036,#16037,#16038,#16039,#16040,#16041,#16042,#16043),
 .UNSPECIFIED.,.F.,.F.,(4,3,3,3,3,3,3,3,3,3,3,3,3,3,3,3,4),(0.,0.09259973745462,
0.125,0.215893769083908,0.25,0.341229939018056,0.375,0.466212791205734,
0.5,0.591212791205995,0.625,0.716229939018014,0.75,0.840893769083763,0.875,
0.967599737454784,1.),.UNSPECIFIED.);
#185=B_SPLINE_CURVE_WITH_KNOTS('',3,(#16045,#16046,#16047,#16048,#16049,
#16050,#16051,#16052,#16053,#16054,#16055,#16056,#16057,#16058,#16059,#16060,
#16061,#16062,#16063,#16064,#16065,#16066,#16067,#16068,#16069,#16070,#16071,
#16072,#16073,#16074,#16075,#16076,#16077,#16078,#16079,#16080,#16081,#16082,
#16083,#16084,#16085,#16086,#16087,#16088,#16089,#16090,#16091,#16092,#16093),
 .UNSPECIFIED.,.F.,.F.,(4,3,3,3,3,3,3,3,3,3,3,3,3,3,3,3,4),(0.,0.0926077535236005,
0.125,0.215901908268581,0.25,0.341238075586479,0.375,0.4662209133831,0.5,
0.591220913383166,0.625,0.716238075586483,0.75,0.840901908268568,0.875,
0.967607753523283,1.),.UNSPECIFIED.);
#186=B_SPLINE_CURVE_WITH_KNOTS('',3,(#16095,#16096,#16097,#16098,#16099,
#16100,#16101,#16102,#16103,#16104,#16105,#16106,#16107,#16108,#16109,#16110,
#16111,#16112,#16113,#16114,#16115,#16116,#16117,#16118,#16119,#16120,#16121,
#16122,#16123,#16124,#16125,#16126,#16127,#16128,#16129,#16130,#16131,#16132,
#16133,#16134,#16135,#16136,#16137,#16138,#16139,#16140,#16141,#16142,#16143),
 .UNSPECIFIED.,.F.,.F.,(4,3,3,3,3,3,3,3,3,3,3,3,3,3,3,3,4),(0.,0.0925881405225714,
0.125,0.21588199401248,0.25,0.341218167721451,0.375,0.466201040738566,0.5,
0.591201040738367,0.625,0.716218167721304,0.75,0.840881994012549,0.875,
0.967588139527948,0.999999861566054),.UNSPECIFIED.);
#187=B_SPLINE_CURVE_WITH_KNOTS('',3,(#16145,#16146,#16147,#16148,#16149,
#16150,#16151,#16152,#16153,#16154,#16155,#16156,#16157,#16158,#16159,#16160,
#16161,#16162,#16163,#16164,#16165,#16166,#16167,#16168,#16169,#16170,#16171,
#16172,#16173,#16174,#16175,#16176,#16177,#16178,#16179,#16180,#16181,#16182,
#16183,#16184,#16185,#16186,#16187,#16188,#16189,#16190,#16191,#16192,#16193),
 .UNSPECIFIED.,.F.,.F.,(4,3,3,3,3,3,3,3,3,3,3,3,3,3,3,3,4),(0.,0.0925890173961925,
0.125,0.215882884356336,0.25,0.34121905778002,0.375,0.46620192922203,0.5,
0.591201929222098,0.625,0.716219057780218,0.75,0.840882884356031,0.875,
0.967589017395721,1.),.UNSPECIFIED.);
#188=B_SPLINE_CURVE_WITH_KNOTS('',3,(#16195,#16196,#16197,#16198,#16199,
#16200,#16201,#16202,#16203,#16204,#16205,#16206,#16207,#16208,#16209,#16210,
#16211,#16212,#16213,#16214,#16215,#16216,#16217,#16218,#16219,#16220,#16221,
#16222,#16223,#16224,#16225,#16226,#16227,#16228,#16229,#16230,#16231,#16232,
#16233,#16234,#16235,#16236,#16237,#16238,#16239,#16240,#16241,#16242,#16243),
 .UNSPECIFIED.,.F.,.F.,(4,3,3,3,3,3,3,3,3,3,3,3,3,3,3,3,4),(0.,0.0926091135500264,
0.125,0.215903289181841,0.25,0.341239456055151,0.375,0.466222291411168,
0.5,0.59122229141116,0.625,0.716239456055371,0.75,0.840903289181801,0.875,
0.967609113549421,1.),.UNSPECIFIED.);
#189=B_SPLINE_CURVE_WITH_KNOTS('',3,(#16245,#16246,#16247,#16248,#16249,
#16250,#16251,#16252,#16253,#16254,#16255,#16256,#16257,#16258,#16259,#16260,
#16261,#16262,#16263,#16264,#16265,#16266,#16267,#16268,#16269,#16270,#16271,
#16272,#16273,#16274,#16275,#16276,#16277,#16278,#16279,#16280,#16281,#16282,
#16283,#16284,#16285,#16286,#16287,#16288,#16289,#16290,#16291,#16292,#16293),
 .UNSPECIFIED.,.F.,.F.,(4,3,3,3,3,3,3,3,3,3,3,3,3,3,3,3,4),(0.,0.0925986851494203,
0.125,0.215892700615775,0.25,0.341228870892842,0.375,0.466211724970258,
0.5,0.59121172497034,0.625,0.716228870892888,0.75,0.840892700615926,0.875,
0.967598685149769,1.),.UNSPECIFIED.);
#190=B_SPLINE_CURVE_WITH_KNOTS('',3,(#16295,#16296,#16297,#16298,#16299,
#16300,#16301,#16302,#16303,#16304,#16305,#16306,#16307,#16308,#16309,#16310,
#16311,#16312,#16313,#16314,#16315,#16316,#16317,#16318,#16319,#16320,#16321,
#16322,#16323,#16324,#16325,#16326,#16327,#16328,#16329,#16330,#16331,#16332,
#16333,#16334,#16335,#16336,#16337,#16338,#16339,#16340),.UNSPECIFIED.,
 .F.,.F.,(4,3,3,3,3,3,3,3,3,3,3,3,3,3,3,4),(1.25824916392832E-6,0.0923454433051621,
0.125,0.216129877093308,0.25,0.342613529803912,0.375,0.457998148773538,
0.5,0.625,0.714780278674796,0.75,0.839601858305807,0.875,0.964995303736524,
0.999998796399913),.UNSPECIFIED.);
#191=B_SPLINE_CURVE_WITH_KNOTS('',3,(#16342,#16343,#16344,#16345,#16346,
#16347,#16348,#16349,#16350,#16351,#16352,#16353,#16354,#16355,#16356,#16357,
#16358,#16359,#16360,#16361,#16362,#16363,#16364,#16365,#16366,#16367,#16368,
#16369,#16370,#16371,#16372,#16373,#16374,#16375,#16376,#16377,#16378,#16379,
#16380,#16381,#16382,#16383,#16384,#16385,#16386,#16387,#16388,#16389,#16390),
 .UNSPECIFIED.,.F.,.F.,(4,3,3,3,3,3,3,3,3,3,3,3,3,3,3,3,4),(0.,0.0925992895932416,
0.125,0.215893314343291,0.25,0.341229484423304,0.375,0.46621233741587,0.5,
0.591212337415676,0.625,0.716229484423541,0.75,0.840893314343279,0.875,
0.967599289593344,1.),.UNSPECIFIED.);
#192=B_SPLINE_CURVE_WITH_KNOTS('',3,(#16392,#16393,#16394,#16395,#16396,
#16397,#16398,#16399,#16400,#16401,#16402,#16403,#16404,#16405,#16406,#16407,
#16408,#16409,#16410,#16411,#16412,#16413,#16414,#16415,#16416,#16417,#16418,
#16419,#16420,#16421,#16422,#16423,#16424,#16425,#16426,#16427,#16428,#16429,
#16430,#16431,#16432,#16433,#16434,#16435,#16436,#16437,#16438,#16439,#16440),
 .UNSPECIFIED.,.F.,.F.,(4,3,3,3,3,3,3,3,3,3,3,3,3,3,3,3,4),(0.,0.0926083986537193,
0.125,0.215902563306285,0.25,0.341238730413271,0.375,0.466221567052477,
0.5,0.59122156705239,0.625,0.716238730413398,0.75,0.840902563306212,0.875,
0.967608398653425,1.),.UNSPECIFIED.);
#193=B_SPLINE_CURVE_WITH_KNOTS('',3,(#16442,#16443,#16444,#16445,#16446,
#16447,#16448,#16449,#16450,#16451,#16452,#16453,#16454,#16455,#16456,#16457,
#16458,#16459,#16460,#16461,#16462,#16463,#16464,#16465,#16466,#16467,#16468,
#16469,#16470,#16471,#16472,#16473,#16474,#16475,#16476,#16477,#16478,#16479,
#16480,#16481,#16482,#16483,#16484,#16485,#16486,#16487,#16488,#16489,#16490),
 .UNSPECIFIED.,.F.,.F.,(4,3,3,3,3,3,3,3,3,3,3,3,3,3,3,3,4),(0.,0.0925881676381304,
0.125,0.215882021544404,0.25,0.341218195244346,0.375,0.466201068212794,
0.5,0.591201068212782,0.625,0.716218195244376,0.75,0.840882021544444,0.875,
0.96758816740381,0.999999967401505),.UNSPECIFIED.);
#194=B_SPLINE_CURVE_WITH_KNOTS('',3,(#16492,#16493,#16494,#16495,#16496,
#16497,#16498,#16499,#16500,#16501,#16502,#16503,#16504,#16505,#16506,#16507,
#16508,#16509,#16510,#16511,#16512,#16513,#16514,#16515,#16516,#16517,#16518,
#16519,#16520,#16521,#16522,#16523,#16524,#16525,#16526,#16527,#16528,#16529,
#16530,#16531,#16532,#16533,#16534,#16535,#16536,#16537,#16538,#16539,#16540),
 .UNSPECIFIED.,.F.,.F.,(4,3,3,3,3,3,3,3,3,3,3,3,3,3,3,3,4),(0.,0.106287359337513,
0.125,0.229771416343439,0.25,0.355096911466,0.375,0.480061767793933,0.5,
0.605061767794126,0.625,0.730096911465622,0.75,0.854771416343529,0.875,
0.981287359338472,0.999999999999949),.UNSPECIFIED.);
#195=B_SPLINE_CURVE_WITH_KNOTS('',3,(#16544,#16545,#16546,#16547,#16548,
#16549,#16550,#16551,#16552,#16553,#16554,#16555,#16556,#16557,#16558,#16559,
#16560,#16561,#16562,#16563,#16564,#16565,#16566,#16567,#16568,#16569,#16570,
#16571,#16572,#16573,#16574,#16575,#16576,#16577,#16578,#16579,#16580,#16581,
#16582,#16583,#16584,#16585,#16586,#16587,#16588,#16589,#16590,#16591,#16592),
 .UNSPECIFIED.,.F.,.F.,(4,3,3,3,3,3,3,3,3,3,3,3,3,3,3,3,4),(4.5000019854714E-7,
0.0926018329307898,0.125,0.215895443114202,0.25,0.341231612510821,0.375,
0.466214461738461,0.5,0.591214461738094,0.625,0.716231612510757,0.75,0.840895443114331,
0.875,0.967601386161383,1.),.UNSPECIFIED.);
#196=B_SPLINE_CURVE_WITH_KNOTS('',3,(#16594,#16595,#16596,#16597,#16598,
#16599,#16600,#16601,#16602,#16603,#16604,#16605,#16606,#16607,#16608,#16609,
#16610,#16611,#16612,#16613,#16614,#16615,#16616,#16617,#16618,#16619,#16620,
#16621,#16622,#16623,#16624,#16625,#16626,#16627),.UNSPECIFIED.,.F.,.F.,
(4,2,2,2,2,2,2,2,2,2,2,2,2,2,2,2,4),(9.46277652146847E-7,0.0925916484161767,
0.125,0.215885706168785,0.25,0.34122139386794,0.375,0.466192349791288,0.5,
0.591249283254599,0.625,0.716174174210448,0.75,0.840880794969292,0.875,
0.967583711036726,0.99999896009837),.UNSPECIFIED.);
#197=B_SPLINE_CURVE_WITH_KNOTS('',3,(#16629,#16630,#16631,#16632,#16633,
#16634,#16635,#16636,#16637,#16638,#16639,#16640,#16641,#16642,#16643,#16644,
#16645,#16646,#16647,#16648,#16649,#16650,#16651,#16652,#16653,#16654,#16655,
#16656,#16657,#16658,#16659,#16660,#16661,#16662,#16663,#16664,#16665,#16666,
#16667,#16668,#16669,#16670,#16671,#16672,#16673,#16674,#16675,#16676,#16677),
 .UNSPECIFIED.,.F.,.F.,(4,3,3,3,3,3,3,3,3,3,3,3,3,3,3,3,4),(0.,0.0925953041831434,
0.125,0.215889267717039,0.25,0.341225439095757,0.375,0.466208299244986,
0.5,0.591208299244716,0.625,0.716225439095638,0.75,0.840889267717158,0.875,
0.96759530418352,1.),.UNSPECIFIED.);
#198=B_SPLINE_CURVE_WITH_KNOTS('',3,(#16679,#16680,#16681,#16682,#16683,
#16684,#16685,#16686,#16687,#16688,#16689,#16690,#16691,#16692,#16693,#16694,
#16695,#16696,#16697,#16698,#16699,#16700,#16701,#16702,#16703,#16704,#16705,
#16706,#16707,#16708,#16709,#16710,#16711,#16712,#16713,#16714,#16715,#16716,
#16717,#16718,#16719,#16720,#16721,#16722,#16723,#16724,#16725,#16726,#16727),
 .UNSPECIFIED.,.F.,.F.,(4,3,3,3,3,3,3,3,3,3,3,3,3,3,3,3,4),(0.,0.0926110022616626,
0.125,0.215905206898781,0.25,0.341241373155053,0.375,0.466224205121077,
0.5,0.591224205120857,0.625,0.716241373154821,0.75,0.840905206898693,0.875,
0.967611002261608,1.),.UNSPECIFIED.);
#199=B_SPLINE_CURVE_WITH_KNOTS('',3,(#16728,#16729,#16730,#16731,#16732,
#16733,#16734,#16735,#16736,#16737,#16738,#16739,#16740,#16741,#16742,#16743,
#16744,#16745,#16746,#16747,#16748,#16749,#16750,#16751,#16752,#16753,#16754,
#16755,#16756,#16757,#16758,#16759,#16760,#16761,#16762,#16763,#16764,#16765,
#16766,#16767,#16768,#16769,#16770,#16771,#16772,#16773,#16774,#16775,#16776),
 .UNSPECIFIED.,.F.,.F.,(4,3,3,3,3,3,3,3,3,3,3,3,3,3,3,3,4),(0.,0.0925932731175236,
0.125,0.215887205452251,0.25,0.34122337749192,0.375,0.466206241288816,0.5,
0.591206241289337,0.625,0.716223377492011,0.75,0.84088720545214,0.875,0.967593273117083,
1.),.UNSPECIFIED.);
#200=B_SPLINE_CURVE_WITH_KNOTS('',3,(#16822,#16823,#16824,#16825,#16826,
#16827,#16828,#16829,#16830,#16831,#16832,#16833,#16834,#16835,#16836,#16837,
#16838,#16839,#16840,#16841,#16842,#16843,#16844,#16845,#16846,#16847,#16848,
#16849,#16850,#16851,#16852,#16853,#16854,#16855,#16856,#16857,#16858,#16859,
#16860,#16861,#16862,#16863,#16864,#16865,#16866,#16867,#16868,#16869,#16870,
#16871,#16872,#16873,#16874,#16875,#16876),.UNSPECIFIED.,.F.,.F.,(4,3,3,
3,3,3,3,3,3,3,3,3,3,3,3,3,3,3,4),(-0.569248610399452,-0.543571759198363,
-0.510395599541255,-0.504799388975929,-0.45563601739013,-0.442602338909788,
-0.358452201979706,-0.343831278006888,-0.337469726455479,-0.308533410217098,
-0.30096067569989,-0.233918536086011,-0.22808143434137,-0.139754810098741,
-0.122954682021969,-0.117884022561589,-0.113367531001717,-0.00535378548456125,
-6.56921400347513E-5),.UNSPECIFIED.);
#201=B_SPLINE_CURVE_WITH_KNOTS('',3,(#16877,#16878,#16879,#16880,#16881,
#16882,#16883,#16884,#16885,#16886,#16887,#16888,#16889,#16890,#16891,#16892,
#16893,#16894,#16895,#16896,#16897,#16898,#16899,#16900,#16901,#16902,#16903,
#16904,#16905,#16906,#16907,#16908,#16909,#16910,#16911,#16912,#16913,#16914,
#16915,#16916,#16917,#16918,#16919,#16920,#16921,#16922,#16923,#16924,#16925,
#16926,#16927,#16928,#16929,#16930,#16931),.UNSPECIFIED.,.F.,.F.,(4,3,3,
3,3,3,3,3,3,3,3,3,3,3,3,3,3,3,4),(-0.566847306048063,-0.536663225899598,
-0.497463681658886,-0.490486608162161,-0.423989019112076,-0.41889779448436,
-0.317015916859763,-0.311568571461078,-0.307442392923327,-0.279475887950007,
-0.27234718303655,-0.21391709050398,-0.20477719839138,-0.200645503382732,
-0.117724865987957,-0.103391697089455,-0.0995431702903938,-0.00440105423172584,
0.),.UNSPECIFIED.);
#202=B_SPLINE_CURVE_WITH_KNOTS('',3,(#17304,#17305,#17306,#17307,#17308,
#17309,#17310,#17311,#17312,#17313,#17314,#17315,#17316,#17317,#17318,#17319,
#17320,#17321,#17322,#17323,#17324,#17325,#17326,#17327,#17328,#17329,#17330,
#17331,#17332,#17333,#17334,#17335,#17336,#17337,#17338,#17339,#17340,#17341,
#17342,#17343,#17344,#17345,#17346,#17347,#17348,#17349,#17350,#17351,#17352,
#17353,#17354,#17355,#17356,#17357,#17358,#17359,#17360,#17361,#17362,#17363,
#17364,#17365,#17366,#17367,#17368,#17369,#17370),.UNSPECIFIED.,.F.,.F.,
(4,3,3,3,3,3,3,3,3,3,3,3,3,3,3,3,3,3,3,3,3,3,4),(0.,0.0902263235284944,
0.0965695032982788,0.102693117565567,0.185183726670681,0.195784092223982,
0.201956945222684,0.206397101465053,0.235002111145181,0.263505425073497,
0.267460741436352,0.295373658448176,0.306667851934945,0.311356021489761,
0.402390498589277,0.414121393711446,0.422114271443368,0.426853739956178,
0.483056044923388,0.493852365850745,0.499811702366216,0.561514407519245,
0.566789965462338),.UNSPECIFIED.);
#203=B_SPLINE_CURVE_WITH_KNOTS('',3,(#17743,#17744,#17745,#17746,#17747,
#17748,#17749,#17750,#17751,#17752,#17753,#17754,#17755,#17756,#17757,#17758,
#17759,#17760,#17761,#17762,#17763,#17764,#17765,#17766,#17767,#17768,#17769,
#17770,#17771,#17772,#17773,#17774,#17775,#17776,#17777,#17778,#17779,#17780,
#17781,#17782,#17783,#17784,#17785,#17786,#17787,#17788,#17789,#17790,#17791,
#17792,#17793,#17794,#17795,#17796,#17797,#17798,#17799,#17800,#17801,#17802,
#17803,#17804,#17805,#17806),.UNSPECIFIED.,.F.,.F.,(4,3,3,3,3,3,3,3,3,3,
3,3,3,3,3,3,3,3,3,3,3,4),(0.,0.0297263173547245,0.115411427535913,0.120694019406524,
0.150458483605126,0.209056395204914,0.221568856508229,0.228760022478968,
0.23414409783388,0.290594481715472,0.296053478345246,0.325007652648377,
0.335794721522812,0.340099498092156,0.344569097461082,0.428539652510242,
0.441342004070912,0.446282536720056,0.507885976399662,0.513324701408156,
0.56483218923889,0.569248610399433),.UNSPECIFIED.);
#204=B_SPLINE_CURVE_WITH_KNOTS('',3,(#18145,#18146,#18147,#18148),
 .UNSPECIFIED.,.F.,.F.,(4,4),(0.971412745929808,0.971526261856752),
 .UNSPECIFIED.);
#205=B_SPLINE_CURVE_WITH_KNOTS('',3,(#18150,#18151,#18152,#18153,#18154,
#18155,#18156,#18157,#18158,#18159),.UNSPECIFIED.,.F.,.F.,(4,3,3,4),(0.,
0.167901694834844,0.56724113492481,0.999999992512719),.UNSPECIFIED.);
#206=B_SPLINE_CURVE_WITH_KNOTS('',3,(#18161,#18162,#18163,#18164,#18165,
#18166),.UNSPECIFIED.,.F.,.F.,(4,2,4),(0.315127929368065,0.328175365228812,
0.354466558811423),.UNSPECIFIED.);
#207=B_SPLINE_CURVE_WITH_KNOTS('',3,(#18168,#18169,#18170,#18171,#18172,
#18173,#18174,#18175,#18176,#18177,#18178,#18179,#18180,#18181,#18182,#18183,
#18184,#18185,#18186,#18187,#18188,#18189,#18190,#18191,#18192,#18193,#18194,
#18195,#18196,#18197,#18198,#18199,#18200,#18201,#18202,#18203,#18204,#18205,
#18206,#18207,#18208,#18209,#18210,#18211,#18212,#18213,#18214,#18215),
 .UNSPECIFIED.,.F.,.F.,(4,2,2,2,2,2,2,2,2,2,2,2,2,2,2,2,2,2,2,2,2,2,2,4),
(0.000119713185355978,0.00575344874658494,0.00971112169393152,0.0122781598323848,
0.0146592854190729,0.0174902469786257,0.0227397139191457,0.0430245441916241,
0.0660773827934058,0.0761631161494674,0.0842516350753493,0.0890477968215787,
0.0934275126674497,0.0991547350761513,0.111968591580187,0.132666811210395,
0.158224662764418,0.163318033350428,0.166132967630979,0.16860703948596,
0.172184160315179,0.182361036453311,0.201361583255606,0.223791868919182),
 .UNSPECIFIED.);
#208=B_SPLINE_CURVE_WITH_KNOTS('',3,(#18216,#18217,#18218,#18219),
 .UNSPECIFIED.,.F.,.F.,(4,4),(-9.40886979550022E-5,-9.99998847734106E-7),
 .UNSPECIFIED.);
#209=B_SPLINE_CURVE_WITH_KNOTS('',3,(#18225,#18226,#18227,#18228),
 .UNSPECIFIED.,.F.,.F.,(4,4),(-4.85633810213992,-4.85633121754184),
 .UNSPECIFIED.);
#210=B_SPLINE_CURVE_WITH_KNOTS('',3,(#18229,#18230,#18231,#18232,#18233,
#18234,#18235,#18236,#18237,#18238,#18239,#18240,#18241,#18242,#18243,#18244,
#18245,#18246,#18247,#18248,#18249,#18250,#18251,#18252,#18253,#18254,#18255,
#18256,#18257,#18258,#18259,#18260,#18261,#18262,#18263,#18264,#18265,#18266,
#18267,#18268,#18269,#18270,#18271,#18272,#18273,#18274,#18275,#18276,#18277,
#18278,#18279,#18280,#18281,#18282,#18283,#18284,#18285,#18286,#18287,#18288,
#18289,#18290,#18291,#18292,#18293,#18294,#18295,#18296,#18297,#18298,#18299,
#18300,#18301,#18302,#18303,#18304,#18305,#18306,#18307,#18308,#18309,#18310,
#18311,#18312,#18313,#18314,#18315,#18316,#18317,#18318,#18319,#18320,#18321,
#18322,#18323,#18324,#18325,#18326,#18327,#18328,#18329,#18330,#18331,#18332,
#18333,#18334,#18335,#18336,#18337,#18338,#18339,#18340,#18341,#18342,#18343,
#18344,#18345,#18346,#18347,#18348,#18349,#18350,#18351,#18352,#18353,#18354,
#18355,#18356,#18357,#18358,#18359,#18360,#18361,#18362,#18363,#18364,#18365,
#18366,#18367,#18368,#18369,#18370,#18371,#18372,#18373,#18374,#18375,#18376,
#18377,#18378,#18379,#18380,#18381,#18382,#18383,#18384,#18385,#18386,#18387,
#18388,#18389,#18390,#18391,#18392,#18393,#18394,#18395,#18396,#18397,#18398,
#18399,#18400,#18401,#18402,#18403,#18404,#18405,#18406),.UNSPECIFIED.,
 .F.,.F.,(4,2,2,2,2,2,2,2,2,2,2,2,2,2,2,2,2,2,2,2,2,2,2,2,2,2,2,2,2,2,2,
2,2,2,2,2,2,2,2,2,2,2,2,2,2,2,2,2,2,2,2,2,2,2,2,2,2,2,2,2,2,2,2,2,2,2,2,
2,2,2,2,2,2,2,2,2,2,2,2,2,2,2,2,2,2,2,2,2,4),(0.000141208970641106,0.00260421869732101,
0.0052276655840623,0.0097768460544778,0.0172305119182923,0.0501220173560818,
0.0664236905796941,0.0757300526936879,0.0791631109294421,0.0815747821003626,
0.0843414713693197,0.0894007964463044,0.122158036354821,0.138557390784882,
0.149876449259462,0.155175782700374,0.159350568636847,0.164184987943546,
0.172678480141147,0.210890365945431,0.227969106547551,0.232065738371256,
0.234603525100323,0.23716172683167,0.241335891636054,0.25882343157927,0.286510199887536,
0.301740206595418,0.307600734640189,0.311888589272734,0.316468780859696,
0.323892113808258,0.358076836795881,0.373771160545672,0.382869904577255,
0.386278215195521,0.388683195388731,0.391441676684064,0.396518214189327,
0.426670009264769,0.451576415664413,0.459372629966599,0.464001457786102,
0.468219921708977,0.473710730334942,0.485788376105022,0.504690750023019,
0.533932313828317,0.53873116378046,0.541406392559831,0.543848174084512,
0.547461433203641,0.558234193736316,0.579315768765851,0.605461131396945,
0.613275807184344,0.617943501828802,0.622217509627598,0.627912405532227,
0.641771644016302,0.664748194881735,0.686924115465114,0.692149336246089,
0.694936696052987,0.697413109346304,0.700989607490205,0.711057887758149,
0.72977222339771,0.757407061188366,0.76510902159049,0.769781938977176,0.77411278768263,
0.779969035677471,0.794784284402865,0.820580861292412,0.8410739972508,0.845308006048228,
0.847872631386642,0.850264924059376,0.853976226329157,0.867138706639604,
0.899855434061717,0.916853095757379,0.922877344557088,0.926610466523709,
0.930734370267285,0.936631753567681,0.953829720348217,0.971412745929808),
 .UNSPECIFIED.);
#211=B_SPLINE_CURVE_WITH_KNOTS('',3,(#18407,#18408,#18409,#18410,#18411,
#18412,#18413,#18414,#18415,#18416,#18417,#18418,#18419,#18420,#18421,#18422,
#18423,#18424,#18425,#18426,#18427,#18428,#18429,#18430,#18431,#18432,#18433,
#18434,#18435,#18436,#18437,#18438,#18439,#18440,#18441,#18442,#18443,#18444,
#18445,#18446,#18447,#18448,#18449,#18450,#18451,#18452,#18453,#18454,#18455,
#18456,#18457,#18458,#18459,#18460,#18461,#18462,#18463,#18464,#18465,#18466,
#18467,#18468,#18469,#18470,#18471,#18472,#18473,#18474,#18475,#18476,#18477,
#18478,#18479,#18480,#18481,#18482,#18483,#18484,#18485,#18486,#18487,#18488,
#18489,#18490,#18491,#18492,#18493,#18494,#18495,#18496,#18497,#18498,#18499,
#18500,#18501,#18502,#18503,#18504,#18505,#18506,#18507,#18508,#18509,#18510,
#18511,#18512,#18513,#18514,#18515,#18516,#18517,#18518,#18519,#18520,#18521,
#18522,#18523,#18524,#18525,#18526,#18527,#18528,#18529,#18530,#18531,#18532,
#18533,#18534,#18535,#18536,#18537,#18538,#18539,#18540,#18541,#18542,#18543,
#18544,#18545,#18546,#18547,#18548,#18549,#18550,#18551,#18552,#18553,#18554,
#18555,#18556,#18557,#18558,#18559,#18560,#18561,#18562,#18563,#18564,#18565,
#18566,#18567,#18568,#18569,#18570,#18571,#18572,#18573,#18574,#18575,#18576,
#18577,#18578,#18579,#18580,#18581,#18582,#18583,#18584,#18585,#18586,#18587,
#18588),.UNSPECIFIED.,.F.,.F.,(4,2,2,2,2,2,2,2,2,2,2,2,2,2,2,2,2,2,2,2,
2,2,2,2,2,2,2,2,2,2,2,2,2,2,2,2,2,2,2,2,2,2,2,2,2,2,2,2,2,2,2,2,2,2,2,2,
2,2,2,2,2,2,2,2,2,2,2,2,2,2,2,2,2,2,2,2,2,2,2,2,2,2,2,2,2,2,2,2,2,2,4),
(-0.971391456537255,-0.971350475017715,-0.94591226166657,-0.939055866602481,
-0.934491943525297,-0.929966522537624,-0.923315457172628,-0.900084828443717,
-0.866675788733297,-0.861483715642629,-0.858667284068134,-0.856156444610882,
-0.852480155304097,-0.841678563536531,-0.82054319420312,-0.79533261802684,
-0.787491045820371,-0.782733466408728,-0.77832103124467,-0.772342363335511,
-0.75698856882546,-0.728964770759938,-0.712339354105396,-0.708142242501503,
-0.705532704686271,-0.702880771961631,-0.698485355783003,-0.674022702995305,
-0.642599533278312,-0.634880128685733,-0.630145861839832,-0.625722256150309,
-0.619676109637291,-0.603761730423759,-0.5733448179666,-0.564910522641159,
-0.557601689880697,-0.55443107439597,-0.551970146896551,-0.548875717294742,
-0.542206024288379,-0.532494999382091,-0.489582880438121,-0.482087767216936,
-0.477401905795565,-0.472964832662002,-0.466804632427164,-0.449814264601177,
-0.413424403576693,-0.405535496779586,-0.402459473341899,-0.399951900345286,
-0.397132042878921,-0.391921343895885,-0.372654164363047,-0.336263006736024,
-0.329122575864086,-0.324502881571398,-0.320018727171346,-0.313602331443732,
-0.29388634728559,-0.276304617435784,-0.256570434034097,-0.251340125257597,
-0.24851417463144,-0.245996946416581,-0.242316540835892,-0.231540604020166,
-0.210486510775074,-0.185387242102097,-0.177555587523125,-0.172793530995205,
-0.16836913555747,-0.162360818143053,-0.146824797563933,-0.118104728439308,
-0.102309888146275,-0.098139487777396,-0.0955356246830923,-0.0929006792526596,
-0.088522539861798,-0.0830553365089054,-0.070707876555459,-0.0556129729315022,
-0.0325113603607354,-0.0247369510017717,-0.0200127871468392,-0.0158546275414271,
-0.0115824295604963,-0.00654733946174566,-9.40886979550022E-5),
 .UNSPECIFIED.);
#212=B_SPLINE_CURVE_WITH_KNOTS('',3,(#18593,#18594,#18595,#18596,#18597,
#18598,#18599,#18600,#18601,#18602,#18603,#18604,#18605,#18606,#18607,#18608,
#18609,#18610,#18611,#18612,#18613,#18614,#18615,#18616,#18617,#18618,#18619,
#18620,#18621,#18622,#18623,#18624,#18625,#18626,#18627,#18628,#18629,#18630,
#18631,#18632,#18633,#18634,#18635,#18636,#18637,#18638,#18639,#18640,#18641,
#18642,#18643,#18644,#18645,#18646,#18647,#18648,#18649,#18650,#18651,#18652,
#18653,#18654,#18655,#18656,#18657,#18658,#18659,#18660,#18661,#18662,#18663,
#18664,#18665,#18666,#18667,#18668,#18669,#18670,#18671,#18672,#18673,#18674,
#18675,#18676,#18677,#18678,#18679,#18680,#18681,#18682,#18683,#18684,#18685,
#18686,#18687,#18688,#18689,#18690,#18691,#18692,#18693,#18694,#18695,#18696,
#18697,#18698,#18699,#18700,#18701,#18702,#18703,#18704,#18705,#18706,#18707,
#18708,#18709,#18710,#18711,#18712,#18713,#18714,#18715,#18716,#18717,#18718,
#18719,#18720,#18721,#18722,#18723,#18724,#18725,#18726,#18727,#18728,#18729,
#18730,#18731,#18732,#18733,#18734,#18735,#18736,#18737,#18738,#18739,#18740,
#18741,#18742,#18743,#18744,#18745,#18746,#18747,#18748,#18749,#18750,#18751,
#18752,#18753,#18754,#18755,#18756,#18757,#18758,#18759,#18760,#18761,#18762,
#18763,#18764,#18765,#18766,#18767,#18768),.UNSPECIFIED.,.F.,.F.,(4,2,2,
2,2,2,2,2,2,2,2,2,2,2,2,2,2,2,2,2,2,2,2,2,2,2,2,2,2,2,2,2,2,2,2,2,2,2,2,
2,2,2,2,2,2,2,2,2,2,2,2,2,2,2,2,2,2,2,2,2,2,2,2,2,2,2,2,2,2,2,2,2,2,2,2,
2,2,2,2,2,2,2,2,2,2,2,2,4),(-4.85633121754184,-4.85213065139609,-4.84647712007667,
-4.81509163858284,-4.79825979897682,-4.78876865709538,-4.78530539628214,
-4.78288273583215,-4.78011349846824,-4.7750701610028,-4.74952354545192,
-4.72855908723541,-4.71538188389384,-4.70978571060111,-4.70552965445536,
-4.70082677238956,-4.69281250170212,-4.65374878230526,-4.63651598370295,
-4.63240505707741,-4.62985974897014,-4.62730253249263,-4.62313232718254,
-4.60581215907345,-4.57782671807124,-4.56249583090281,-4.55661704711339,
-4.55232213524437,-4.54774021309657,-4.54032700092237,-4.50611548905706,
-4.4904787062145,-4.48139560604128,-4.47798324594874,-4.47556663890993,
-4.47276988568106,-4.46759538793662,-4.4469975552687,-4.42839427299879,
-4.41579147273591,-4.40632672287472,-4.40134419610195,-4.39712653939579,
-4.39196322116091,-4.38149899293316,-4.34576805751086,-4.3291871500724,
-4.32511116833149,-4.32257420413104,-4.32001020944753,-4.3158074141098,
-4.29765351873152,-4.27033522323949,-4.2551758391028,-4.24931760071498,
-4.24502565608104,-4.24043587806352,-4.23298424974857,-4.1991058388011,
-4.18330012692505,-4.17699819205573,-4.17214266234621,-4.16944123140104,
-4.1670201152808,-4.1640022471072,-4.15612700531233,-4.11979209381665,-4.10217771943166,
-4.0960492225731,-4.09171332297588,-4.08774491599307,-4.08121543145688,
-4.06038638190995,-4.03660661272028,-4.0217184107034,-4.01774498588615,
-4.01522918083307,-4.01264060239549,-4.00832142166615,-3.98491873872065,
-3.96283719571124,-3.94786173772201,-3.94202651256228,-3.93773842295176,
-3.93314082421309,-3.92564856185857,-3.89212701756681,-3.88485527042599),
 .UNSPECIFIED.);
#213=B_SPLINE_CURVE_WITH_KNOTS('',3,(#18770,#18771,#18772,#18773,#18774,
#18775,#18776,#18777,#18778,#18779,#18780,#18781,#18782,#18783,#18784,#18785,
#18786,#18787,#18788,#18789,#18790,#18791,#18792,#18793,#18794,#18795,#18796,
#18797,#18798,#18799,#18800,#18801,#18802,#18803,#18804,#18805,#18806,#18807,
#18808,#18809,#18810,#18811,#18812,#18813,#18814,#18815,#18816,#18817,#18818,
#18819,#18820,#18821,#18822,#18823,#18824,#18825,#18826,#18827,#18828,#18829,
#18830,#18831,#18832,#18833,#18834,#18835,#18836,#18837,#18838,#18839,#18840,
#18841,#18842,#18843,#18844,#18845,#18846,#18847,#18848,#18849,#18850,#18851,
#18852,#18853,#18854,#18855,#18856,#18857,#18858,#18859,#18860,#18861,#18862,
#18863,#18864,#18865,#18866,#18867,#18868,#18869,#18870,#18871,#18872,#18873,
#18874,#18875,#18876,#18877,#18878,#18879,#18880,#18881,#18882,#18883,#18884,
#18885,#18886,#18887,#18888,#18889,#18890,#18891,#18892,#18893,#18894,#18895,
#18896,#18897,#18898,#18899,#18900,#18901,#18902,#18903,#18904,#18905,#18906,
#18907,#18908,#18909,#18910,#18911,#18912,#18913,#18914,#18915,#18916,#18917,
#18918,#18919,#18920,#18921,#18922,#18923,#18924,#18925,#18926,#18927,#18928,
#18929,#18930,#18931,#18932,#18933,#18934,#18935,#18936,#18937,#18938,#18939,
#18940,#18941,#18942,#18943,#18944,#18945,#18946,#18947,#18948,#18949),
 .UNSPECIFIED.,.F.,.F.,(4,2,2,2,2,2,2,2,2,2,2,2,2,2,2,2,2,2,2,2,2,2,2,2,
2,2,2,2,2,2,2,2,2,2,2,2,2,2,2,2,2,2,2,2,2,2,2,2,2,2,2,2,2,2,2,2,2,2,2,2,
2,2,2,2,2,2,2,2,2,2,2,2,2,2,2,2,2,2,2,2,2,2,2,2,2,2,2,2,2,4),(-1.94269089166418,
-1.93517126631823,-1.93043333031223,-1.92786163297422,-1.92553536015628,
-1.92280532619892,-1.91803394431714,-1.89257796006248,-1.87521637487989,
-1.85925975941574,-1.85320984431279,-1.84878693253339,-1.84405669275704,
-1.83635192095474,-1.80474817087353,-1.78807814579666,-1.77861330164555,
-1.77509630832447,-1.77260867024126,-1.76971426813013,-1.76413130798493,
-1.72451055249351,-1.70709282269508,-1.70088554182812,-1.69643807008872,
-1.69176164519176,-1.6843267070496,-1.65018390868158,-1.6349011240992,-1.62868924094152,
-1.62386396573735,-1.62112286042163,-1.61860796391698,-1.61476212732756,
-1.60325377303154,-1.57221947927429,-1.55461691378427,-1.54839093462721,
-1.54394024355143,-1.5392693116814,-1.53186285436495,-1.4974924177766,-1.47704377309018,
-1.47170592584779,-1.46886008183724,-1.46635918549734,-1.46332036842669,
-1.45569326796168,-1.41897825334754,-1.40193593124306,-1.39576718039066,
-1.39132592330984,-1.38663716530924,-1.3791401304918,-1.34060260362163,
-1.32827031598642,-1.32279955547753,-1.31841370662874,-1.31576482604718,
-1.31315484570357,-1.30895356582117,-1.29223604561974,-1.26426876913352,
-1.24892766355139,-1.24295068925588,-1.23853883800795,-1.2337812834758,
-1.22593814368876,-1.20005736734272,-1.17945799774462,-1.16880260208862,
-1.16514274803746,-1.1626344563469,-1.15981042358652,-1.15458141811861,
-1.13486316357308,-1.11599121466708,-1.09728664369118,-1.09095635205127,
-1.08648786296795,-1.08184677873542,-1.07459311863954,-1.03907910966406,
-1.01933714810872,-1.01407451481946,-1.0112436859667,-1.00873791278509,
-1.00567541865444,-0.999413749447903,-0.971391456537255),.UNSPECIFIED.);
#214=B_SPLINE_CURVE_WITH_KNOTS('',3,(#18950,#18951,#18952,#18953),
 .UNSPECIFIED.,.F.,.F.,(4,4),(-5.03931041703063E-5,-9.99999999955958E-7),
 .UNSPECIFIED.);
#215=B_SPLINE_CURVE_WITH_KNOTS('',3,(#18958,#18959,#18960,#18961,#18962,
#18963,#18964,#18965,#18966,#18967,#18968,#18969,#18970,#18971,#18972,#18973,
#18974,#18975,#18976,#18977,#18978,#18979,#18980,#18981,#18982,#18983,#18984,
#18985,#18986,#18987,#18988,#18989,#18990,#18991,#18992,#18993,#18994,#18995,
#18996,#18997,#18998,#18999,#19000,#19001,#19002,#19003,#19004,#19005,#19006,
#19007,#19008,#19009,#19010,#19011,#19012,#19013,#19014,#19015,#19016,#19017,
#19018,#19019,#19020,#19021,#19022,#19023,#19024,#19025,#19026,#19027,#19028,
#19029,#19030,#19031,#19032,#19033,#19034,#19035,#19036,#19037,#19038,#19039,
#19040,#19041,#19042,#19043,#19044,#19045,#19046,#19047,#19048,#19049,#19050,
#19051,#19052,#19053,#19054,#19055,#19056,#19057,#19058,#19059,#19060,#19061,
#19062,#19063,#19064,#19065,#19066,#19067,#19068,#19069,#19070,#19071,#19072,
#19073,#19074,#19075,#19076,#19077,#19078,#19079,#19080,#19081,#19082,#19083,
#19084,#19085,#19086,#19087,#19088,#19089,#19090,#19091,#19092,#19093,#19094,
#19095,#19096,#19097,#19098,#19099,#19100,#19101,#19102,#19103,#19104,#19105,
#19106,#19107,#19108,#19109,#19110,#19111,#19112,#19113,#19114,#19115,#19116,
#19117,#19118,#19119,#19120,#19121,#19122,#19123,#19124,#19125,#19126,#19127,
#19128,#19129,#19130,#19131,#19132,#19133,#19134,#19135,#19136,#19137,#19138,
#19139,#19140,#19141),.UNSPECIFIED.,.F.,.F.,(4,2,2,2,2,2,2,2,2,2,2,2,2,
2,2,2,2,2,2,2,2,2,2,2,2,2,2,2,2,2,2,2,2,2,2,2,2,2,2,2,2,2,2,2,2,2,2,2,2,
2,2,2,2,2,2,2,2,2,2,2,2,2,2,2,2,2,2,2,2,2,2,2,2,2,2,2,2,2,2,2,2,2,2,2,2,
2,2,2,2,2,2,4),(-3.88485527042599,-3.87612942688473,-3.86692044470073,-3.86349153731901,
-3.86107257062718,-3.85828415396544,-3.85314986936548,-3.83333871713199,
-3.81620582124791,-3.79554569255171,-3.78915634087622,-3.78477394437684,
-3.78033504307713,-3.77364604115463,-3.74852033650871,-3.72943267851357,
-3.71450137835232,-3.71052510579754,-3.70800873290492,-3.70542091489492,
-3.70110519033777,-3.67776277543455,-3.65576783747023,-3.64067702214714,
-3.63482764500726,-3.6305374713829,-3.62594527333001,-3.61847969068087,
-3.58472537830717,-3.56885372918825,-3.55968859064669,-3.55626545207974,
-3.55384732491795,-3.55105601839559,-3.54590777953046,-3.52577729066484,
-3.50121160951107,-3.4868336778872,-3.48107453324816,-3.4767977861641,-3.47217062463026,
-3.464530214041,-3.4265206417358,-3.41369232636088,-3.40567341917178,-3.40241026570776,
-3.40001061219079,-3.39712333543128,-3.39133091879335,-3.35149730986139,
-3.3340332722328,-3.3279203483318,-3.32358760248186,-3.31961685512853,-3.31307117766192,
-3.29189576157376,-3.26853402696514,-3.25362519952796,-3.24965080394012,
-3.24713502918839,-3.2445471729515,-3.24023032986175,-3.216862172777,-3.19482835978413,
-3.17979514314729,-3.17395332523438,-3.16966470088453,-3.16507048997968,
-3.15759303466847,-3.12395452658673,-3.10802504654718,-3.09884021816107,
-3.09541476698086,-3.09299655139007,-3.09020699420807,-3.0850660896511,
-3.06508406113471,-3.04741826210348,-3.03394630531244,-3.0240292898885,
-3.01896370630131,-3.01474788399437,-3.00967462757103,-3.00003076781016,
-2.96340500896624,-2.94664413792194,-2.94255877751648,-2.94001993078873,
-2.93745851883094,-2.93326652107717,-2.91540016853139,-2.91349531428362),
 .UNSPECIFIED.);
#216=B_SPLINE_CURVE_WITH_KNOTS('',3,(#19142,#19143,#19144,#19145,#19146,
#19147,#19148,#19149,#19150,#19151,#19152,#19153,#19154,#19155,#19156,#19157,
#19158,#19159,#19160,#19161,#19162,#19163,#19164,#19165,#19166,#19167,#19168,
#19169,#19170,#19171,#19172,#19173,#19174,#19175,#19176,#19177,#19178,#19179,
#19180,#19181,#19182,#19183,#19184,#19185,#19186,#19187,#19188,#19189,#19190,
#19191,#19192,#19193,#19194,#19195,#19196,#19197,#19198,#19199,#19200,#19201,
#19202,#19203,#19204,#19205,#19206,#19207,#19208,#19209,#19210,#19211,#19212,
#19213,#19214,#19215,#19216,#19217,#19218,#19219,#19220,#19221,#19222,#19223,
#19224,#19225,#19226,#19227,#19228,#19229,#19230,#19231,#19232,#19233,#19234,
#19235,#19236,#19237,#19238,#19239,#19240,#19241,#19242,#19243,#19244,#19245,
#19246,#19247,#19248,#19249,#19250,#19251,#19252,#19253,#19254,#19255,#19256,
#19257,#19258,#19259,#19260,#19261,#19262,#19263,#19264,#19265,#19266,#19267,
#19268,#19269,#19270,#19271,#19272,#19273,#19274,#19275,#19276,#19277,#19278,
#19279,#19280,#19281,#19282,#19283,#19284,#19285,#19286,#19287,#19288,#19289,
#19290,#19291,#19292,#19293,#19294,#19295,#19296,#19297,#19298,#19299,#19300,
#19301,#19302,#19303,#19304,#19305,#19306,#19307,#19308,#19309,#19310,#19311,
#19312,#19313),.UNSPECIFIED.,.F.,.F.,(4,2,2,2,2,2,2,2,2,2,2,2,2,2,2,2,2,
2,2,2,2,2,2,2,2,2,2,2,2,2,2,2,2,2,2,2,2,2,2,2,2,2,2,2,2,2,2,2,2,2,2,2,2,
2,2,2,2,2,2,2,2,2,2,2,2,2,2,2,2,2,2,2,2,2,2,2,2,2,2,2,2,2,2,2,2,4),(-0.971153636545791,
-0.971008594948987,-0.965153140353171,-0.95076796891759,-0.926253312146383,
-0.90671530802577,-0.901494145309361,-0.89867202134374,-0.896163631368954,
-0.892501243608833,-0.881821284397918,-0.861131733116912,-0.835352323870838,
-0.827509082887044,-0.822751871248581,-0.818340630311989,-0.812364916031061,
-0.797028470229962,-0.769069200644485,-0.752372464055914,-0.748172865866162,
-0.745563418770317,-0.742914593343789,-0.738527914593733,-0.713956050207449,
-0.682628402926648,-0.674902030268896,-0.670168151700236,-0.665748074128256,
-0.659711984422174,-0.643865552001454,-0.613741869417596,-0.599615662445248,
-0.595543574305058,-0.593215185351513,-0.590611055995399,-0.586436796558227,
-0.569165018086564,-0.529000858285284,-0.52183672145698,-0.517213947677662,
-0.512735529760769,-0.506342893017696,-0.486899844471605,-0.462578022509873,
-0.447258910048538,-0.443111883548401,-0.440769822998353,-0.438181882272539,
-0.434086121713075,-0.418245765591886,-0.394401111842103,-0.375077375664371,
-0.368594007728611,-0.364144264275441,-0.359553818730779,-0.352556450278034,
-0.323932613112025,-0.296283664564022,-0.291322307551835,-0.288553280531884,
-0.286023139790771,-0.282230708438604,-0.27030305615395,-0.244409759413656,
-0.222958751252185,-0.216306730914958,-0.212233208575315,-0.207751323681161,
-0.201340042475556,-0.181673786527202,-0.164031378728836,-0.144274319040584,
-0.139042083772736,-0.136217773264899,-0.133710255969495,-0.130053059538382,
-0.119418783112649,-0.0988954692710536,-0.0728956763044899,-0.0650518898003542,
-0.0602946576044903,-0.0558835931377834,-0.0499084241794123,-0.0345755390114698,
-5.03931041703063E-5),.UNSPECIFIED.);
#217=B_SPLINE_CURVE_WITH_KNOTS('',3,(#19318,#19319,#19320,#19321,#19322,
#19323,#19324,#19325,#19326,#19327,#19328,#19329,#19330,#19331,#19332,#19333,
#19334,#19335,#19336,#19337,#19338,#19339,#19340,#19341,#19342,#19343,#19344,
#19345,#19346,#19347,#19348,#19349,#19350,#19351,#19352,#19353,#19354,#19355,
#19356,#19357,#19358,#19359,#19360,#19361,#19362,#19363,#19364,#19365,#19366,
#19367,#19368,#19369,#19370,#19371,#19372,#19373,#19374,#19375,#19376,#19377,
#19378,#19379,#19380,#19381,#19382,#19383,#19384,#19385,#19386,#19387,#19388,
#19389,#19390,#19391,#19392,#19393,#19394,#19395,#19396,#19397,#19398,#19399,
#19400,#19401,#19402,#19403,#19404,#19405,#19406,#19407,#19408,#19409,#19410,
#19411,#19412,#19413,#19414,#19415,#19416,#19417,#19418,#19419,#19420,#19421,
#19422,#19423,#19424,#19425,#19426,#19427,#19428,#19429,#19430,#19431,#19432,
#19433,#19434,#19435,#19436,#19437,#19438,#19439,#19440,#19441,#19442,#19443,
#19444,#19445,#19446,#19447,#19448,#19449,#19450,#19451,#19452,#19453,#19454,
#19455,#19456,#19457,#19458,#19459,#19460,#19461,#19462,#19463,#19464,#19465,
#19466,#19467,#19468,#19469,#19470,#19471,#19472,#19473,#19474,#19475,#19476,
#19477,#19478,#19479,#19480,#19481,#19482,#19483,#19484,#19485,#19486,#19487,
#19488,#19489,#19490,#19491,#19492,#19493,#19494,#19495,#19496,#19497,#19498,
#19499),.UNSPECIFIED.,.F.,.F.,(4,2,2,2,2,2,2,2,2,2,2,2,2,2,2,2,2,2,2,2,
2,2,2,2,2,2,2,2,2,2,2,2,2,2,2,2,2,2,2,2,2,2,2,2,2,2,2,2,2,2,2,2,2,2,2,2,
2,2,2,2,2,2,2,2,2,2,2,2,2,2,2,2,2,2,2,2,2,2,2,2,2,2,2,2,2,2,2,2,2,2,4),
(-2.91349531428362,-2.88785921300174,-2.8726430027449,-2.86677863205918,
-2.86248643922693,-2.85790029096159,-2.85046367156569,-2.81646981931229,
-2.8007280660255,-2.79160863757645,-2.78819166947628,-2.78577453314058,
-2.78298032492328,-2.7778177001423,-2.75740712949668,-2.73825152738121,
-2.72583812859598,-2.71647441260755,-2.71151088112635,-2.70729248773251,
-2.70210703845323,-2.69390586646746,-2.6591339369195,-2.64588606824007,
-2.63769869396671,-2.63441089253566,-2.63200904157476,-2.62913865956645,
-2.6234339484568,-2.58348277115152,-2.56600629696093,-2.55989253487532,
-2.55555995071342,-2.55158985421312,-2.54504643819555,-2.52390841910659,
-2.50029087033371,-2.49029362580967,-2.48351409579007,-2.480449193245,-2.4780605078139,
-2.47501214793163,-2.46832900078042,-2.45915292464736,-2.42810789893616,
-2.41232853260371,-2.40625822001906,-2.40197600471217,-2.39746852318833,
-2.39042469203808,-2.38200394689515,-2.36369363346378,-2.33336593040561,
-2.32867955052637,-2.32601391858675,-2.3235491164382,-2.31983572683312,
-2.30811366746104,-2.28309948628011,-2.2599663128295,-2.25335383883438,
-2.24893029326256,-2.24453614668166,-2.23807947644657,-2.21642727345666,
-2.19829989391596,-2.17894872278306,-2.17472001156547,-2.1721509942611,
-2.16961971164294,-2.16556936904969,-2.14944123261186,-2.12563610681186,
-2.10603499553312,-2.09958972783228,-2.09563623816902,-2.09128861274927,
-2.08508808823211,-2.06670303492164,-2.04752070148475,-2.027147259442,-2.02198742240317,
-2.01919398856709,-2.01677702398121,-2.01335958053459,-2.00423504373367,
-1.98847734663213,-1.95449285532475,-1.94705346079759,-1.94246711155014,
-1.94225105833858),.UNSPECIFIED.);
#218=B_SPLINE_CURVE_WITH_KNOTS('',3,(#19500,#19501,#19502,#19503,#19504,
#19505,#19506,#19507,#19508,#19509,#19510,#19511,#19512,#19513,#19514,#19515,
#19516,#19517,#19518,#19519,#19520,#19521,#19522,#19523,#19524,#19525,#19526,
#19527,#19528,#19529,#19530,#19531,#19532,#19533,#19534,#19535,#19536,#19537,
#19538,#19539,#19540,#19541,#19542,#19543,#19544,#19545,#19546,#19547,#19548,
#19549,#19550,#19551,#19552,#19553,#19554,#19555,#19556,#19557,#19558,#19559,
#19560,#19561,#19562,#19563,#19564,#19565,#19566,#19567,#19568,#19569,#19570,
#19571,#19572,#19573,#19574,#19575,#19576,#19577,#19578,#19579,#19580,#19581,
#19582,#19583,#19584,#19585,#19586,#19587,#19588,#19589,#19590,#19591,#19592,
#19593,#19594,#19595,#19596,#19597,#19598,#19599,#19600,#19601,#19602,#19603,
#19604,#19605,#19606,#19607,#19608,#19609,#19610,#19611,#19612,#19613,#19614,
#19615,#19616,#19617,#19618,#19619,#19620,#19621,#19622,#19623,#19624,#19625,
#19626,#19627,#19628,#19629,#19630,#19631,#19632,#19633,#19634,#19635,#19636,
#19637,#19638,#19639,#19640,#19641,#19642,#19643,#19644,#19645,#19646,#19647,
#19648,#19649,#19650,#19651,#19652,#19653,#19654,#19655,#19656,#19657,#19658,
#19659,#19660,#19661,#19662,#19663,#19664,#19665,#19666,#19667,#19668,#19669,
#19670,#19671,#19672,#19673),.UNSPECIFIED.,.F.,.F.,(4,2,2,2,2,2,2,2,2,2,
2,2,2,2,2,2,2,2,2,2,2,2,2,2,2,2,2,2,2,2,2,2,2,2,2,2,2,2,2,2,2,2,2,2,2,2,
2,2,2,2,2,2,2,2,2,2,2,2,2,2,2,2,2,2,2,2,2,2,2,2,2,2,2,2,2,2,2,2,2,2,2,2,
2,2,2,2,4),(-1.94245618738083,-1.93666604794167,-1.90204794308009,-1.89466971332662,
-1.89000414570624,-1.88555010505709,-1.87930511456366,-1.86150959565628,
-1.84248742044491,-1.82190397686627,-1.81663235642541,-1.81379978161942,
-1.8112944826846,-1.80765376515567,-1.79716872592755,-1.77718374838492,
-1.75044607779919,-1.74260114083196,-1.73784309629813,-1.73343120666949,
-1.72745480759043,-1.71211797648903,-1.68416231528133,-1.66745337302565,
-1.6632526590439,-1.6606427107058,-1.65799358232213,-1.65360673403587,-1.64813392266078,
-1.63579470820685,-1.59724524016339,-1.58974619776021,-1.58505694537765,
-1.58061575981501,-1.57444797141161,-1.55741343123057,-1.52073045017774,
-1.51309191974478,-1.51005139105216,-1.50755014135901,-1.50470548247491,
-1.49937336423293,-1.4789803418051,-1.44449618557995,-1.43710156101452,
-1.43243304053073,-1.42798123994456,-1.42174793734908,-1.40406750826335,
-1.38483827982886,-1.36431858492595,-1.35905146718736,-1.35621995243168,
-1.35371459476435,-1.35007240956499,-1.33957267411533,-1.31953415473493,
-1.29287412174753,-1.28502968466071,-1.28027201711475,-1.2758605236468,
-1.26988473431397,-1.25454998511729,-1.22659974312072,-1.20988862582101,
-1.20568810136917,-1.20307834315922,-1.20042948546114,-1.19604321065498,
-1.17138803697016,-1.14015161558894,-1.13241791790184,-1.12768236692295,
-1.12326253877635,-1.11722967994469,-1.10141348586324,-1.07142877420758,
-1.05714431415319,-1.05306015150634,-1.05072945077579,-1.048127766341,-1.04396593742351,
-1.02694592560699,-0.988307700660695,-0.980210340516297,-0.97540285891718,
-0.971153636545791),.UNSPECIFIED.);
#219=B_SPLINE_CURVE_WITH_KNOTS('',3,(#19678,#19679,#19680,#19681,#19682,
#19683,#19684,#19685,#19686,#19687,#19688,#19689,#19690,#19691,#19692,#19693,
#19694,#19695,#19696,#19697,#19698,#19699,#19700,#19701,#19702,#19703,#19704,
#19705,#19706,#19707,#19708,#19709,#19710,#19711,#19712,#19713,#19714,#19715,
#19716,#19717,#19718,#19719,#19720,#19721,#19722,#19723,#19724,#19725,#19726,
#19727,#19728,#19729,#19730,#19731,#19732,#19733,#19734,#19735,#19736,#19737,
#19738,#19739,#19740,#19741,#19742,#19743,#19744,#19745,#19746,#19747,#19748,
#19749,#19750,#19751,#19752,#19753,#19754,#19755,#19756,#19757,#19758,#19759,
#19760,#19761,#19762,#19763,#19764,#19765,#19766,#19767,#19768,#19769,#19770,
#19771,#19772,#19773,#19774,#19775,#19776,#19777,#19778,#19779,#19780,#19781,
#19782,#19783,#19784,#19785,#19786,#19787,#19788,#19789,#19790,#19791,#19792,
#19793,#19794,#19795,#19796,#19797,#19798,#19799,#19800,#19801,#19802,#19803,
#19804,#19805,#19806,#19807,#19808,#19809,#19810,#19811,#19812,#19813,#19814,
#19815,#19816,#19817,#19818,#19819,#19820,#19821,#19822,#19823,#19824,#19825,
#19826,#19827,#19828,#19829,#19830,#19831,#19832,#19833,#19834,#19835,#19836,
#19837,#19838,#19839,#19840,#19841,#19842,#19843,#19844,#19845,#19846,#19847,
#19848,#19849,#19850,#19851,#19852,#19853,#19854,#19855),.UNSPECIFIED.,
 .F.,.F.,(4,2,2,2,2,2,2,2,2,2,2,2,2,2,2,2,2,2,2,2,2,2,2,2,2,2,2,2,2,2,2,
2,2,2,2,2,2,2,2,2,2,2,2,2,2,2,2,2,2,2,2,2,2,2,2,2,2,2,2,2,2,2,2,2,2,2,2,
2,2,2,2,2,2,2,2,2,2,2,2,2,2,2,2,2,2,2,2,2,4),(-1.94225105833858,-1.93817574801027,
-1.93231411518889,-1.91711500751957,-1.88963102947338,-1.87172412036913,
-1.86753138927278,-1.8649700191301,-1.86243177847413,-1.8583481593741,-1.84161793735377,
-1.80515530132293,-1.795380257346,-1.79028208426469,-1.78606669827375,-1.78102681224781,
-1.77124795889596,-1.73973914369167,-1.719912592923,-1.71477931531364,-1.71199154432955,
-1.70957320869571,-1.70614527105133,-1.69693999447017,-1.68095029460128,
-1.64740248617903,-1.63991313286521,-1.6353168705613,-1.63102976626463,
-1.6251954438425,-1.61021784625178,-1.58816155316777,-1.56478150171211,
-1.56046398562556,-1.55787617832783,-1.55536095068415,-1.5513880750123,
-1.53649964166235,-1.51269756471832,-1.49188165487078,-1.48535372135347,
-1.48138635901469,-1.47705172621421,-1.47092519036825,-1.45331554879081,
-1.41749445323066,-1.40922488689507,-1.40584696409475,-1.40343514035856,
-1.400620134993,-1.39519912177293,-1.38788544959407,-1.3670881388276,-1.34080726817211,
-1.33301890460348,-1.32836274674951,-1.32409675309266,-1.31840930426554,
-1.30456333433945,-1.2816664608601,-1.25919555634037,-1.25404859301556,
-1.25125790778109,-1.24884029374826,-1.24541780555451,-1.23625448984316,
-1.22038566594815,-1.1866117703993,-1.17914796741874,-1.17455678542318,
-1.17026754163774,-1.1644193812063,-1.14932995360108,-1.12226165345558,
-1.10383073725108,-1.09962093371131,-1.09705596718609,-1.09452113217626,
-1.09045361213551,-1.07401965479348,-1.0457268751906,-1.0300686358062,-1.02400990891724,
-1.01972965461697,-1.01521888392003,-1.00815824775775,-0.98876999730182,
-0.971774429615847,-0.971085382281135),.UNSPECIFIED.);
#220=B_SPLINE_CURVE_WITH_KNOTS('',3,(#19856,#19857,#19858,#19859,#19860,
#19861,#19862,#19863,#19864,#19865,#19866,#19867,#19868,#19869,#19870,#19871,
#19872,#19873,#19874,#19875,#19876,#19877,#19878,#19879,#19880,#19881,#19882,
#19883,#19884,#19885,#19886,#19887,#19888,#19889,#19890,#19891,#19892,#19893,
#19894,#19895,#19896,#19897,#19898,#19899,#19900,#19901,#19902,#19903,#19904,
#19905,#19906,#19907,#19908,#19909,#19910,#19911,#19912,#19913,#19914,#19915,
#19916,#19917,#19918,#19919,#19920,#19921,#19922,#19923,#19924,#19925,#19926,
#19927,#19928,#19929,#19930,#19931,#19932,#19933,#19934,#19935,#19936,#19937,
#19938,#19939,#19940,#19941,#19942,#19943,#19944,#19945,#19946,#19947,#19948,
#19949,#19950,#19951,#19952,#19953,#19954,#19955,#19956,#19957,#19958,#19959,
#19960,#19961,#19962,#19963,#19964,#19965,#19966,#19967,#19968,#19969,#19970,
#19971,#19972,#19973,#19974,#19975,#19976,#19977,#19978,#19979,#19980,#19981,
#19982,#19983,#19984,#19985,#19986,#19987,#19988,#19989,#19990,#19991,#19992,
#19993,#19994,#19995,#19996,#19997,#19998,#19999,#20000,#20001,#20002,#20003,
#20004,#20005,#20006,#20007,#20008,#20009,#20010,#20011,#20012,#20013,#20014,
#20015,#20016,#20017,#20018,#20019,#20020,#20021,#20022,#20023,#20024,#20025,
#20026,#20027,#20028,#20029,#20030,#20031,#20032,#20033,#20034,#20035),
 .UNSPECIFIED.,.F.,.F.,(4,2,2,2,2,2,2,2,2,2,2,2,2,2,2,2,2,2,2,2,2,2,2,2,
2,2,2,2,2,2,2,2,2,2,2,2,2,2,2,2,2,2,2,2,2,2,2,2,2,2,2,2,2,2,2,2,2,2,2,2,
2,2,2,2,2,2,2,2,2,2,2,2,2,2,2,2,2,2,2,2,2,2,2,2,2,2,2,2,2,4),(-2.91390510725203,
-2.90506916989555,-2.88772673429663,-2.8835480860879,-2.8809423704627,-2.87861359182467,
-2.87454254971778,-2.86044734758774,-2.83026176834386,-2.81439641115966,
-2.80835642733313,-2.80393451095304,-2.79919960570182,-2.79147369713496,
-2.76012189440003,-2.73557156460837,-2.73118505816924,-2.72853566313497,
-2.7259250364792,-2.72172250438345,-2.70499398005282,-2.67702817031134,
-2.66168584902575,-2.65570787327748,-2.65129512960579,-2.64653646712782,
-2.63869114627471,-2.6126222420344,-2.59215471299504,-2.58153453166287,
-2.57787815246974,-2.5753700689154,-2.57254382937296,-2.56730509631592,
-2.54736467729883,-2.52861598188627,-2.50999173565466,-2.50366784824209,
-2.49919992865341,-2.49455609451121,-2.48729097506967,-2.45184326922799,
-2.4371964058279,-2.42844302550073,-2.42535639556814,-2.42284501514053,
-2.420028027468,-2.41483495373192,-2.3957295454715,-2.35910993658772,-2.35200981835196,
-2.34739843873784,-2.3429095787987,-2.33646386555045,-2.31638148401164,
-2.29909437824261,-2.27944481753455,-2.27421846504341,-2.27139486389236,
-2.26888614771493,-2.26522465745816,-2.25455806149966,-2.23392189313628,
-2.2080583944128,-2.20021292232938,-2.19545449055155,-2.19104220230369,
-2.18506520124496,-2.16972638699072,-2.14176573463677,-2.12505839436397,
-2.12085745960638,-2.11824731279366,-2.11559791678661,-2.11121051920109,
-2.10573695657757,-2.09339565663989,-2.05484541326446,-2.04734518869667,
-2.04265542025411,-2.03821389526489,-2.03204588294094,-2.01501288953075,
-1.97834784318526,-1.970691107395,-1.9676476134136,-1.96514559019334,-1.96230241920289,
-1.95697850885554,-1.94245618738083),.UNSPECIFIED.);
#221=B_SPLINE_CURVE_WITH_KNOTS('',3,(#20041,#20042,#20043,#20044),
 .UNSPECIFIED.,.F.,.F.,(4,4),(0.971411654023308,0.971463527532095),
 .UNSPECIFIED.);
#222=B_SPLINE_CURVE_WITH_KNOTS('',3,(#20045,#20046,#20047,#20048,#20049,
#20050,#20051,#20052,#20053,#20054,#20055,#20056,#20057,#20058,#20059,#20060,
#20061,#20062,#20063,#20064,#20065,#20066,#20067,#20068,#20069,#20070,#20071,
#20072,#20073,#20074,#20075,#20076,#20077,#20078,#20079,#20080,#20081,#20082,
#20083,#20084,#20085,#20086,#20087,#20088,#20089,#20090,#20091,#20092,#20093,
#20094,#20095,#20096,#20097,#20098,#20099,#20100,#20101,#20102,#20103,#20104,
#20105,#20106,#20107,#20108,#20109,#20110,#20111,#20112,#20113,#20114,#20115,
#20116,#20117,#20118,#20119,#20120,#20121,#20122,#20123,#20124,#20125,#20126,
#20127,#20128,#20129,#20130,#20131,#20132,#20133,#20134,#20135,#20136,#20137,
#20138,#20139,#20140,#20141,#20142,#20143,#20144,#20145,#20146,#20147,#20148,
#20149,#20150,#20151,#20152,#20153,#20154,#20155,#20156,#20157,#20158,#20159,
#20160,#20161,#20162,#20163,#20164,#20165,#20166,#20167,#20168,#20169,#20170,
#20171,#20172,#20173,#20174,#20175,#20176,#20177,#20178,#20179,#20180,#20181,
#20182,#20183,#20184,#20185,#20186,#20187,#20188,#20189,#20190,#20191,#20192,
#20193,#20194,#20195,#20196,#20197,#20198,#20199,#20200,#20201,#20202,#20203,
#20204,#20205,#20206,#20207,#20208,#20209,#20210,#20211,#20212,#20213,#20214,
#20215,#20216,#20217,#20218,#20219,#20220,#20221,#20222,#20223,#20224,#20225,
#20226,#20227,#20228),.UNSPECIFIED.,.F.,.F.,(4,2,2,2,2,2,2,2,2,2,2,2,2,
2,2,2,2,2,2,2,2,2,2,2,2,2,2,2,2,2,2,2,2,2,2,2,2,2,2,2,2,2,2,2,2,2,2,2,2,
2,2,2,2,2,2,2,2,2,2,2,2,2,2,2,2,2,2,2,2,2,2,2,2,2,2,2,2,2,2,2,2,2,2,2,2,
2,2,2,2,2,2,4),(-0.971085382281135,-0.952017792902401,-0.946887432167989,
-0.944100295124911,-0.941681821236157,-0.938252749983855,-0.929038611127879,
-0.913023210440452,-0.879523662738073,-0.872029045202164,-0.867431756175606,
-0.863145118166893,-0.857313684147572,-0.842359088763997,-0.820286139752394,
-0.796894438362392,-0.79257632409696,-0.789988405026593,-0.787473312643114,
-0.783501009954662,-0.768620603544608,-0.744673319203854,-0.723979872911306,
-0.717458520787705,-0.713492309834453,-0.709156757727181,-0.703024669862699,
-0.685358114282465,-0.65359169314679,-0.642232113050811,-0.638459384428977,
-0.636008118489447,-0.633371235784275,-0.628821535758767,-0.623041560473158,
-0.609403794671107,-0.573020454850763,-0.565176371485666,-0.560509312757121,
-0.556247032331601,-0.550585160075782,-0.536923941376815,-0.514576124664695,
-0.491216671566923,-0.486125177869648,-0.48334636199671,-0.48092577991027,
-0.477480959993249,-0.468144152881925,-0.451770477933558,-0.418925052205649,
-0.411361974473767,-0.406751108100979,-0.402470006324611,-0.396674683919592,
-0.382006200663234,-0.356452120365438,-0.336009594444376,-0.331774337944482,
-0.329204078843861,-0.326674365941362,-0.322630720333002,-0.306612701948914,
-0.280508397917966,-0.277886164043204,-0.262211200634713,-0.25615115654366,
-0.251870919348402,-0.247360986889347,-0.24030345927568,-0.209476177528243,
-0.183985304908225,-0.178943418322464,-0.176175112575443,-0.173751473514796,
-0.170285537214507,-0.160782937797474,-0.143915852684806,-0.111923197089701,
-0.104281902724935,-0.0996552709832551,-0.0953797221880297,-0.0896232712769271,
-0.0752578316239034,-0.0628013904956974,-0.0323914044481022,-0.0260414146726733,
-0.0230517243937155,-0.0206616239994298,-0.0183163031974911,-0.0151902078220476,
-1.00000003733225E-6),.UNSPECIFIED.);
#223=B_SPLINE_CURVE_WITH_KNOTS('',3,(#20229,#20230,#20231,#20232,#20233,
#20234,#20235,#20236,#20237,#20238,#20239,#20240,#20241,#20242,#20243,#20244,
#20245,#20246,#20247,#20248,#20249,#20250,#20251,#20252,#20253,#20254,#20255,
#20256,#20257,#20258,#20259,#20260,#20261,#20262,#20263,#20264,#20265,#20266,
#20267,#20268,#20269,#20270,#20271,#20272,#20273,#20274,#20275,#20276,#20277,
#20278,#20279,#20280,#20281,#20282,#20283,#20284,#20285,#20286,#20287,#20288,
#20289,#20290,#20291,#20292,#20293,#20294,#20295,#20296,#20297,#20298,#20299,
#20300,#20301,#20302,#20303,#20304,#20305,#20306,#20307,#20308,#20309,#20310,
#20311,#20312,#20313,#20314,#20315,#20316,#20317,#20318,#20319,#20320,#20321,
#20322,#20323,#20324,#20325,#20326,#20327,#20328,#20329,#20330,#20331,#20332,
#20333,#20334,#20335,#20336,#20337,#20338,#20339,#20340,#20341,#20342,#20343,
#20344,#20345,#20346,#20347,#20348,#20349,#20350,#20351,#20352,#20353,#20354,
#20355,#20356,#20357,#20358,#20359,#20360,#20361,#20362,#20363,#20364,#20365,
#20366,#20367,#20368,#20369,#20370,#20371,#20372,#20373,#20374,#20375,#20376,
#20377,#20378,#20379,#20380,#20381,#20382,#20383,#20384,#20385,#20386,#20387,
#20388,#20389,#20390,#20391,#20392,#20393,#20394,#20395,#20396,#20397,#20398,
#20399,#20400,#20401,#20402,#20403,#20404,#20405,#20406,#20407,#20408),
 .UNSPECIFIED.,.F.,.F.,(4,2,2,2,2,2,2,2,2,2,2,2,2,2,2,2,2,2,2,2,2,2,2,2,
2,2,2,2,2,2,2,2,2,2,2,2,2,2,2,2,2,2,2,2,2,2,2,2,2,2,2,2,2,2,2,2,2,2,2,2,
2,2,2,2,2,2,2,2,2,2,2,2,2,2,2,2,2,2,2,2,2,2,2,2,2,2,2,2,2,4),(-3.88535150283469,
-3.88206035453889,-3.87607707548919,-3.87166257690228,-3.86690391205419,
-3.85906272704095,-3.83357894725827,-3.8126953004503,-3.80533831202851,
-3.799868786755,-3.7969956088574,-3.79450114210205,-3.79149892792447,-3.78410652161969,
-3.74710213544244,-3.73001793708437,-3.72384423113077,-3.71940166878453,
-3.71471352987746,-3.70722203056161,-3.66863710155652,-3.65631546398605,
-3.65084729615386,-3.64646290060631,-3.64381421307235,-3.64120384542324,
-3.63700107334225,-3.62025719321828,-3.59230640344088,-3.57696863223177,
-3.57099186417255,-3.56657992282527,-3.56182207196605,-3.55397804374203,
-3.52719836237098,-3.50725743768062,-3.49678493994851,-3.49314572741337,
-3.4906405877451,-3.4878070449491,-3.4825315902463,-3.46189736598215,-3.44288580097196,
-3.42509991143467,-3.41885501071075,-3.41440051324379,-3.40973401626855,
-3.40235319539531,-3.36553066063845,-3.34709456543,-3.34197757082293,-3.33917592150492,
-3.33668712098327,-3.33359093629159,-3.32549151930023,-3.2986392514912,
-3.27555184356393,-3.2678827313774,-3.26315915128797,-3.2587326127178,-3.25266185931445,
-3.23774973729583,-3.23323840101226,-3.20883007852156,-3.19271533485041,
-3.18860248720295,-3.18601043490097,-3.18367043807317,-3.179537537448,-3.16449543019859,
-3.13514329638442,-3.11946714048323,-3.11344962767322,-3.10903138551789,
-3.10428867036823,-3.09652209350788,-3.06579020797141,-3.04160158508689,
-3.03672543278749,-3.03397344902604,-3.03146333981517,-3.02764630109747,
-3.01643596510118,-2.9869759230571,-2.96777260568876,-2.96139797963505,
-2.95692138561248,-2.95229144896243,-2.94509696895192,-2.91390510725203),
 .UNSPECIFIED.);
#224=B_SPLINE_CURVE_WITH_KNOTS('',3,(#20414,#20415,#20416,#20417,#20418,
#20419,#20420,#20421,#20422,#20423,#20424,#20425,#20426,#20427,#20428,#20429,
#20430,#20431,#20432),.UNSPECIFIED.,.F.,.F.,(4,3,3,3,3,3,4),(3.11344365898459E-7,
0.0233011787387913,0.320469476292411,0.5,0.51186353466473,0.820469476292293,
0.999999999999359),.UNSPECIFIED.);
#225=B_SPLINE_CURVE_WITH_KNOTS('',3,(#20435,#20436,#20437,#20438,#20439,
#20440,#20441,#20442,#20443,#20444,#20445,#20446,#20447,#20448,#20449,#20450,
#20451,#20452,#20453,#20454,#20455,#20456,#20457,#20458,#20459,#20460,#20461,
#20462,#20463,#20464,#20465,#20466,#20467,#20468,#20469,#20470,#20471,#20472,
#20473,#20474,#20475,#20476,#20477,#20478,#20479,#20480,#20481,#20482,#20483,
#20484,#20485,#20486,#20487,#20488,#20489,#20490,#20491,#20492,#20493,#20494,
#20495,#20496,#20497,#20498,#20499,#20500,#20501,#20502,#20503,#20504,#20505,
#20506,#20507,#20508,#20509,#20510,#20511,#20512,#20513,#20514,#20515,#20516,
#20517,#20518,#20519,#20520,#20521,#20522,#20523,#20524,#20525,#20526,#20527,
#20528,#20529,#20530,#20531,#20532),.UNSPECIFIED.,.F.,.F.,(4,2,2,2,2,2,
2,2,2,2,2,2,2,2,2,2,2,2,2,2,2,2,2,2,2,2,2,2,2,2,2,2,2,2,2,2,2,2,2,2,2,2,
2,2,2,2,2,2,4),(8.62633731758881E-5,0.00489546330344884,0.0142706318016333,
0.0445460973104298,0.0630467411669007,0.0693037770110129,0.0736989523517897,
0.0782406243222035,0.0852821894467348,0.124802990275626,0.141850628688387,
0.145989670920605,0.148576444505331,0.151175121296076,0.155488466861705,
0.178558908054217,0.202019090751898,0.216034749297213,0.221750471086131,
0.226027220615217,0.230685578642636,0.238453950532035,0.269014666080015,
0.293684353627655,0.298770656815782,0.301546549909239,0.303950704394756,
0.307358580056001,0.316538424984634,0.33249230058845,0.366143481626674,
0.373591277326783,0.378150253498505,0.38239241413236,0.388145658930972,
0.402721932626938,0.427956648573111,0.447476517083816,0.452584570366893,
0.455349803213659,0.457753117029615,0.46114906629338,0.470153889756483,
0.485582082471485,0.520062889397207,0.52737915856892,0.531908116637689,
0.534920387016673,0.537782073242468),.UNSPECIFIED.);
#226=B_SPLINE_CURVE_WITH_KNOTS('',3,(#20538,#20539,#20540,#20541),
 .UNSPECIFIED.,.F.,.F.,(4,4),(0.971382721880866,0.971517849456709),
 .UNSPECIFIED.);
#227=B_SPLINE_CURVE_WITH_KNOTS('',3,(#20543,#20544,#20545,#20546,#20547,
#20548,#20549,#20550,#20551,#20552),.UNSPECIFIED.,.F.,.F.,(4,3,3,4),(0.,
0.0931868878003157,0.613406353066145,0.999999999998996),.UNSPECIFIED.);
#228=B_SPLINE_CURVE_WITH_KNOTS('',3,(#20555,#20556,#20557,#20558,#20559,
#20560,#20561,#20562,#20563,#20564,#20565,#20566,#20567,#20568,#20569,#20570,
#20571,#20572,#20573,#20574,#20575,#20576,#20577,#20578,#20579,#20580,#20581,
#20582,#20583,#20584,#20585,#20586,#20587,#20588,#20589,#20590,#20591,#20592,
#20593,#20594,#20595,#20596,#20597,#20598,#20599,#20600,#20601,#20602,#20603,
#20604,#20605,#20606,#20607,#20608,#20609,#20610,#20611,#20612,#20613,#20614,
#20615,#20616,#20617,#20618,#20619,#20620,#20621,#20622,#20623,#20624,#20625,
#20626,#20627,#20628,#20629,#20630,#20631,#20632,#20633,#20634,#20635,#20636,
#20637,#20638,#20639,#20640,#20641,#20642),.UNSPECIFIED.,.F.,.F.,(4,2,2,
2,2,2,2,2,2,2,2,2,2,2,2,2,2,2,2,2,2,2,2,2,2,2,2,2,2,2,2,2,2,2,2,2,2,2,2,
2,2,2,2,4),(0.000234844493040472,0.00146418424371738,0.00341290155910423,
0.0105235842651047,0.0435947675953836,0.0652403380488386,0.0713326511653109,
0.074496898121553,0.0768442786627634,0.0797918452300767,0.0848443214240282,
0.108994234681365,0.135616401151146,0.143099789849741,0.148157384505868,
0.150240790666415,0.15174083621689,0.153383032157199,0.156222550817788,
0.167533662195587,0.198103239830759,0.219661864304074,0.224625012836271,
0.227533567510446,0.229855712185375,0.232992693500092,0.239052101197498,
0.260684547479627,0.281545102252944,0.300695542025709,0.30380988239119,
0.305520791106776,0.306959059118639,0.308816983437047,0.312803153697811,
0.329751614485091,0.363453134506496,0.376029122449674,0.380247298277758,
0.382972843708573,0.385398498336505,0.38792367207521,0.391442636254487,
0.395910794425901),.UNSPECIFIED.);
#229=B_SPLINE_CURVE_WITH_KNOTS('',3,(#20648,#20649,#20650,#20651),
 .UNSPECIFIED.,.F.,.F.,(4,4),(3.88500542880906,3.88507765274843),
 .UNSPECIFIED.);
#230=B_SPLINE_CURVE_WITH_KNOTS('',3,(#20652,#20653,#20654,#20655,#20656,
#20657,#20658,#20659,#20660,#20661,#20662,#20663,#20664,#20665,#20666,#20667,
#20668,#20669,#20670,#20671,#20672,#20673,#20674,#20675,#20676,#20677,#20678,
#20679,#20680,#20681,#20682,#20683,#20684,#20685,#20686,#20687,#20688,#20689,
#20690,#20691,#20692,#20693,#20694,#20695,#20696,#20697,#20698,#20699,#20700,
#20701,#20702,#20703,#20704,#20705,#20706,#20707,#20708,#20709,#20710,#20711,
#20712,#20713,#20714,#20715,#20716,#20717,#20718,#20719,#20720,#20721,#20722,
#20723,#20724,#20725,#20726,#20727,#20728,#20729,#20730,#20731,#20732,#20733,
#20734,#20735,#20736,#20737,#20738,#20739,#20740,#20741,#20742,#20743,#20744,
#20745,#20746,#20747,#20748,#20749,#20750,#20751,#20752,#20753,#20754,#20755,
#20756,#20757,#20758,#20759,#20760,#20761,#20762,#20763,#20764,#20765,#20766,
#20767,#20768,#20769,#20770,#20771,#20772,#20773,#20774,#20775,#20776,#20777,
#20778,#20779,#20780,#20781,#20782,#20783,#20784,#20785,#20786,#20787,#20788,
#20789,#20790,#20791,#20792,#20793,#20794,#20795,#20796,#20797,#20798,#20799,
#20800,#20801,#20802,#20803,#20804,#20805,#20806,#20807,#20808,#20809,#20810,
#20811,#20812,#20813,#20814,#20815,#20816,#20817,#20818,#20819,#20820,#20821,
#20822,#20823,#20824,#20825,#20826,#20827,#20828,#20829,#20830,#20831,#20832,
#20833,#20834,#20835,#20836,#20837,#20838,#20839,#20840,#20841,#20842,#20843),
 .UNSPECIFIED.,.F.,.F.,(4,2,2,2,2,2,2,2,2,2,2,2,2,2,2,2,2,2,2,2,2,2,2,2,
2,2,2,2,2,2,2,2,2,2,2,2,2,2,2,2,2,2,2,2,2,2,2,2,2,2,2,2,2,2,2,2,2,2,2,2,
2,2,2,2,2,2,2,2,2,2,2,2,2,2,2,2,2,2,2,2,2,2,2,2,2,2,2,2,2,2,2,2,2,2,2,4),
(0.00010723938499698,0.0325187247414615,0.0544725371139445,0.0575983339188545,
0.0592871541663569,0.0607260986265854,0.0625764159723312,0.0666114580245643,
0.0972489748726172,0.118039938923406,0.12618621984718,0.132455473259296,
0.135619249056975,0.138173003785047,0.141108191615718,0.146128011407001,
0.174150022420611,0.194280527218451,0.209426783900504,0.212355910959386,
0.214005042652508,0.21545781729891,0.217386535260743,0.221663145687393,
0.245868482680921,0.278894239275846,0.286186917169818,0.28954662742067,
0.292125179215272,0.294953054612662,0.299590347161342,0.316186033500614,
0.34553556872939,0.362165930058378,0.366122194262503,0.367978103843899,
0.369411413612714,0.371105569223375,0.37420224477463,0.393833070494413,
0.413307470118417,0.437728930353591,0.442639641342819,0.445508952404061,
0.448048188735129,0.451250327337316,0.45779269776308,0.485741215041162,
0.516986055850625,0.520572071624079,0.522376012929019,0.523836159716188,
0.525393711857864,0.527903595431521,0.536715860065318,0.553860138012039,
0.590528931316358,0.596098825485749,0.599429046958941,0.602017534001131,
0.604845373079938,0.609457924076973,0.62757698180739,0.648156752284447,
0.650779948621628,0.672976630071433,0.676122126760828,0.677846444242693,
0.679171577048668,0.681015609814576,0.6847506784207,0.70807317152071,0.743124756883826,
0.748635715824495,0.751966549153858,0.754578867291662,0.757457772803745,
0.762213915144583,0.781977740838373,0.801561242789734,0.824507170834108,
0.828405954858497,0.830497849884236,0.831950627934779,0.833445295207564,
0.835868352091489,0.844813610434875,0.86262868468981,0.900453538272329,
0.906603066920837,0.909641785046459,0.912060551520529,0.914800836309468,
0.919501233589327,0.942373104456299,0.971382721880866),.UNSPECIFIED.);
#231=B_SPLINE_CURVE_WITH_KNOTS('',3,(#20845,#20846,#20847,#20848),
 .UNSPECIFIED.,.F.,.F.,(4,4),(0.395910794425901,0.395980603577569),
 .UNSPECIFIED.);
#232=B_SPLINE_CURVE_WITH_KNOTS('',3,(#20849,#20850,#20851,#20852,#20853,
#20854,#20855,#20856,#20857,#20858,#20859,#20860,#20861,#20862,#20863,#20864,
#20865,#20866,#20867,#20868,#20869,#20870,#20871,#20872,#20873,#20874,#20875,
#20876,#20877,#20878,#20879,#20880,#20881,#20882,#20883,#20884,#20885,#20886,
#20887,#20888,#20889,#20890,#20891,#20892,#20893,#20894,#20895,#20896,#20897,
#20898,#20899,#20900,#20901,#20902,#20903,#20904,#20905,#20906,#20907,#20908,
#20909,#20910,#20911,#20912,#20913,#20914,#20915,#20916,#20917,#20918,#20919,
#20920,#20921,#20922,#20923,#20924,#20925,#20926,#20927,#20928,#20929,#20930,
#20931,#20932,#20933,#20934,#20935,#20936,#20937,#20938,#20939,#20940,#20941,
#20942,#20943,#20944,#20945,#20946,#20947,#20948,#20949,#20950,#20951,#20952,
#20953,#20954,#20955,#20956,#20957,#20958,#20959,#20960,#20961,#20962,#20963,
#20964,#20965,#20966,#20967,#20968,#20969,#20970,#20971,#20972,#20973,#20974,
#20975,#20976,#20977,#20978,#20979,#20980,#20981,#20982,#20983,#20984,#20985,
#20986,#20987,#20988,#20989,#20990,#20991,#20992,#20993,#20994,#20995,#20996,
#20997,#20998,#20999,#21000,#21001,#21002,#21003,#21004,#21005,#21006,#21007,
#21008,#21009,#21010,#21011,#21012,#21013,#21014,#21015,#21016,#21017,#21018,
#21019,#21020,#21021,#21022,#21023,#21024,#21025,#21026,#21027,#21028,#21029,
#21030,#21031,#21032,#21033,#21034,#21035,#21036,#21037,#21038,#21039,#21040),
 .UNSPECIFIED.,.F.,.F.,(4,2,2,2,2,2,2,2,2,2,2,2,2,2,2,2,2,2,2,2,2,2,2,2,
2,2,2,2,2,2,2,2,2,2,2,2,2,2,2,2,2,2,2,2,2,2,2,2,2,2,2,2,2,2,2,2,2,2,2,2,
2,2,2,2,2,2,2,2,2,2,2,2,2,2,2,2,2,2,2,2,2,2,2,2,2,2,2,2,2,2,2,2,2,2,2,4),
(9.9999999796755E-7,0.02519092473315,0.0564025880721698,0.0616559800192072,
0.0637316023650858,0.0651999446191349,0.0668019206662103,0.0694848898638641,
0.0790681216699718,0.106175768478792,0.133394245650913,0.138446429899689,
0.141377475176916,0.143960024998273,0.147202921781375,0.153568097338929,
0.186356224183761,0.205581266730133,0.21191672535024,0.216378598227054,
0.218339147871063,0.21980092101262,0.221473877686754,0.224398440116991,
0.237776146358797,0.262138962502371,0.285564999976058,0.291850582258868,
0.295032065258697,0.297605155500909,0.300568549248421,0.305652693250769,
0.333568857700026,0.365169152721188,0.37060678651047,0.372720564963444,
0.374201757311434,0.37579470633124,0.378441810170241,0.387657508910769,
0.415010559853812,0.442351829245785,0.447395093832823,0.450317863305526,
0.452891051892687,0.456119141701659,0.462658796258345,0.491880569723409,
0.513956596191244,0.520786495528479,0.525501565918187,0.527499328014449,
0.528961232216845,0.530605175812081,0.533480768351148,0.545499219654417,
0.57085035850078,0.594754734797463,0.601100471141146,0.604293562160237,
0.606867200090937,0.609821509125751,0.614866065499073,0.642774862253483,
0.674390605975228,0.679796159409505,0.681906034592995,0.683387469654588,
0.684984439363804,0.687644949509465,0.696985810657996,0.724241673081108,
0.751521510367138,0.756566267650658,0.759491226758494,0.762067194953283,
0.765299977278521,0.771637877409102,0.804989965384699,0.824039851195637,
0.830341354740278,0.834782709217647,0.836734785574818,0.838191394415411,
0.839860934758488,0.842777098139197,0.856042009909667,0.880505979313697,
0.903992705973529,0.910285138291514,0.913466804443258,0.916038436588451,
0.918998346673348,0.924071971441916,0.952345120658601,0.971257865379087),
 .UNSPECIFIED.);
#233=B_SPLINE_CURVE_WITH_KNOTS('',3,(#21045,#21046,#21047,#21048,#21049,
#21050,#21051,#21052,#21053,#21054,#21055,#21056,#21057,#21058,#21059,#21060,
#21061,#21062,#21063,#21064,#21065,#21066,#21067,#21068,#21069,#21070,#21071,
#21072,#21073,#21074,#21075,#21076,#21077,#21078,#21079,#21080,#21081,#21082,
#21083,#21084,#21085,#21086,#21087,#21088,#21089,#21090,#21091,#21092,#21093,
#21094,#21095,#21096,#21097,#21098,#21099,#21100,#21101,#21102,#21103,#21104,
#21105,#21106,#21107,#21108,#21109,#21110,#21111,#21112,#21113,#21114,#21115,
#21116,#21117,#21118,#21119,#21120,#21121,#21122,#21123,#21124,#21125,#21126,
#21127,#21128,#21129,#21130,#21131,#21132,#21133,#21134,#21135,#21136,#21137,
#21138,#21139,#21140,#21141,#21142,#21143,#21144,#21145,#21146,#21147,#21148,
#21149,#21150,#21151,#21152,#21153,#21154,#21155,#21156,#21157,#21158,#21159,
#21160,#21161,#21162,#21163,#21164,#21165,#21166,#21167,#21168,#21169,#21170,
#21171,#21172,#21173,#21174,#21175,#21176,#21177,#21178,#21179,#21180,#21181,
#21182,#21183,#21184,#21185,#21186,#21187,#21188,#21189,#21190,#21191,#21192,
#21193,#21194,#21195,#21196,#21197,#21198,#21199,#21200,#21201,#21202,#21203,
#21204,#21205,#21206,#21207,#21208,#21209,#21210,#21211,#21212,#21213,#21214,
#21215,#21216,#21217,#21218,#21219,#21220,#21221,#21222,#21223,#21224,#21225,
#21226,#21227,#21228,#21229,#21230,#21231,#21232,#21233,#21234,#21235,#21236,
#21237,#21238,#21239,#21240,#21241,#21242,#21243,#21244,#21245,#21246,#21247,
#21248,#21249,#21250),.UNSPECIFIED.,.F.,.F.,(4,2,2,2,2,2,2,2,2,2,2,2,2,
2,2,2,2,2,2,2,2,2,2,2,2,2,2,2,2,2,2,2,2,2,2,2,2,2,2,2,2,2,2,2,2,2,2,2,2,
2,2,2,2,2,2,2,2,2,2,2,2,2,2,2,2,2,2,2,2,2,2,2,2,2,2,2,2,2,2,2,2,2,2,2,2,
2,2,2,2,2,2,2,2,2,2,2,2,2,2,2,2,2,4),(2.91363847548873,2.92846992430067,
2.9350037570659,2.93822435847139,2.9407892795551,2.94370003308178,2.94871529797709,
2.97539590091814,3.00163345244596,3.01244030335717,3.01522552220558,3.01684535898034,
3.01830721705526,3.0203326637322,3.02523830887129,3.0324500724466,3.05703095222732,
3.08310147634826,3.0896067236805,3.09282193493012,3.09538651111843,3.09830111136425,
3.10333388046192,3.13064857064572,3.15794469573232,3.16727920182255,3.16993216976661,
3.1715230771442,3.17299676052353,3.17509224043723,3.18044210440504,3.21188177216223,
3.24014375118115,3.24514046985061,3.24807586495119,3.25063824712196,3.25382388106003,
3.26017575008762,3.28422343262169,3.30985634038819,3.32152127499904,3.32436726635071,
3.32600045416016,3.32745808321209,3.32945562095726,3.33419227433353,3.3410696018987,
3.36347202072606,3.39225530415368,3.39878904836501,3.40200957470853,3.40457441166448,
3.40748503655207,3.41249997330323,3.43916916861822,3.46538510161361,3.47622728940209,
3.47901516489793,3.4806355529561,3.48209722001825,3.48412136315025,3.48901874827911,
3.49621381119142,3.52067755869478,3.5492957521086,3.55432286424874,3.55726513610132,
3.55982690613964,3.56300319099291,3.56930697945768,3.59296538608811,3.61778457682974,
3.63059294607692,3.63347815776497,3.63513682593029,3.6365890294428,3.63854103762135,
3.64300479014127,3.64935395955308,3.66869093849567,3.70156201422261,3.70793168799658,
3.71116385984767,3.71373107656037,3.71663708756684,3.72162556090924,3.74736062303953,
3.77185899830765,3.78512965865827,3.7880391861883,3.78970331034777,3.79100705499865,
3.79285973693038,3.79678624329087,3.81312212407598,3.84374498333481,3.85947673479073,
3.86404209704228,3.8668545262212,3.86932980156745,3.87183462723816,3.87508034379017,
3.88500542880906),.UNSPECIFIED.);
#234=B_SPLINE_CURVE_WITH_KNOTS('',3,(#21251,#21252,#21253,#21254,#21255,
#21256,#21257,#21258,#21259,#21260,#21261,#21262,#21263,#21264,#21265,#21266,
#21267,#21268,#21269,#21270,#21271,#21272,#21273,#21274,#21275,#21276,#21277,
#21278,#21279,#21280,#21281,#21282,#21283,#21284,#21285,#21286,#21287,#21288,
#21289,#21290,#21291,#21292,#21293,#21294,#21295,#21296,#21297,#21298,#21299,
#21300,#21301,#21302,#21303,#21304,#21305,#21306,#21307,#21308,#21309,#21310,
#21311,#21312,#21313,#21314,#21315,#21316,#21317,#21318,#21319,#21320,#21321,
#21322,#21323,#21324,#21325,#21326,#21327,#21328,#21329,#21330,#21331,#21332,
#21333,#21334,#21335,#21336,#21337,#21338,#21339,#21340,#21341,#21342,#21343,
#21344,#21345,#21346,#21347,#21348,#21349,#21350,#21351,#21352,#21353,#21354,
#21355,#21356,#21357,#21358,#21359,#21360,#21361,#21362,#21363,#21364,#21365,
#21366,#21367,#21368,#21369,#21370,#21371,#21372,#21373,#21374,#21375,#21376,
#21377,#21378,#21379,#21380,#21381,#21382,#21383,#21384,#21385,#21386,#21387,
#21388,#21389,#21390,#21391,#21392,#21393,#21394,#21395,#21396,#21397,#21398,
#21399,#21400,#21401,#21402,#21403,#21404,#21405,#21406,#21407,#21408,#21409,
#21410,#21411,#21412,#21413,#21414,#21415,#21416,#21417,#21418,#21419,#21420,
#21421,#21422,#21423,#21424,#21425,#21426,#21427,#21428,#21429,#21430,#21431,
#21432,#21433,#21434,#21435,#21436,#21437,#21438,#21439,#21440,#21441,#21442,
#21443,#21444,#21445,#21446,#21447,#21448,#21449,#21450,#21451,#21452,#21453,
#21454,#21455,#21456,#21457,#21458,#21459,#21460,#21461,#21462),
 .UNSPECIFIED.,.F.,.F.,(4,2,2,2,2,2,2,2,2,2,2,2,2,2,2,2,2,2,2,2,2,2,2,2,
2,2,2,2,2,2,2,2,2,2,2,2,2,2,2,2,2,2,2,2,2,2,2,2,2,2,2,2,2,2,2,2,2,2,2,2,
2,2,2,2,2,2,2,2,2,2,2,2,2,2,2,2,2,2,2,2,2,2,2,2,2,2,2,2,2,2,2,2,2,2,2,2,
2,2,2,2,2,2,2,2,2,4),(0.971257865379087,0.976325255804158,0.983962143761288,
0.989081685200867,0.991146399765066,0.99261935824194,0.994233295168095,
0.996971799670707,1.00719264491218,1.03382143376433,1.06072456082819,1.06575934219924,
1.06868220348836,1.07125851377223,1.07449464533364,1.08084868505782,1.11382997239657,
1.13312526446993,1.13947228778614,1.14393769368611,1.14589414297634,1.14735147273487,
1.14901894796997,1.15192538747999,1.16499881532324,1.18959666054105,1.21314384227968,
1.21944408532782,1.22262751146473,1.2251995459957,1.22815880142242,1.23322854545502,
1.26117681299847,1.28541740127014,1.29309564335376,1.29823548258234,1.30030352534595,
1.30177710840145,1.30338965782822,1.30612209305398,1.31627369360075,1.34295132762344,
1.36988319406742,1.3749184436539,1.37784123349403,1.38041727164373,1.38365277619851,
1.39022157974486,1.41718262529436,1.43761462950057,1.4467480392036,1.45257091166774,
1.45474111922433,1.45623301281079,1.45780793621372,1.46036929416519,1.46871670971107,
1.49670760690703,1.52442176842347,1.52947730490398,1.53240441272288,1.53497984635921,
1.53820873780349,1.54474325694021,1.57440412199197,1.59611513982899,1.60288557410263,
1.60757094423572,1.60956493398379,1.61102707837854,1.6126738835161,1.61556337358936,
1.62773580619324,1.65296815940903,1.67681172019271,1.68314856102598,1.68633903496989,
1.68891140214184,1.69186514390001,1.69691082539189,1.72637566256953,1.75012648343322,
1.75722108995571,1.76207137141689,1.7640927858228,1.76555890720528,1.76719213379559,
1.77001927648233,1.78130188580457,1.80716753299769,1.83132094388323,1.8376958511454,
1.84089374947813,1.84344303646357,1.84638287376466,1.85136668970763,1.8749379239436,
1.90357094345627,1.91133048358001,1.91650982504854,1.91858400109638,1.92005855538232,
1.92166844916331,1.92438899032147,1.93440366827172,1.94248326667345),
 .UNSPECIFIED.);
#235=B_SPLINE_CURVE_WITH_KNOTS('',3,(#21467,#21468,#21469,#21470,#21471,
#21472,#21473,#21474,#21475,#21476,#21477,#21478,#21479,#21480,#21481,#21482,
#21483,#21484,#21485,#21486,#21487,#21488,#21489,#21490,#21491,#21492,#21493,
#21494,#21495,#21496,#21497,#21498,#21499,#21500,#21501,#21502,#21503,#21504,
#21505,#21506,#21507,#21508,#21509,#21510,#21511,#21512,#21513,#21514,#21515,
#21516,#21517,#21518,#21519,#21520,#21521,#21522,#21523,#21524,#21525,#21526,
#21527,#21528,#21529,#21530,#21531,#21532,#21533,#21534,#21535,#21536,#21537,
#21538,#21539,#21540,#21541,#21542,#21543,#21544,#21545,#21546,#21547,#21548,
#21549,#21550,#21551,#21552,#21553,#21554,#21555,#21556,#21557,#21558,#21559,
#21560,#21561,#21562,#21563,#21564,#21565,#21566,#21567,#21568,#21569,#21570,
#21571,#21572,#21573,#21574,#21575,#21576,#21577,#21578,#21579,#21580,#21581,
#21582,#21583,#21584,#21585,#21586,#21587,#21588,#21589,#21590,#21591,#21592,
#21593,#21594,#21595,#21596,#21597,#21598,#21599,#21600,#21601,#21602,#21603,
#21604,#21605,#21606,#21607,#21608,#21609,#21610,#21611,#21612,#21613,#21614,
#21615,#21616,#21617,#21618,#21619,#21620,#21621,#21622,#21623,#21624,#21625,
#21626,#21627,#21628,#21629,#21630,#21631,#21632,#21633,#21634,#21635,#21636,
#21637,#21638,#21639,#21640,#21641,#21642,#21643,#21644,#21645,#21646,#21647,
#21648,#21649,#21650,#21651,#21652,#21653,#21654,#21655,#21656,#21657,#21658,
#21659,#21660,#21661,#21662),.UNSPECIFIED.,.F.,.F.,(4,2,2,2,2,2,2,2,2,2,
2,2,2,2,2,2,2,2,2,2,2,2,2,2,2,2,2,2,2,2,2,2,2,2,2,2,2,2,2,2,2,2,2,2,2,2,
2,2,2,2,2,2,2,2,2,2,2,2,2,2,2,2,2,2,2,2,2,2,2,2,2,2,2,2,2,2,2,2,2,2,2,2,
2,2,2,2,2,2,2,2,2,2,2,2,2,2,2,4),(1.94237495036772,1.94253659913532,1.96409512683097,
2.00185039429317,2.0072586395656,2.01057432072849,2.01314890224053,2.01600255190526,
2.02075328911474,2.04114311351225,2.07026986901385,2.08457089645924,2.0875358103584,
2.089212075023,2.09051427689846,2.09234999246578,2.09618267534226,2.11170077327053,
2.1463471246293,2.15949757954353,2.16380268412224,2.16656053774036,2.16916704368215,
2.17270340883202,2.18101782407163,2.21205172661935,2.23707904544012,2.24138069583305,
2.24328263050384,2.24473185985878,2.24639852132983,2.24940039746432,2.26626634298567,
2.30086647801091,2.31406497738209,2.31837520819215,2.32113413029699,2.32374008464055,
2.32727325957176,2.33556834130142,2.36658614775378,2.37409716642295,2.39346041401075,
2.39657274435135,2.3982819605469,2.39972478476211,2.40159520321101,2.40561167478547,
2.42274234098753,2.45259378397755,2.46808790924334,2.47266585788397,2.47548226344961,
2.47806656224483,2.48145729271481,2.48891506478013,2.52223743771716,2.54620570782123,
2.55051754289015,2.55242128098498,2.55387074274075,2.55553632041342,2.55853310653489,
2.57525885906144,2.60941671689506,2.62309673387811,2.62746093204471,2.63023140313683,
2.63283224823109,2.63633371488541,2.64443661403982,2.65588413690852,2.68792724786295,
2.70280799359832,2.7058031157615,2.70748619407393,2.70878744058801,2.71061374550297,
2.71439734538039,2.71950183861378,2.73292586816594,2.76378702805817,2.77762347194152,
2.78200417146369,2.78477825376355,2.7873777403833,2.79087008666148,2.79891783028213,
2.81025920809249,2.85435907783433,2.85927960557419,2.86137154585917,2.8628299232549,
2.86441724114062,2.86705430920708,2.87730208617024,2.89973667215865,2.91363847548873),
 .UNSPECIFIED.);
#236=B_SPLINE_CURVE_WITH_KNOTS('',3,(#21663,#21664,#21665,#21666,#21667,
#21668,#21669,#21670,#21671,#21672,#21673,#21674,#21675,#21676,#21677,#21678,
#21679,#21680,#21681,#21682,#21683,#21684,#21685,#21686,#21687,#21688,#21689,
#21690,#21691,#21692,#21693,#21694,#21695,#21696,#21697,#21698,#21699,#21700,
#21701,#21702,#21703,#21704,#21705,#21706,#21707,#21708,#21709,#21710,#21711,
#21712,#21713,#21714,#21715,#21716,#21717,#21718,#21719,#21720,#21721,#21722,
#21723,#21724,#21725,#21726,#21727,#21728,#21729,#21730,#21731,#21732,#21733,
#21734,#21735,#21736,#21737,#21738,#21739,#21740,#21741,#21742,#21743,#21744,
#21745,#21746,#21747,#21748,#21749,#21750,#21751,#21752,#21753,#21754,#21755,
#21756,#21757,#21758,#21759,#21760,#21761,#21762,#21763,#21764,#21765,#21766,
#21767,#21768,#21769,#21770,#21771,#21772,#21773,#21774,#21775,#21776,#21777,
#21778,#21779,#21780,#21781,#21782,#21783,#21784,#21785,#21786,#21787,#21788,
#21789,#21790,#21791,#21792,#21793,#21794,#21795,#21796,#21797,#21798,#21799,
#21800,#21801,#21802,#21803,#21804,#21805,#21806,#21807,#21808,#21809,#21810,
#21811,#21812,#21813,#21814,#21815,#21816,#21817,#21818,#21819,#21820,#21821,
#21822,#21823,#21824,#21825,#21826,#21827,#21828,#21829,#21830,#21831,#21832,
#21833,#21834,#21835,#21836,#21837,#21838,#21839,#21840,#21841,#21842,#21843,
#21844,#21845,#21846,#21847,#21848,#21849,#21850,#21851,#21852,#21853,#21854),
 .UNSPECIFIED.,.F.,.F.,(4,2,2,2,2,2,2,2,2,2,2,2,2,2,2,2,2,2,2,2,2,2,2,2,
2,2,2,2,2,2,2,2,2,2,2,2,2,2,2,2,2,2,2,2,2,2,2,2,2,2,2,2,2,2,2,2,2,2,2,2,
2,2,2,2,2,2,2,2,2,2,2,2,2,2,2,2,2,2,2,2,2,2,2,2,2,2,2,2,2,2,2,2,2,2,2,4),
(1.94248326667345,1.96117665740519,1.98816504256082,1.99320162058116,1.99612460892992,
1.99870048343877,2.00193533306056,2.00850120578587,2.03655542175966,2.06771854393334,
2.07164915893847,2.0735082861722,2.07481795786207,2.07649179774937,2.07942661952704,
2.09305774849087,2.12273754222689,2.14324551837807,2.14801575984335,2.1508815844196,
2.15346768045551,2.15679921380833,2.16223641388999,2.19981682681802,2.22354290357223,
2.22671240585986,2.22841923764114,2.22986984164467,2.23173234044536,2.23578707225683,
2.26622254667201,2.2933523159578,2.3008638056891,2.30427292507808,2.30686922497771,
2.3096969583169,2.31428990536329,2.32981317854939,2.35920713380074,2.37670650875656,
2.38077052850205,2.38265470246385,2.38410446174985,2.38581823259845,2.3889308611405,
2.40784497213815,2.42811084607846,2.45191551434548,2.45690495479881,2.45984622762602,
2.46239562403442,2.46559218242204,2.47195923437794,2.49604705419999,2.52177327221965,
2.53328053947546,2.53612345368896,2.53776022181072,2.53922544786543,2.54124004219528,
2.54604822331266,2.55305860625372,2.5762630771683,2.60389479596131,2.61049225390588,
2.61373341419378,2.6163101613531,2.61922970599601,2.62424902270143,2.65060109391575,
2.67627533764175,2.6878578450532,2.69070588165652,2.69234379956564,2.69380874096683,
2.69582114787963,2.70061587377952,2.70759963272315,2.73063282106473,2.75851724987628,
2.76509364286982,2.76833083185051,2.77090729639272,2.77382959338312,2.77886148434049,
2.80564165610537,2.83205906085926,2.84259257456498,2.84536381605995,2.84698499897824,
2.84845557525342,2.85050428204258,2.85552140797899,2.86294891921168,2.8890095558369,
2.91380463577067),.UNSPECIFIED.);
#237=B_SPLINE_CURVE_WITH_KNOTS('',3,(#21859,#21860,#21861,#21862,#21863,
#21864,#21865,#21866,#21867,#21868,#21869,#21870,#21871,#21872,#21873,#21874,
#21875,#21876,#21877,#21878,#21879,#21880,#21881,#21882,#21883,#21884,#21885,
#21886,#21887,#21888,#21889,#21890,#21891,#21892,#21893,#21894,#21895,#21896,
#21897,#21898,#21899,#21900,#21901,#21902,#21903,#21904,#21905,#21906,#21907,
#21908,#21909,#21910,#21911,#21912,#21913,#21914,#21915,#21916,#21917,#21918,
#21919,#21920,#21921,#21922,#21923,#21924,#21925,#21926,#21927,#21928,#21929,
#21930,#21931,#21932,#21933,#21934,#21935,#21936,#21937,#21938,#21939,#21940,
#21941,#21942,#21943,#21944,#21945,#21946,#21947,#21948,#21949,#21950,#21951,
#21952,#21953,#21954,#21955,#21956,#21957,#21958,#21959,#21960,#21961,#21962,
#21963,#21964,#21965,#21966,#21967,#21968,#21969,#21970,#21971,#21972,#21973,
#21974,#21975,#21976,#21977,#21978,#21979,#21980,#21981,#21982,#21983,#21984,
#21985,#21986,#21987,#21988,#21989,#21990,#21991,#21992,#21993,#21994,#21995,
#21996,#21997,#21998,#21999,#22000,#22001,#22002,#22003,#22004,#22005,#22006,
#22007,#22008,#22009,#22010,#22011,#22012,#22013,#22014,#22015,#22016,#22017,
#22018,#22019,#22020,#22021,#22022,#22023,#22024,#22025,#22026,#22027,#22028,
#22029,#22030,#22031,#22032,#22033,#22034,#22035,#22036,#22037,#22038,#22039,
#22040,#22041,#22042,#22043,#22044,#22045,#22046,#22047,#22048,#22049,#22050,
#22051,#22052,#22053,#22054,#22055,#22056,#22057,#22058,#22059,#22060,#22061,
#22062,#22063,#22064,#22065,#22066,#22067,#22068),.UNSPECIFIED.,.F.,.F.,
(4,2,2,2,2,2,2,2,2,2,2,2,2,2,2,2,2,2,2,2,2,2,2,2,2,2,2,2,2,2,2,2,2,2,2,
2,2,2,2,2,2,2,2,2,2,2,2,2,2,2,2,2,2,2,2,2,2,2,2,2,2,2,2,2,2,2,2,2,2,2,2,
2,2,2,2,2,2,2,2,2,2,2,2,2,2,2,2,2,2,2,2,2,2,2,2,2,2,2,2,2,2,2,2,2,4),(0.971210180410019,
0.975261496742874,0.994106600701588,1.00036348073205,1.00477761980553,1.00671997089861,
1.00817010981954,1.00983255736165,1.01273618767421,1.0259100314029,1.0504498676663,
1.07397609471919,1.08026287570202,1.08343533175024,1.08599624542203,1.08893999017788,
1.09397570919052,1.12202624026933,1.14693303345406,1.15419233059721,1.15912123074284,
1.16115031821869,1.16261261461269,1.16423052028552,1.16700740171044,1.17770986578371,
1.20400122857697,1.23070963420215,1.23572486237741,1.23863541531787,1.24120005999134,
1.24442018203644,1.25073707171717,1.28428643785143,1.30321538549088,1.30948801878196,
1.31391047558128,1.31585427836146,1.31730458836495,1.31896618149448,1.32186606227585,
1.3349682287126,1.35955862079213,1.38310789328704,1.38939753379382,1.39257054218465,
1.39513148348492,1.39807479955747,1.40310864322361,1.4307536621768,1.4559890974859,
1.46329538543929,1.46824769886415,1.47028056604288,1.47174345287426,1.47335964406156,
1.47612871113095,1.48673168299265,1.51309345768745,1.53984307456524,1.54485944724831,
1.5477702359569,1.55033483416101,1.55355455965989,1.56008489558888,1.58923968240741,
1.61136492567873,1.61819731087374,1.6229105589393,1.6249041105827,1.62636102715067,
1.62799578613998,1.63085002457584,1.64265032168548,1.66816463731992,1.69443121625562,
1.69943344183427,1.70234117507355,1.70490614626822,1.70813042531729,1.71446771173402,
1.7476058422646,1.76681768522387,1.77314302695158,1.7775932495274,1.77954187616466,
1.78099275340665,1.78265151394907,1.78553900513351,1.79840826385534,1.8231625868599,
1.84678694267006,1.85308585862446,1.85626064287922,1.85882165581355,1.86176355651798,
1.86679126908261,1.89487302921753,1.9151291232248,1.93011630653898,1.93304191434742,
1.93469215616608,1.93614501112256,1.9380747945384,1.94237495036772),
 .UNSPECIFIED.);
#238=B_SPLINE_CURVE_WITH_KNOTS('',3,(#22069,#22070,#22071,#22072,#22073,
#22074,#22075,#22076,#22077,#22078,#22079,#22080,#22081,#22082,#22083,#22084,
#22085,#22086,#22087,#22088,#22089,#22090,#22091,#22092,#22093,#22094,#22095,
#22096,#22097,#22098,#22099,#22100,#22101,#22102,#22103,#22104,#22105,#22106,
#22107,#22108,#22109,#22110,#22111,#22112,#22113,#22114,#22115,#22116,#22117,
#22118,#22119,#22120,#22121,#22122,#22123,#22124,#22125,#22126,#22127,#22128,
#22129,#22130,#22131,#22132,#22133,#22134,#22135,#22136,#22137,#22138,#22139,
#22140,#22141,#22142,#22143,#22144,#22145,#22146,#22147,#22148,#22149,#22150,
#22151,#22152,#22153,#22154,#22155,#22156,#22157,#22158,#22159,#22160,#22161,
#22162,#22163,#22164,#22165,#22166,#22167,#22168,#22169,#22170,#22171,#22172,
#22173,#22174,#22175,#22176,#22177,#22178,#22179,#22180,#22181,#22182,#22183,
#22184,#22185,#22186,#22187,#22188,#22189,#22190,#22191,#22192,#22193,#22194,
#22195,#22196,#22197,#22198,#22199,#22200,#22201,#22202,#22203,#22204,#22205,
#22206,#22207,#22208,#22209,#22210,#22211,#22212,#22213,#22214,#22215,#22216,
#22217,#22218,#22219,#22220,#22221,#22222,#22223,#22224,#22225,#22226,#22227,
#22228,#22229,#22230,#22231,#22232,#22233,#22234,#22235,#22236,#22237,#22238,
#22239,#22240,#22241,#22242,#22243,#22244,#22245,#22246,#22247,#22248,#22249,
#22250,#22251,#22252,#22253,#22254,#22255,#22256,#22257,#22258,#22259,#22260,
#22261,#22262,#22263,#22264,#22265,#22266,#22267,#22268,#22269,#22270,#22271,
#22272,#22273,#22274,#22275,#22276),.UNSPECIFIED.,.F.,.F.,(4,2,2,2,2,2,
2,2,2,2,2,2,2,2,2,2,2,2,2,2,2,2,2,2,2,2,2,2,2,2,2,2,2,2,2,2,2,2,2,2,2,2,
2,2,2,2,2,2,2,2,2,2,2,2,2,2,2,2,2,2,2,2,2,2,2,2,2,2,2,2,2,2,2,2,2,2,2,2,
2,2,2,2,2,2,2,2,2,2,2,2,2,2,2,2,2,2,2,2,2,2,2,2,2,4),(2.91380463577067,
2.91558023577488,2.92062618130808,2.92358031518007,2.92615316906034,2.92934443437629,
2.93568344900227,2.95954075360705,2.98479097068585,2.99696999021269,2.99986041191154,
3.00150760920297,3.00296999809474,3.00496417752987,3.00964942673475,3.01641857102645,
3.03812103479389,3.06777817344399,3.07431287501553,3.07754216346911,3.08011806219389,
3.08304585813898,3.08810297454847,3.11583112608264,3.14383779454734,3.15219383664496,
3.15475651621168,3.15633193330948,3.15782406349889,3.15999422601928,3.16581474348366,
3.17494123920076,3.19534119474881,3.2247871699429,3.22983373040736,3.23278812485231,
3.23536114588621,3.23855254101388,3.24489154816366,3.26874694409867,3.2939915060906,
3.30618175967733,3.30907300811698,3.31072045347557,3.31218290329949,3.31417694970153,
3.31886092905509,3.32562744274242,3.34731280902575,3.37699643245793,3.38353122196624,
3.38676065989535,3.38933672597844,3.39226476385495,3.39732243112552,3.42506105053049,
3.45308458564713,3.46142151175627,3.46398219524387,3.46555724141491,3.46704975444102,
3.4692215408972,3.47505284053578,3.48420296014097,3.50471598674893,3.53160979281116,
3.53814656226339,3.54137648854507,3.54395272173579,3.54688071057921,3.55193767871528,
3.57963815438586,3.60759427639966,3.61602233692538,3.61859310767078,3.62017042739307,
3.62166173713894,3.62382690372044,3.62961127745315,3.63865749737499,3.65867039064899,
3.68862288924594,3.6936796302642,3.69663652616528,3.69920964962001,3.70239848356632,
3.70872322063626,3.73246006604158,3.75745128468574,3.77001147430507,3.77288766811954,
3.77454856513064,3.77600784250254,3.77797724530373,3.7825158637303,3.78900141758038,
3.80905589589399,3.8409627958709,3.84736024583427,3.85060579078563,3.85318354678195,
3.8561015952899,3.86111163008662,3.8852916424057),.UNSPECIFIED.);
#239=B_SPLINE_CURVE_WITH_KNOTS('',3,(#22282,#22283,#22284,#22285),
 .UNSPECIFIED.,.F.,.F.,(4,4),(4.85639440324075,4.85640163643273),
 .UNSPECIFIED.);
#240=B_SPLINE_CURVE_WITH_KNOTS('',3,(#22286,#22287,#22288,#22289,#22290,
#22291,#22292,#22293,#22294,#22295,#22296,#22297,#22298,#22299,#22300,#22301,
#22302,#22303,#22304,#22305,#22306,#22307,#22308,#22309,#22310,#22311,#22312,
#22313,#22314,#22315,#22316,#22317,#22318,#22319,#22320,#22321,#22322,#22323,
#22324,#22325,#22326,#22327,#22328,#22329,#22330,#22331,#22332,#22333,#22334,
#22335,#22336,#22337,#22338,#22339,#22340,#22341,#22342,#22343,#22344,#22345,
#22346,#22347,#22348,#22349,#22350,#22351,#22352,#22353,#22354,#22355,#22356,
#22357,#22358,#22359,#22360,#22361,#22362,#22363,#22364,#22365,#22366,#22367,
#22368,#22369,#22370,#22371,#22372,#22373,#22374,#22375,#22376,#22377,#22378,
#22379,#22380,#22381,#22382,#22383,#22384,#22385,#22386,#22387,#22388,#22389,
#22390,#22391,#22392,#22393,#22394,#22395,#22396,#22397,#22398,#22399,#22400,
#22401,#22402,#22403,#22404,#22405,#22406,#22407,#22408,#22409,#22410,#22411,
#22412,#22413,#22414,#22415,#22416,#22417,#22418,#22419,#22420,#22421,#22422,
#22423,#22424,#22425,#22426,#22427,#22428,#22429,#22430,#22431,#22432,#22433,
#22434,#22435,#22436,#22437,#22438,#22439,#22440,#22441,#22442,#22443,#22444,
#22445,#22446,#22447,#22448,#22449,#22450,#22451,#22452,#22453,#22454,#22455,
#22456,#22457,#22458,#22459,#22460,#22461,#22462,#22463,#22464,#22465,#22466,
#22467,#22468,#22469,#22470,#22471,#22472,#22473,#22474,#22475,#22476,#22477,
#22478,#22479,#22480,#22481,#22482,#22483,#22484,#22485,#22486,#22487,#22488,
#22489,#22490,#22491),.UNSPECIFIED.,.F.,.F.,(4,2,2,2,2,2,2,2,2,2,2,2,2,
2,2,2,2,2,2,2,2,2,2,2,2,2,2,2,2,2,2,2,2,2,2,2,2,2,2,2,2,2,2,2,2,2,2,2,2,
2,2,2,2,2,2,2,2,2,2,2,2,2,2,2,2,2,2,2,2,2,2,2,2,2,2,2,2,2,2,2,2,2,2,2,2,
2,2,2,2,2,2,2,2,2,2,2,2,2,2,2,2,2,4),(1.00000000494344E-6,0.00175834446107242,
0.00351802001987414,0.00623450174180225,0.0104376497705416,0.0234537311842529,
0.033898526851978,0.0645977440181031,0.0720635796929351,0.0770950285300956,
0.0791406606262912,0.0806056574754419,0.0822163658602987,0.0849601410301629,
0.0953115684528038,0.121859723686488,0.148720086995578,0.153739794934463,
0.156651398638247,0.159216050547573,0.162434960064653,0.168960487834963,
0.195674234885171,0.219731334588504,0.226865921249746,0.231732405192923,
0.233751370289202,0.235212128255905,0.236834755579364,0.239633104491153,
0.250618548081526,0.27671048144492,0.30330343132107,0.308315483056487,0.311225410308613,
0.3137902267606,0.317011527069953,0.323549707391378,0.350329584820988,0.374317103293988,
0.381441183857816,0.38630236009672,0.388320431739015,0.389781028990109,
0.391404020031621,0.394204129618682,0.40521408987298,0.431287981028016,
0.457870299532301,0.46288195733698,0.465791762509731,0.468356534692227,
0.471577863725021,0.47790053528438,0.511340996447652,0.530345024962821,
0.536631749548814,0.54106165361766,0.543006768903625,0.544457249350533,
0.546118107239259,0.549014709269728,0.562054105165321,0.586689174060207,
0.612485916210867,0.61747369057303,0.620378390903898,0.622943889064307,
0.626173110657204,0.632534154233901,0.665129884854871,0.684723479931867,
0.69111909137914,0.695606264981013,0.697561349841379,0.699013076849338,
0.700668273634879,0.703539939567172,0.716118155241525,0.741079167566029,
0.764799965387285,0.771110959475979,0.774288168938421,0.776849423654191,
0.779789718702168,0.784810029171743,0.811053635071867,0.837445112522644,
0.844911333075698,0.849942907812285,0.851988500992957,0.853453437771141,
0.855064044559905,0.857807574679856,0.868157479231774,0.894705142478403,
0.921564687368944,0.926584169790405,0.929495638051399,0.932060167909693,
0.935278920587192,0.941589134389271,0.971210180410019),.UNSPECIFIED.);
#241=B_SPLINE_CURVE_WITH_KNOTS('',3,(#22493,#22494,#22495,#22496,#22497,
#22498,#22499,#22500,#22501,#22502,#22503,#22504,#22505,#22506,#22507,#22508,
#22509,#22510,#22511,#22512,#22513,#22514,#22515,#22516,#22517,#22518,#22519,
#22520,#22521,#22522,#22523,#22524,#22525,#22526,#22527,#22528,#22529,#22530,
#22531,#22532,#22533,#22534,#22535,#22536,#22537,#22538,#22539,#22540,#22541,
#22542,#22543,#22544,#22545,#22546,#22547,#22548,#22549,#22550,#22551,#22552,
#22553,#22554,#22555,#22556,#22557,#22558,#22559,#22560,#22561,#22562,#22563,
#22564,#22565,#22566,#22567,#22568,#22569,#22570,#22571,#22572,#22573,#22574,
#22575,#22576,#22577,#22578,#22579,#22580,#22581,#22582,#22583,#22584,#22585,
#22586,#22587,#22588,#22589,#22590,#22591,#22592,#22593,#22594,#22595,#22596,
#22597,#22598,#22599,#22600,#22601,#22602,#22603,#22604,#22605,#22606,#22607,
#22608,#22609,#22610,#22611,#22612,#22613,#22614,#22615,#22616,#22617,#22618,
#22619,#22620,#22621,#22622,#22623,#22624,#22625,#22626,#22627,#22628,#22629,
#22630,#22631,#22632,#22633,#22634,#22635,#22636,#22637,#22638,#22639,#22640,
#22641,#22642,#22643,#22644,#22645,#22646,#22647,#22648,#22649,#22650,#22651,
#22652,#22653,#22654,#22655,#22656,#22657,#22658,#22659,#22660,#22661,#22662,
#22663,#22664,#22665,#22666,#22667,#22668,#22669,#22670,#22671,#22672,#22673,
#22674,#22675,#22676,#22677,#22678,#22679,#22680,#22681,#22682,#22683,#22684,
#22685,#22686,#22687,#22688,#22689,#22690,#22691,#22692,#22693,#22694,#22695,
#22696),.UNSPECIFIED.,.F.,.F.,(4,2,2,2,2,2,2,2,2,2,2,2,2,2,2,2,2,2,2,2,
2,2,2,2,2,2,2,2,2,2,2,2,2,2,2,2,2,2,2,2,2,2,2,2,2,2,2,2,2,2,2,2,2,2,2,2,
2,2,2,2,2,2,2,2,2,2,2,2,2,2,2,2,2,2,2,2,2,2,2,2,2,2,2,2,2,2,2,2,2,2,2,2,
2,2,2,2,2,2,2,2,2,4),(3.8852916424057,3.88712357187435,3.91216947743994,
3.9246531922623,3.92752492741152,3.92918482502709,3.93064436526573,3.93261565580514,
3.93716512981121,3.94367145555473,3.96384219122548,3.99558822905864,4.00199128771823,
4.00523801162481,4.00781591189297,4.01073328057202,4.01574000778422,4.04164490123671,
4.06648872724025,4.07925380133357,4.08214462365852,4.0838088761948,4.08526743828527,
4.08723096949413,4.09173541682024,4.09815558014516,4.11784667598959,4.15026463169926,
4.15664360145686,4.15988541073684,4.16246288824127,4.16538348918838,4.17040520475659,
4.19679595052899,4.222532884249,4.23404070996666,4.23688433896004,4.23852159625695,
4.2399873173006,4.24200266999815,4.24681301802354,4.25382686470911,4.27704643474919,
4.30467621364325,4.31127680073499,4.31451920909085,4.31709681847175,4.32001720133888,
4.32503760590402,4.35137965262185,4.37702892191618,4.38866251591199,4.39151463310466,
4.39315377350226,4.39461898862488,4.3966306520774,4.40141849033875,4.40838787240894,
4.4313225042054,4.45936782852854,4.46593563184901,4.46917181948658,4.47174894438843,
4.47467355033144,4.47971340721548,4.50673000075536,4.53353739410063,4.54354954777129,
4.54627087031369,4.54788144324439,4.54935680320084,4.55143235107923,4.55661641116771,
4.5643834559937,4.59306964624377,4.61658370856067,4.62156784010452,4.62450869290741,
4.62705936322379,4.63025965359842,4.63664157293854,4.6608390061161,4.68671506922212,
4.69799859720205,4.7008269822907,4.70246101537498,4.70392793678638,4.70595054604866,
4.71080417987074,4.71790343977355,4.7416770470004,4.77112603927686,4.77616935104553,
4.77912353385828,4.78169738759916,4.78489113496757,4.79123933425002,4.81516140348468,
4.85043472705162,4.85462041813607,4.85590572853124,4.85697161330123),
 .UNSPECIFIED.);
#242=B_SPLINE_CURVE_WITH_KNOTS('',3,(#22697,#22698,#22699,#22700),
 .UNSPECIFIED.,.F.,.F.,(4,4),(9.99999999028984E-7,8.68074318044454E-6),
 .UNSPECIFIED.);
#243=B_SPLINE_CURVE_WITH_KNOTS('',3,(#22705,#22706,#22707,#22708,#22709,
#22710,#22711,#22712,#22713,#22714,#22715,#22716,#22717,#22718,#22719,#22720,
#22721,#22722,#22723,#22724,#22725,#22726,#22727,#22728,#22729,#22730,#22731,
#22732,#22733,#22734,#22735,#22736,#22737,#22738,#22739,#22740,#22741,#22742,
#22743,#22744,#22745,#22746,#22747,#22748,#22749,#22750,#22751,#22752,#22753,
#22754,#22755,#22756,#22757,#22758,#22759,#22760,#22761,#22762,#22763,#22764,
#22765,#22766,#22767,#22768,#22769,#22770,#22771,#22772,#22773,#22774,#22775,
#22776,#22777,#22778,#22779,#22780,#22781,#22782,#22783,#22784,#22785,#22786,
#22787,#22788,#22789,#22790,#22791,#22792,#22793,#22794,#22795,#22796,#22797,
#22798,#22799,#22800,#22801,#22802,#22803,#22804,#22805,#22806,#22807,#22808,
#22809,#22810,#22811,#22812,#22813,#22814,#22815,#22816,#22817,#22818,#22819,
#22820,#22821,#22822,#22823,#22824,#22825,#22826,#22827,#22828,#22829,#22830,
#22831,#22832,#22833,#22834,#22835,#22836,#22837,#22838,#22839,#22840,#22841,
#22842,#22843,#22844,#22845,#22846,#22847,#22848,#22849,#22850,#22851,#22852,
#22853,#22854,#22855,#22856,#22857,#22858,#22859,#22860,#22861,#22862,#22863,
#22864,#22865,#22866,#22867,#22868,#22869,#22870,#22871,#22872,#22873,#22874,
#22875,#22876,#22877,#22878,#22879,#22880,#22881,#22882,#22883,#22884,#22885,
#22886,#22887,#22888,#22889,#22890,#22891,#22892,#22893,#22894,#22895,#22896,
#22897,#22898,#22899,#22900,#22901,#22902),.UNSPECIFIED.,.F.,.F.,(4,2,2,
2,2,2,2,2,2,2,2,2,2,2,2,2,2,2,2,2,2,2,2,2,2,2,2,2,2,2,2,2,2,2,2,2,2,2,2,
2,2,2,2,2,2,2,2,2,2,2,2,2,2,2,2,2,2,2,2,2,2,2,2,2,2,2,2,2,2,2,2,2,2,2,2,
2,2,2,2,2,2,2,2,2,2,2,2,2,2,2,2,2,2,2,2,2,2,2,4),(3.88489243871108,3.92114843911136,
3.92656013571019,3.92987713707966,3.9324522733762,3.93530605983754,3.94005588503002,
3.96041815001304,3.98933486616674,4.0038601255331,4.00684130011541,4.0085214093387,
4.00982332137784,4.01165439266635,4.01546184708096,4.03076426927921,4.0647053273136,
4.07865001671835,4.0830424625509,4.08581931758763,4.08841818411302,4.09190477054171,
4.09991638662898,4.11118802125539,4.15410919928886,4.15999890960721,4.16223883309563,
4.16359119989388,4.16509950099853,4.1673728664512,4.17400499664583,4.18502877768122,
4.2168562802777,4.23287953530137,4.23747879974249,4.2403003640074,4.24288419227716,
4.24626673441922,4.25367470103365,4.28282408075351,4.31122782526017,4.31537292236307,
4.31727616889885,4.31872594402144,4.32039269555107,4.32339348619826,4.34020867853257,
4.37462871920109,4.38803614840836,4.39237002355832,4.3951345729966,4.39773917536513,
4.4012601394897,4.40947670781103,4.44044145439295,4.46571228666464,4.47000530883829,
4.47190607237417,4.47335552999937,4.47502377836822,4.47803160834316,4.49504339424672,
4.53021274530603,4.5428371012365,4.54708648986297,4.54983303028564,4.5524462630988,
4.55601933802338,4.56455681225543,4.57685363467972,4.59718156069749,4.59922542152331,
4.62206633515296,4.62520700258585,4.62692277842189,4.62836538728244,4.63022812195892,
4.63420181190906,4.65094177479742,4.68039786180168,4.69666885651923,4.70129560173763,
4.70412304087402,4.70670510908676,4.71007502098321,4.71741242970433,4.74190433180067,
4.77076194799688,4.77804793297946,4.78047846486467,4.78202057229202,4.78352409031177,
4.78577440122295,4.79222657592678,4.80281629548545,4.83856415593349,4.8506049365565,
4.85389406752718,4.85639440324075),.UNSPECIFIED.);
#244=B_SPLINE_CURVE_WITH_KNOTS('',3,(#22903,#22904,#22905,#22906,#22907,
#22908,#22909,#22910,#22911,#22912,#22913,#22914,#22915,#22916,#22917,#22918,
#22919,#22920,#22921,#22922,#22923,#22924,#22925,#22926,#22927,#22928,#22929,
#22930,#22931,#22932,#22933,#22934,#22935,#22936,#22937,#22938,#22939,#22940,
#22941,#22942,#22943,#22944,#22945,#22946,#22947,#22948,#22949,#22950,#22951,
#22952,#22953,#22954,#22955,#22956,#22957,#22958,#22959,#22960,#22961,#22962,
#22963,#22964,#22965,#22966,#22967,#22968,#22969,#22970,#22971,#22972,#22973,
#22974,#22975,#22976,#22977,#22978,#22979,#22980,#22981,#22982,#22983,#22984,
#22985,#22986,#22987,#22988,#22989,#22990,#22991,#22992,#22993,#22994,#22995,
#22996,#22997,#22998,#22999,#23000,#23001,#23002,#23003,#23004,#23005,#23006,
#23007,#23008,#23009,#23010,#23011,#23012,#23013,#23014,#23015,#23016,#23017,
#23018,#23019,#23020,#23021,#23022,#23023,#23024,#23025,#23026,#23027,#23028,
#23029,#23030,#23031,#23032,#23033,#23034,#23035,#23036,#23037,#23038,#23039,
#23040,#23041,#23042,#23043,#23044,#23045,#23046,#23047,#23048,#23049,#23050,
#23051,#23052,#23053,#23054,#23055,#23056,#23057,#23058,#23059,#23060,#23061,
#23062,#23063,#23064,#23065,#23066,#23067,#23068,#23069,#23070,#23071,#23072,
#23073,#23074,#23075,#23076,#23077,#23078,#23079,#23080,#23081,#23082,#23083,
#23084,#23085,#23086,#23087,#23088,#23089,#23090,#23091,#23092,#23093,#23094,
#23095,#23096,#23097,#23098,#23099,#23100,#23101,#23102,#23103,#23104,#23105,
#23106),.UNSPECIFIED.,.F.,.F.,(4,2,2,2,2,2,2,2,2,2,2,2,2,2,2,2,2,2,2,2,
2,2,2,2,2,2,2,2,2,2,2,2,2,2,2,2,2,2,2,2,2,2,2,2,2,2,2,2,2,2,2,2,2,2,2,2,
2,2,2,2,2,2,2,2,2,2,2,2,2,2,2,2,2,2,2,2,2,2,2,2,2,2,2,2,2,2,2,2,2,2,2,2,
2,2,2,2,2,2,2,2,2,4),(8.68074318044454E-6,0.000834621271518507,0.00173280952585111,
0.00355963114514543,0.00791244521117191,0.0325924078649119,0.0637082748297012,
0.0720437098184778,0.0755925001490042,0.0782098340002669,0.0809808938060275,
0.0853107618666323,0.0985894049359075,0.133103219096935,0.149958024574866,
0.152968375369957,0.154641256738511,0.156097219500549,0.158010376055546,
0.162348137750859,0.185507039412247,0.206264126190896,0.218221226988665,
0.226593471511632,0.230148455544655,0.232766982559044,0.235536212871401,
0.239856756378913,0.25304641563528,0.287648468173131,0.304528149240935,
0.307539607759378,0.309212814345661,0.310668864453939,0.312581885754515,
0.316918317418711,0.340081690107502,0.360840544904464,0.372798664169237,
0.381171621812575,0.384726908647325,0.38734565869906,0.390115124885162,
0.394436036402009,0.40762681910747,0.442231818934014,0.459112937757,0.462124652781375,
0.463798001885804,0.465254176015673,0.467167360261257,0.471504161288867,
0.494669506996137,0.515430130015401,0.527389267783587,0.535762938582636,
0.539318528241047,0.54193750134877,0.544707203430572,0.549028482995861,
0.562220389314955,0.596828336624423,0.613710893310983,0.6167228648631,0.618396356497941,
0.619852654660281,0.621766001865311,0.626103172289309,0.649270491527636,
0.670032883382867,0.681993039275234,0.690367423053537,0.693923315522988,
0.696542511699596,0.699312449710978,0.703634097419727,0.716827128039619,
0.751438022523362,0.768322017045462,0.77133424514177,0.773007879318091,
0.774464301523692,0.776377811703755,0.780715351566238,0.803884647951786,
0.824648813439459,0.83660998283435,0.844985077253225,0.84854127216841,0.851160691368128,
0.853930865465378,0.858252881988832,0.871447042964835,0.906060879208404,
0.922946310159948,0.925958794766932,0.92763257148505,0.929089117746588,
0.931002790934689,0.935340700377612,0.958512009723332,0.971370657581808),
 .UNSPECIFIED.);
#245=B_SPLINE_CURVE_WITH_KNOTS('',3,(#23111,#23112,#23113,#23114,#23115,
#23116,#23117,#23118,#23119,#23120,#23121,#23122,#23123,#23124,#23125,#23126,
#23127,#23128,#23129,#23130,#23131,#23132,#23133,#23134,#23135,#23136,#23137,
#23138,#23139,#23140,#23141,#23142,#23143,#23144,#23145,#23146,#23147,#23148,
#23149,#23150,#23151,#23152,#23153,#23154,#23155,#23156,#23157,#23158,#23159,
#23160,#23161,#23162,#23163,#23164,#23165,#23166,#23167,#23168,#23169,#23170,
#23171,#23172,#23173,#23174,#23175,#23176,#23177,#23178,#23179,#23180,#23181,
#23182,#23183,#23184,#23185,#23186,#23187,#23188,#23189,#23190,#23191,#23192,
#23193,#23194,#23195,#23196,#23197,#23198,#23199,#23200,#23201,#23202,#23203,
#23204,#23205,#23206,#23207,#23208,#23209,#23210,#23211,#23212,#23213,#23214,
#23215,#23216,#23217,#23218,#23219,#23220,#23221,#23222,#23223,#23224,#23225,
#23226,#23227,#23228,#23229,#23230,#23231,#23232,#23233,#23234,#23235,#23236,
#23237,#23238,#23239,#23240,#23241,#23242,#23243,#23244,#23245,#23246,#23247,
#23248,#23249,#23250,#23251,#23252,#23253,#23254,#23255,#23256,#23257,#23258,
#23259,#23260,#23261,#23262,#23263,#23264,#23265,#23266,#23267,#23268,#23269,
#23270,#23271,#23272,#23273,#23274,#23275,#23276,#23277,#23278,#23279,#23280,
#23281,#23282,#23283,#23284,#23285,#23286,#23287,#23288,#23289,#23290,#23291,
#23292,#23293,#23294,#23295,#23296,#23297,#23298,#23299,#23300,#23301,#23302,
#23303,#23304,#23305,#23306,#23307,#23308,#23309,#23310,#23311,#23312,#23313,
#23314,#23315,#23316),.UNSPECIFIED.,.F.,.F.,(4,2,2,2,2,2,2,2,2,2,2,2,2,
2,2,2,2,2,2,2,2,2,2,2,2,2,2,2,2,2,2,2,2,2,2,2,2,2,2,2,2,2,2,2,2,2,2,2,2,
2,2,2,2,2,2,2,2,2,2,2,2,2,2,2,2,2,2,2,2,2,2,2,2,2,2,2,2,2,2,2,2,2,2,2,2,
2,2,2,2,2,2,2,2,2,2,2,2,2,2,2,2,2,4),(2.91352716392038,2.92212482027256,
2.92488138764063,2.92649497879777,2.92795908418521,2.92999858455716,2.93499109717784,
2.94237726532148,2.96818478069313,2.99507394356249,3.00012399632293,3.00307121175156,
3.00563220930499,3.00880097969311,3.01506754852075,3.03842966858025,3.06259523178947,
3.07632777435279,3.07926015573891,3.08092925845763,3.08223289030545,3.08407972677961,
3.08796964960132,3.1039746164507,3.13269775760315,3.15037353985382,3.15509602948967,
3.15794397369396,3.16052054463653,3.16384885099863,3.17095682835366,3.18055687794074,
3.20869358513345,3.23056715658777,3.23369639205691,3.23540958465394,3.23685236330121,
3.23871833615166,3.24270962649622,3.25960832398754,3.28922482092507,3.30519699361634,
3.30979756053083,3.31261925958587,3.31520277733571,3.31858428265464,3.32598734138549,
3.35770729684018,3.38341822677389,3.38770008357308,3.38959880091261,3.39104793077835,
3.39271726118508,3.3957304577294,3.41289943203876,3.44881449936663,3.46069966978749,
3.46486506607815,3.46759374421344,3.47021659919886,3.47384592631169,3.4827415395113,
3.49576147876501,3.51516429080594,3.52239732713388,3.53986462762231,3.54293413492266,
3.5446340214246,3.54607824345045,3.54796252885003,3.55205267116827,3.56985834260623,
3.60009683927851,3.61466321470322,3.61912480443844,3.62191651849675,3.62450968858381,
3.62795903241982,3.63575110225162,3.66165840818371,3.69307743509823,3.69704507335354,
3.69890662198317,3.70034907840885,3.70206560451353,3.70530197039488,3.7305938442555,
3.76612759885566,3.7722999426448,3.77549042435448,3.77805296650026,3.78098446292431,
3.7860964208165,3.81786535163903,3.84752243315254,3.851214243834,3.85305254609228,
3.85452929175845,3.85608352634331,3.85856979805513,3.86711179078751,3.88340845438037,
3.88489243871108),.UNSPECIFIED.);
#246=B_SPLINE_CURVE_WITH_KNOTS('',3,(#23317,#23318,#23319,#23320,#23321,
#23322,#23323,#23324,#23325,#23326,#23327,#23328,#23329,#23330,#23331,#23332,
#23333,#23334,#23335,#23336,#23337,#23338,#23339,#23340,#23341,#23342,#23343,
#23344,#23345,#23346,#23347,#23348,#23349,#23350,#23351,#23352,#23353,#23354,
#23355,#23356,#23357,#23358,#23359,#23360,#23361,#23362,#23363,#23364,#23365,
#23366,#23367,#23368,#23369,#23370,#23371,#23372,#23373,#23374,#23375,#23376,
#23377,#23378,#23379,#23380,#23381,#23382,#23383,#23384,#23385,#23386,#23387,
#23388,#23389,#23390,#23391,#23392,#23393,#23394,#23395,#23396,#23397,#23398,
#23399,#23400,#23401,#23402,#23403,#23404,#23405,#23406,#23407,#23408,#23409,
#23410,#23411,#23412,#23413,#23414,#23415,#23416,#23417,#23418,#23419,#23420,
#23421,#23422,#23423,#23424,#23425,#23426,#23427,#23428,#23429,#23430,#23431,
#23432,#23433,#23434,#23435,#23436,#23437,#23438,#23439,#23440,#23441,#23442,
#23443,#23444,#23445,#23446,#23447,#23448,#23449,#23450,#23451,#23452,#23453,
#23454,#23455,#23456,#23457,#23458,#23459,#23460,#23461,#23462,#23463,#23464,
#23465,#23466,#23467,#23468,#23469,#23470,#23471,#23472,#23473,#23474,#23475,
#23476,#23477,#23478,#23479,#23480,#23481,#23482,#23483,#23484,#23485,#23486,
#23487,#23488,#23489,#23490,#23491,#23492,#23493,#23494,#23495,#23496,#23497,
#23498,#23499,#23500,#23501,#23502,#23503,#23504,#23505,#23506,#23507,#23508,
#23509,#23510,#23511,#23512,#23513,#23514,#23515,#23516,#23517,#23518,#23519,
#23520,#23521,#23522,#23523,#23524),.UNSPECIFIED.,.F.,.F.,(4,2,2,2,2,2,
2,2,2,2,2,2,2,2,2,2,2,2,2,2,2,2,2,2,2,2,2,2,2,2,2,2,2,2,2,2,2,2,2,2,2,2,
2,2,2,2,2,2,2,2,2,2,2,2,2,2,2,2,2,2,2,2,2,2,2,2,2,2,2,2,2,2,2,2,2,2,2,2,
2,2,2,2,2,2,2,2,2,2,2,2,2,2,2,2,2,2,2,2,2,2,2,2,2,4),(0.971370657581808,
0.979277997018167,0.991240131328745,0.999615911644618,1.00317240498867,
1.00579204656183,1.00856245817241,1.01288485015418,1.02608020317924,1.06069692285973,
1.07758377455686,1.08059651512142,1.08227043426922,1.08372710462119,1.08564094103095,
1.08997922122614,1.11315291153842,1.13392121614515,1.1458838133258,1.15426002370785,
1.15781677380067,1.160436630868,1.16320729453397,1.16753013023196,1.18072731093024,
1.21534631004211,1.23223441952737,1.23524741014308,1.23692147045425,1.23837826515267,
1.2402922668557,1.24463092960056,1.26781085042781,1.28858663131252,1.30054445182912,
1.30891842181223,1.31247499335924,1.31509499395538,1.31786606135251,1.32219005327595,
1.33539569764978,1.37001066950027,1.38689833174362,1.38991151043589,1.39158569855271,
1.3930426201776,1.3949568087112,1.39929597709156,1.42253064686139,1.44337485726503,
1.46128708260616,1.46589493885138,1.46872704178241,1.47132420297448,1.47467246407102,
1.48028947067604,1.49259957033701,1.52517775118101,1.53629503838642,1.54297152385403,
1.5452571055728,1.54677288788755,1.54813185940556,1.55038322408958,1.5563084996177,
1.58629649017889,1.61508764045441,1.62017044177064,1.62310462820691,1.62568116343352,
1.62890465720159,1.63540425449226,1.66676551929197,1.68724691320141,1.69380937879914,
1.69838812140855,1.70036480117645,1.7018253970308,1.70348317868293,1.70634427066025,
1.71860735344789,1.7438013255651,1.76763481318485,1.77397276408173,1.77716480931454,
1.77973891734645,1.78269517899748,1.78774645505725,1.81781380738918,1.84111733777395,
1.84814571851921,1.85296342916564,1.85498032773697,1.85644658375467,1.85808378736496,
1.86092591854467,1.87240512350821,1.898155388249,1.92455457964085,1.92957734258209,
1.93249866801996,1.9350768592819,1.93831966467421,1.94318075099866),
 .UNSPECIFIED.);
#247=B_SPLINE_CURVE_WITH_KNOTS('',3,(#23529,#23530,#23531,#23532,#23533,
#23534,#23535,#23536,#23537,#23538,#23539,#23540,#23541,#23542,#23543,#23544,
#23545,#23546,#23547,#23548,#23549,#23550,#23551,#23552,#23553,#23554,#23555,
#23556,#23557,#23558,#23559,#23560,#23561,#23562,#23563,#23564,#23565,#23566,
#23567,#23568,#23569,#23570,#23571,#23572,#23573,#23574,#23575,#23576,#23577,
#23578,#23579,#23580,#23581,#23582,#23583,#23584,#23585,#23586,#23587,#23588,
#23589,#23590,#23591,#23592,#23593,#23594,#23595,#23596,#23597,#23598,#23599,
#23600,#23601,#23602,#23603,#23604,#23605,#23606,#23607,#23608,#23609,#23610,
#23611,#23612,#23613,#23614,#23615,#23616,#23617,#23618,#23619,#23620,#23621,
#23622,#23623,#23624,#23625,#23626,#23627,#23628,#23629,#23630,#23631,#23632,
#23633,#23634,#23635,#23636,#23637,#23638,#23639,#23640,#23641,#23642,#23643,
#23644,#23645,#23646,#23647,#23648,#23649,#23650,#23651,#23652,#23653,#23654,
#23655,#23656,#23657,#23658,#23659,#23660,#23661,#23662,#23663,#23664,#23665,
#23666,#23667,#23668,#23669,#23670,#23671,#23672,#23673,#23674,#23675,#23676,
#23677,#23678,#23679,#23680,#23681,#23682,#23683,#23684,#23685,#23686,#23687,
#23688,#23689,#23690,#23691,#23692,#23693,#23694,#23695,#23696,#23697,#23698,
#23699,#23700,#23701,#23702,#23703,#23704,#23705,#23706,#23707,#23708,#23709,
#23710,#23711,#23712,#23713,#23714,#23715,#23716,#23717,#23718,#23719,#23720,
#23721,#23722,#23723,#23724,#23725,#23726),.UNSPECIFIED.,.F.,.F.,(4,2,2,
2,2,2,2,2,2,2,2,2,2,2,2,2,2,2,2,2,2,2,2,2,2,2,2,2,2,2,2,2,2,2,2,2,2,2,2,
2,2,2,2,2,2,2,2,2,2,2,2,2,2,2,2,2,2,2,2,2,2,2,2,2,2,2,2,2,2,2,2,2,2,2,2,
2,2,2,2,2,2,2,2,2,2,2,2,2,2,2,2,2,2,2,2,2,2,2,4),(1.94227575636339,1.94606012199988,
1.97571217536218,1.9926199053659,1.99661156625058,1.9984773157092,1.99991972840137,
2.00163227418584,2.00475978212231,2.02651431365555,2.0547111591379,2.06431910950835,
2.0714315889137,2.07476020351083,2.07733627674735,2.08018292812399,2.08490150537415,
2.10251977375633,2.13129096851807,2.1473191074588,2.15121114362269,2.15305812141286,
2.15436150135844,2.15602982093617,2.15895976721434,2.17265670682989,2.19682333204858,
2.22017979226211,2.22644504745562,2.22961311231055,2.23217352947465,2.23512006630898,
2.24016892342347,2.2681614449127,2.29967791704117,2.30510960970925,2.30721706388844,
2.30869254398128,2.31027832891169,2.31290910232146,2.32201267224442,2.34945384016924,
2.37685147897525,2.38188510879577,2.38479950338163,2.38736348806987,2.3905774129512,
2.39707808220417,2.42788725642536,2.45597234416596,2.45977444644796,2.46163928365593,
2.46298912404641,2.46449959847563,2.46678475879825,2.47351408996637,2.48477781593115,
2.51870532238233,2.53265700246679,2.53704967634984,2.53982626438683,2.54242459771294,
2.54591003562909,2.55391700887379,2.56518046371741,2.60799697087485,2.61396822429828,
2.61621926782982,2.61757353405862,2.61907907482276,2.62134002742006,2.62787659692171,
2.63866956121232,2.65850129791815,2.68592481999823,2.69095996101765,2.69390377005905,
2.69646498309967,2.69963812421213,2.70592729348022,2.72947099415938,2.75403918440645,
2.76720130642072,2.77010472802123,2.77176724079776,2.77321758637382,2.77516038021447,
2.77957628986106,2.78583571601702,2.80469402736594,2.83832679364759,2.84463853199626,
2.84785782733945,2.8504226814839,2.85333440283375,2.85835401052689,2.8851860636777,
2.91168153582172,2.91352716392038),.UNSPECIFIED.);
#248=B_SPLINE_CURVE_WITH_KNOTS('',3,(#23727,#23728,#23729,#23730,#23731,
#23732,#23733,#23734,#23735,#23736,#23737,#23738,#23739,#23740,#23741,#23742,
#23743,#23744,#23745,#23746,#23747,#23748,#23749,#23750,#23751,#23752,#23753,
#23754,#23755,#23756,#23757,#23758,#23759,#23760,#23761,#23762,#23763,#23764,
#23765,#23766,#23767,#23768,#23769,#23770,#23771,#23772,#23773,#23774,#23775,
#23776,#23777,#23778,#23779,#23780,#23781,#23782,#23783,#23784,#23785,#23786,
#23787,#23788,#23789,#23790,#23791,#23792,#23793,#23794,#23795,#23796,#23797,
#23798,#23799,#23800,#23801,#23802,#23803,#23804,#23805,#23806,#23807,#23808,
#23809,#23810,#23811,#23812,#23813,#23814,#23815,#23816,#23817,#23818,#23819,
#23820,#23821,#23822,#23823,#23824,#23825,#23826,#23827,#23828,#23829,#23830,
#23831,#23832,#23833,#23834,#23835,#23836,#23837,#23838,#23839,#23840,#23841,
#23842,#23843,#23844,#23845,#23846,#23847,#23848,#23849,#23850,#23851,#23852,
#23853,#23854,#23855,#23856,#23857,#23858,#23859,#23860,#23861,#23862,#23863,
#23864,#23865,#23866,#23867,#23868,#23869,#23870,#23871,#23872,#23873,#23874,
#23875,#23876,#23877,#23878,#23879,#23880,#23881,#23882,#23883,#23884,#23885,
#23886,#23887,#23888,#23889,#23890,#23891,#23892,#23893,#23894,#23895,#23896,
#23897,#23898,#23899,#23900,#23901,#23902,#23903,#23904,#23905,#23906,#23907,
#23908,#23909,#23910,#23911,#23912,#23913,#23914,#23915,#23916,#23917,#23918,
#23919,#23920,#23921,#23922,#23923,#23924,#23925,#23926),.UNSPECIFIED.,
 .F.,.F.,(4,2,2,2,2,2,2,2,2,2,2,2,2,2,2,2,2,2,2,2,2,2,2,2,2,2,2,2,2,2,2,
2,2,2,2,2,2,2,2,2,2,2,2,2,2,2,2,2,2,2,2,2,2,2,2,2,2,2,2,2,2,2,2,2,2,2,2,
2,2,2,2,2,2,2,2,2,2,2,2,2,2,2,2,2,2,2,2,2,2,2,2,2,2,2,2,2,2,2,2,4),(1.94318075099866,
1.9449198072812,1.97261890963837,1.995819569099,2.00283190549208,2.00764146870455,
2.00965699748318,2.01112302858771,2.01276084670494,2.01560588362152,2.02712858789808,
2.05284750938481,2.07922886835664,2.084251023186,2.08717218475555,2.08975034447495,
2.09299326121901,2.09937520817257,2.13180342803993,2.15151755490416,2.15794295301821,
2.16245013482104,2.16441445003703,2.16587341224631,2.16753794281071,2.17042882170992,
2.18318705438527,2.20802840266903,2.2316957167679,2.23801297545379,2.24120091700669,
2.24377468137401,2.24673381322601,2.25179809407889,2.27867666689431,2.30450972255293,
2.31190868164312,2.3169119821349,2.31895909220625,2.32042997518728,2.32205311836209,
2.32483100450179,2.33543647401551,2.36180396000936,2.38622062984978,2.39262988999964,
2.39583578896418,2.39838725763012,2.40132496488738,2.40629390495854,2.42926122870977,
2.44732319463312,2.46934237407034,2.47248260926525,2.47420309487407,2.47565308593321,
2.47753050985365,2.48155472198726,2.49867808379253,2.52854028639414,2.54404881676014,
2.5486422113095,2.55147112582103,2.55406911058441,2.55748131859959,2.56500325592232,
2.59290053350538,2.62255713928356,2.62625668649689,2.62810130433826,2.62958451847937,
2.63114787730473,2.63365357108196,2.6423172607276,2.65897037247993,2.69609350093568,
2.70158344086033,2.70489551112571,2.70748754357272,2.71033742021486,2.71502821410594,
2.73417146660743,2.75406843857191,2.76100701961687,2.77879231342716,2.78187970926978,
2.7835884278339,2.7850397121151,2.78693338415877,2.79104542149832,2.80897942182484,
2.83958118453618,2.85373662015413,2.85816367452865,2.86095677927945,2.8635672107077,
2.8670640619128,2.87507746271276,2.88633861573731,2.91507246461277),
 .UNSPECIFIED.);
#249=B_SPLINE_CURVE_WITH_KNOTS('',3,(#23931,#23932,#23933,#23934,#23935,
#23936,#23937,#23938,#23939,#23940,#23941,#23942,#23943,#23944,#23945,#23946,
#23947,#23948,#23949,#23950,#23951,#23952,#23953,#23954,#23955,#23956,#23957,
#23958,#23959,#23960,#23961,#23962,#23963,#23964,#23965,#23966,#23967,#23968,
#23969,#23970,#23971,#23972,#23973,#23974,#23975,#23976,#23977,#23978,#23979,
#23980,#23981,#23982,#23983,#23984,#23985,#23986,#23987,#23988,#23989,#23990,
#23991,#23992,#23993,#23994,#23995,#23996,#23997,#23998,#23999,#24000,#24001,
#24002,#24003,#24004,#24005,#24006,#24007,#24008,#24009,#24010,#24011,#24012,
#24013,#24014,#24015,#24016,#24017,#24018,#24019,#24020,#24021,#24022,#24023,
#24024,#24025,#24026,#24027,#24028,#24029,#24030,#24031,#24032,#24033,#24034,
#24035,#24036,#24037,#24038,#24039,#24040,#24041,#24042,#24043,#24044,#24045,
#24046,#24047,#24048,#24049,#24050,#24051,#24052,#24053,#24054,#24055,#24056,
#24057,#24058,#24059,#24060,#24061,#24062,#24063,#24064,#24065,#24066,#24067,
#24068,#24069,#24070,#24071,#24072,#24073,#24074,#24075,#24076,#24077,#24078,
#24079,#24080,#24081,#24082,#24083,#24084,#24085,#24086,#24087,#24088,#24089,
#24090,#24091,#24092,#24093,#24094,#24095,#24096,#24097,#24098,#24099,#24100,
#24101,#24102,#24103,#24104,#24105,#24106,#24107,#24108,#24109,#24110,#24111,
#24112,#24113,#24114,#24115,#24116,#24117,#24118,#24119,#24120,#24121,#24122,
#24123,#24124,#24125,#24126,#24127,#24128,#24129,#24130,#24131,#24132,#24133,
#24134,#24135,#24136),.UNSPECIFIED.,.F.,.F.,(4,2,2,2,2,2,2,2,2,2,2,2,2,
2,2,2,2,2,2,2,2,2,2,2,2,2,2,2,2,2,2,2,2,2,2,2,2,2,2,2,2,2,2,2,2,2,2,2,2,
2,2,2,2,2,2,2,2,2,2,2,2,2,2,2,2,2,2,2,2,2,2,2,2,2,2,2,2,2,2,2,2,2,2,2,2,
2,2,2,2,2,2,2,2,2,2,2,2,2,2,2,2,2,4),(0.971183928329439,0.981978580297393,
0.989401327859789,0.992785759167962,0.995369105059563,0.998188251475987,
1.00277924958466,1.01865391345551,1.04834270021461,1.06528631472166,1.06928197282649,
1.07114847611538,1.07259095302642,1.07430295771319,1.07742799586797,1.09844372534886,
1.12721199756066,1.13691361258339,1.1440783144175,1.14741644304352,1.14999370968088,
1.15283547035284,1.15753132624397,1.17476253752569,1.20373062134106,1.21995788358913,
1.22387281787572,1.22572414150184,1.22702802935362,1.22869344022834,1.23161051040303,
1.24504973305628,1.26939901029108,1.29283771105136,1.2991132856649,1.30228338606068,
1.30484395024269,1.30778900397799,1.31283121134815,1.33961809664802,1.3655305769501,
1.37293124013626,1.3779303025948,1.37997059421145,1.3814345791128,1.38304728676066,
1.38580079242375,1.39621252604107,1.42270758721816,1.44953498976916,1.45455321926251,
1.45746426532755,1.46002860389898,1.46324735662422,1.46955835223679,1.50320419867449,
1.52206384330452,1.52832323121067,1.53273860156304,1.53468106903922,1.53613111878725,
1.53779326134986,1.54069592290172,1.55385477169786,1.57840233772069,1.60193104480362,
1.608217850225,1.61139014617916,1.61395084962223,1.61689426353616,1.6219291953336,
1.64858043756649,1.67461357454576,1.68203078476091,1.68703802966729,1.68907962577979,
1.6905438152654,1.69215593941916,1.69490680327333,1.70528653442309,1.73180419716634,
1.75864494565876,1.76366352646318,1.76657463884147,1.76913895430266,1.77235756962026,
1.7788829580155,1.80844893503423,1.83025608883817,1.84035003586668,1.84297447876203,
1.8445588313716,1.84601816219907,1.8481168146456,1.85202908873096,1.87630100960411,
1.90932997566341,1.91673698068668,1.9201186061708,1.92270155659123,1.92552198879771,
1.93011900053472,1.94227575636339),.UNSPECIFIED.);
#250=B_SPLINE_CURVE_WITH_KNOTS('',3,(#24137,#24138,#24139,#24140,#24141,
#24142,#24143,#24144,#24145,#24146,#24147,#24148,#24149,#24150,#24151,#24152,
#24153,#24154,#24155,#24156,#24157,#24158,#24159,#24160,#24161,#24162,#24163,
#24164,#24165,#24166,#24167,#24168,#24169,#24170,#24171,#24172,#24173,#24174,
#24175,#24176,#24177,#24178,#24179,#24180,#24181,#24182,#24183,#24184,#24185,
#24186,#24187,#24188,#24189,#24190,#24191,#24192,#24193,#24194,#24195,#24196,
#24197,#24198,#24199,#24200,#24201,#24202,#24203,#24204,#24205,#24206,#24207,
#24208,#24209,#24210,#24211,#24212,#24213,#24214,#24215,#24216,#24217,#24218,
#24219,#24220,#24221,#24222,#24223,#24224,#24225,#24226,#24227,#24228,#24229,
#24230,#24231,#24232,#24233,#24234,#24235,#24236,#24237,#24238,#24239,#24240,
#24241,#24242,#24243,#24244,#24245,#24246,#24247,#24248,#24249,#24250,#24251,
#24252,#24253,#24254,#24255,#24256,#24257,#24258,#24259,#24260,#24261,#24262,
#24263,#24264,#24265,#24266,#24267,#24268,#24269,#24270,#24271,#24272,#24273,
#24274,#24275,#24276,#24277,#24278,#24279,#24280,#24281,#24282,#24283,#24284,
#24285,#24286,#24287,#24288,#24289,#24290,#24291,#24292,#24293,#24294,#24295,
#24296,#24297,#24298,#24299,#24300,#24301,#24302,#24303,#24304,#24305,#24306,
#24307,#24308,#24309,#24310,#24311,#24312,#24313,#24314,#24315,#24316,#24317,
#24318,#24319,#24320,#24321,#24322,#24323,#24324,#24325,#24326,#24327,#24328,
#24329,#24330,#24331,#24332,#24333,#24334,#24335,#24336,#24337,#24338,#24339,
#24340,#24341,#24342),.UNSPECIFIED.,.F.,.F.,(4,2,2,2,2,2,2,2,2,2,2,2,2,
2,2,2,2,2,2,2,2,2,2,2,2,2,2,2,2,2,2,2,2,2,2,2,2,2,2,2,2,2,2,2,2,2,2,2,2,
2,2,2,2,2,2,2,2,2,2,2,2,2,2,2,2,2,2,2,2,2,2,2,2,2,2,2,2,2,2,2,2,2,2,2,2,
2,2,2,2,2,2,2,2,2,2,2,2,2,2,2,2,2,4),(2.91507246461277,2.92892983330798,
2.93509516237109,2.93738075274632,2.93874615004116,2.9402548103543,2.94250567280783,
2.94891181939204,2.95937704315373,2.97925187709222,3.00715373703291,3.01220125260113,
3.01515682255433,3.01773123803996,3.02092484345554,3.02726988664468,3.05115966669676,
3.07646309735543,3.08860236958841,3.09148728571456,3.09313389401542,3.09459758556087,
3.09659602088827,3.10130229099896,3.10811100018298,3.13004117415034,3.15943372786153,
3.16597586600442,3.16920776061695,3.17178525325416,3.17471433998824,3.17977234704304,
3.20743104356605,3.2353054443965,3.24386354716294,3.24644888360228,3.24802988722588,
3.24952022680718,3.25167754879362,3.2574029546012,3.26631794597162,3.28782523526673,
3.31655396307781,3.32159623887981,3.32455075938561,3.32712547601933,3.33032103230054,
3.33667535866395,3.36063851848362,3.38609251563041,3.39802302667916,3.40089441631143,
3.40253815581299,3.4040027933226,3.40600728005715,3.41074914141098,3.41762725967811,
3.43998152481581,3.4688258990976,3.47537357560256,3.47860667661035,3.48118443786163,
3.48411308533695,3.48916842141634,3.51670823744944,3.54437765586336,3.55321480934177,
3.55582832848231,3.55741560488964,3.55890269654982,3.56104216523377,3.56664439771152,
3.57529149614558,3.61293861000869,3.62723795007889,3.63168110210604,3.63447809538465,
3.6370878703782,3.64057731917508,3.64854387446908,3.67413671680118,3.70566659648351,
3.70958395400686,3.71144846979611,3.71290030663004,3.71460820413436,3.71777868320359,
3.74141412036115,3.77914121269257,3.78456775338773,3.78789767369664,3.79048541141279,
3.79335600238358,3.79814120537275,3.81885920918604,3.84727462794304,3.86191504451675,
3.8649107962956,3.86659923341252,3.86790791402729,3.86974956384311,3.87358361220623,
3.88714619154448),.UNSPECIFIED.);
#251=B_SPLINE_CURVE_WITH_KNOTS('',3,(#24347,#24348,#24349,#24350,#24351,
#24352,#24353,#24354,#24355,#24356,#24357,#24358,#24359,#24360,#24361,#24362,
#24363,#24364,#24365,#24366,#24367,#24368,#24369,#24370,#24371,#24372,#24373,
#24374,#24375,#24376,#24377,#24378,#24379,#24380,#24381,#24382,#24383,#24384,
#24385,#24386,#24387,#24388,#24389,#24390,#24391,#24392,#24393,#24394,#24395,
#24396,#24397,#24398,#24399,#24400,#24401,#24402,#24403,#24404,#24405,#24406,
#24407,#24408,#24409,#24410,#24411,#24412,#24413,#24414,#24415,#24416,#24417,
#24418,#24419,#24420,#24421,#24422,#24423,#24424,#24425,#24426,#24427,#24428,
#24429,#24430,#24431,#24432,#24433,#24434,#24435,#24436,#24437,#24438,#24439,
#24440,#24441,#24442,#24443,#24444,#24445,#24446,#24447,#24448,#24449,#24450,
#24451,#24452,#24453,#24454,#24455,#24456,#24457,#24458,#24459,#24460,#24461,
#24462,#24463,#24464,#24465,#24466,#24467,#24468,#24469,#24470,#24471,#24472,
#24473,#24474,#24475,#24476,#24477,#24478,#24479,#24480,#24481,#24482,#24483,
#24484,#24485,#24486,#24487,#24488,#24489,#24490,#24491,#24492,#24493,#24494,
#24495,#24496,#24497,#24498,#24499,#24500,#24501,#24502,#24503,#24504,#24505,
#24506,#24507,#24508,#24509,#24510,#24511,#24512,#24513,#24514,#24515,#24516,
#24517,#24518,#24519,#24520,#24521,#24522,#24523,#24524,#24525,#24526,#24527,
#24528,#24529,#24530,#24531,#24532,#24533,#24534,#24535,#24536,#24537,#24538,
#24539,#24540,#24541,#24542,#24543,#24544),.UNSPECIFIED.,.F.,.F.,(4,2,2,
2,2,2,2,2,2,2,2,2,2,2,2,2,2,2,2,2,2,2,2,2,2,2,2,2,2,2,2,2,2,2,2,2,2,2,2,
2,2,2,2,2,2,2,2,2,2,2,2,2,2,2,2,2,2,2,2,2,2,2,2,2,2,2,2,2,2,2,2,2,2,2,2,
2,2,2,2,2,2,2,2,2,2,2,2,2,2,2,2,2,2,2,2,2,2,2,4),(3.71760032817636E-5,0.03278469583082,
0.0563587893830542,0.0626514284411906,0.0658249701322316,0.0683858821371772,
0.0713286585911362,0.076360324979787,0.104235625211231,0.129287446885874,
0.136567454309088,0.14150664053465,0.14353735177536,0.144999865587911,0.146616953652437,
0.14939025023695,0.160047601256219,0.186335777941661,0.21309429534276,0.218110799715376,
0.221021565072916,0.223586083497252,0.226805630064309,0.233120032288051,
0.266710715841159,0.285610033406775,0.29187701324973,0.296296447900073,
0.298239683289246,0.299689884604605,0.301351715648585,0.304252789441236,
0.317379142574959,0.341951324916222,0.365491869975665,0.371780313659773,
0.374953024573585,0.377513869636035,0.380457233485767,0.385491551727468,
0.413050494466129,0.433138625376172,0.443690163139714,0.450125285100344,
0.452372961858122,0.45387560991684,0.455417750302452,0.457849845984146,
0.465152245768651,0.493970927540239,0.52215374812209,0.527206346535803,
0.530124787872092,0.532688246223326,0.535896107075785,0.542365392150518,
0.574187251074119,0.594329771245847,0.600824054159274,0.605362724250848,
0.607326610242817,0.608779387211021,0.610429520813941,0.613279257986403,
0.625509127753051,0.65071582067813,0.676814107350653,0.681811034053337,
0.684717556421354,0.687282572938134,0.690508395188122,0.696853581806874,
0.729811182356325,0.749147142434869,0.75549531249463,0.75995749671615,0.761908156281899,
0.763359235798578,0.765016722442816,0.767898791347565,0.78066927847836,
0.805491972683465,0.829147458303651,0.835450100375146,0.838625531888373,
0.841186490164272,0.844127694061621,0.849152646406451,0.877892520150095,
0.899429983843141,0.908320310967609,0.91402784059735,0.916175851308233,
0.917658770030781,0.919230297849247,0.921796432067453,0.930249207011913,
0.958170814870202,0.971183928329439),.UNSPECIFIED.);
#252=B_SPLINE_CURVE_WITH_KNOTS('',3,(#24546,#24547,#24548,#24549,#24550,
#24551,#24552,#24553,#24554,#24555,#24556,#24557,#24558,#24559,#24560,#24561,
#24562,#24563,#24564,#24565,#24566,#24567,#24568,#24569,#24570,#24571,#24572,
#24573,#24574,#24575,#24576,#24577,#24578,#24579,#24580,#24581,#24582,#24583,
#24584,#24585,#24586,#24587,#24588,#24589,#24590,#24591,#24592,#24593,#24594,
#24595,#24596,#24597,#24598,#24599,#24600,#24601,#24602,#24603,#24604,#24605,
#24606,#24607,#24608,#24609,#24610,#24611,#24612,#24613,#24614,#24615,#24616,
#24617,#24618,#24619,#24620,#24621,#24622,#24623,#24624,#24625,#24626,#24627,
#24628,#24629,#24630,#24631,#24632,#24633,#24634,#24635,#24636,#24637,#24638,
#24639,#24640,#24641,#24642,#24643,#24644,#24645,#24646,#24647,#24648,#24649,
#24650,#24651,#24652,#24653,#24654,#24655,#24656,#24657,#24658,#24659,#24660,
#24661,#24662,#24663,#24664,#24665,#24666,#24667,#24668,#24669,#24670,#24671,
#24672,#24673,#24674,#24675,#24676,#24677,#24678,#24679,#24680,#24681,#24682,
#24683,#24684,#24685,#24686,#24687,#24688,#24689,#24690,#24691,#24692,#24693,
#24694,#24695,#24696,#24697,#24698,#24699,#24700,#24701,#24702,#24703,#24704,
#24705,#24706,#24707,#24708,#24709,#24710,#24711,#24712,#24713,#24714,#24715,
#24716,#24717,#24718,#24719,#24720,#24721,#24722,#24723,#24724,#24725,#24726,
#24727,#24728,#24729,#24730,#24731,#24732,#24733,#24734,#24735,#24736,#24737),
 .UNSPECIFIED.,.F.,.F.,(4,2,2,2,2,2,2,2,2,2,2,2,2,2,2,2,2,2,2,2,2,2,2,2,
2,2,2,2,2,2,2,2,2,2,2,2,2,2,2,2,2,2,2,2,2,2,2,2,2,2,2,2,2,2,2,2,2,2,2,2,
2,2,2,2,2,2,2,2,2,2,2,2,2,2,2,2,2,2,2,2,2,2,2,2,2,2,2,2,2,2,2,2,2,2,2,4),
(3.88714619154448,3.88904047763074,3.92337707087601,3.9368685887607,3.94122442248375,
3.94400268807385,3.94662023297175,3.95015903961425,3.95842150992048,3.9895133701466,
4.01460583942679,4.01891333637113,4.02082217862764,4.02227867611456,4.02395672416928,
4.02698696700417,4.04435119938023,4.07304469944747,4.09081410353643,4.09555711310022,
4.09841863245391,4.1010084819,4.104355632429,4.11151234509875,4.12118754014292,
4.14971225519636,4.17108501371657,4.1742229054481,4.17594309641775,4.17739347450226,
4.17927221962773,4.18330219246631,4.200473585041,4.24287590994943,4.24908514021146,
4.25229262490926,4.25486811507121,4.25781388016512,4.26295004203676,4.29561457726858,
4.3242485980522,4.32843094909298,4.33031747457891,4.3317714145387,4.33346382172003,
4.33656145173604,4.35621865732663,4.38705124106428,4.40094664754376,4.40534698166918,
4.40813472222598,4.41074807879151,4.41426101332378,4.42236778024624,4.43380701886507,
4.47005956901946,4.48118795456977,4.48400603333332,4.48563818755824,4.48710643820127,
4.48913502877977,4.4940224392307,4.50118789742162,4.52539359298118,4.55432540624771,
4.55936779294089,4.56232242904433,4.56489727676177,4.56809303498626,4.57444789680388,
4.59841400940972,4.62387283079741,4.63579905187722,4.63867026231687,4.64031401309601,
4.6417787417417,4.64378346337462,4.6485263765485,4.65540643329968,4.67777163423897,
4.70653285405691,4.71312691302682,4.71636902005457,4.7189476972708,4.72187068583609,
4.72689912781784,4.75344411101109,4.77944225728865,4.79060484515618,4.79342549850228,
4.79505827166498,4.79652644920787,4.79855406078582,4.80343496672445,4.81058731918367,
4.85928900080305),.UNSPECIFIED.);
#253=B_SPLINE_CURVE_WITH_KNOTS('',3,(#24738,#24739,#24740,#24741),
 .UNSPECIFIED.,.F.,.F.,(4,4),(9.99997534344612E-7,6.60003561536544E-5),
 .UNSPECIFIED.);
#254=B_SPLINE_CURVE_WITH_KNOTS('',3,(#24747,#24748,#24749,#24750,#24751,
#24752,#24753,#24754,#24755,#24756,#24757,#24758,#24759,#24760,#24761,#24762,
#24763,#24764,#24765,#24766,#24767,#24768,#24769,#24770,#24771,#24772,#24773,
#24774,#24775,#24776,#24777,#24778,#24779,#24780,#24781,#24782,#24783,#24784,
#24785,#24786,#24787,#24788,#24789,#24790,#24791,#24792,#24793,#24794,#24795,
#24796,#24797,#24798,#24799,#24800,#24801,#24802,#24803,#24804,#24805,#24806,
#24807,#24808,#24809,#24810,#24811,#24812,#24813,#24814,#24815,#24816,#24817,
#24818,#24819,#24820,#24821,#24822,#24823,#24824,#24825,#24826,#24827,#24828,
#24829,#24830,#24831,#24832,#24833,#24834,#24835,#24836,#24837,#24838,#24839,
#24840,#24841,#24842,#24843,#24844,#24845,#24846,#24847,#24848,#24849,#24850,
#24851,#24852,#24853,#24854,#24855,#24856,#24857,#24858,#24859,#24860,#24861,
#24862,#24863,#24864,#24865,#24866,#24867,#24868,#24869,#24870,#24871,#24872,
#24873,#24874,#24875,#24876,#24877,#24878,#24879,#24880,#24881,#24882,#24883,
#24884,#24885,#24886,#24887,#24888,#24889,#24890,#24891,#24892,#24893,#24894,
#24895,#24896,#24897,#24898,#24899,#24900,#24901,#24902,#24903,#24904,#24905,
#24906,#24907,#24908,#24909,#24910,#24911,#24912,#24913,#24914,#24915,#24916,
#24917,#24918,#24919,#24920,#24921,#24922,#24923,#24924,#24925,#24926,#24927,
#24928,#24929,#24930,#24931,#24932,#24933,#24934,#24935,#24936,#24937,#24938,
#24939,#24940,#24941,#24942,#24943,#24944,#24945,#24946,#24947,#24948,#24949,
#24950,#24951,#24952),.UNSPECIFIED.,.F.,.F.,(4,2,2,2,2,2,2,2,2,2,2,2,2,
2,2,2,2,2,2,2,2,2,2,2,2,2,2,2,2,2,2,2,2,2,2,2,2,2,2,2,2,2,2,2,2,2,2,2,2,
2,2,2,2,2,2,2,2,2,2,2,2,2,2,2,2,2,2,2,2,2,2,2,2,2,2,2,2,2,2,2,2,2,2,2,2,
2,2,2,2,2,2,2,2,2,2,2,2,2,2,2,2,2,4),(0.971367835775262,0.998094173292414,
1.00234894763263,1.00424292364808,1.00569151645768,1.0073638562606,1.01039123684256,
1.0279810237121,1.05685453782617,1.07423204822755,1.07893735022615,1.08178157454706,
1.08435900800789,1.08769441721048,1.09484145362972,1.10451150391608,1.13307180573538,
1.1543984102362,1.15752541889822,1.15923809480626,1.16068088479313,1.16254744345115,
1.16654201582585,1.18347064374707,1.21311749279739,1.22906455797877,1.2336443704587,
1.23646155281658,1.23904632060158,1.2424373094354,1.24989413459048,1.27995385018521,
1.30733551430408,1.31114376790517,1.31301029331827,1.31436075156709,1.31587118764701,
1.3181549947914,1.3248707199154,1.33609963139502,1.36992386303947,1.38401729741264,
1.38842559341184,1.39120597995782,1.39380369474847,1.3972819409031,1.405243118424,
1.41641823676776,1.43639857184088,1.46182641650173,1.46611565634774,1.46801566557311,
1.4694649343276,1.47113341770954,1.47414276131796,1.49120327700166,1.52659441990255,
1.53899136783934,1.54321564207803,1.54595669417189,1.54857245185579,1.55216136662084,
1.56079950410705,1.57329785567181,1.59340544813696,1.59873477391159,1.61820286507637,
1.62131736843421,1.62302724251528,1.62447027973268,1.62634052994438,1.63035503934253,
1.64746448333872,1.67729620266772,1.69283846121881,1.6974212522254,1.70023902479084,
1.70282352002554,1.70621296503973,1.71366139995885,1.74124779457326,1.77136409510874,
1.77541529414148,1.77727250381039,1.77871713316958,1.78041405223617,1.78355711624091,
1.8060218451321,1.84431851969616,1.8506303939869,1.85384970621829,1.85641454876322,
1.85932623019209,1.86434570090037,1.89117383312301,1.9181079716179,1.92818047252751,
1.93090284163963,1.93250893244155,1.93389341514821,1.93534591863205,1.93827964096405,
1.942706406208),.UNSPECIFIED.);
#255=B_SPLINE_CURVE_WITH_KNOTS('',3,(#24953,#24954,#24955,#24956),
 .UNSPECIFIED.,.F.,.F.,(4,4),(9.99999999419236E-7,3.71760032817636E-5),
 .UNSPECIFIED.);
#256=B_SPLINE_CURVE_WITH_KNOTS('',3,(#24957,#24958,#24959,#24960,#24961,
#24962,#24963,#24964,#24965,#24966,#24967,#24968,#24969,#24970,#24971,#24972,
#24973,#24974,#24975,#24976,#24977,#24978,#24979,#24980,#24981,#24982,#24983,
#24984,#24985,#24986,#24987,#24988,#24989,#24990,#24991,#24992,#24993,#24994,
#24995,#24996,#24997,#24998,#24999,#25000,#25001,#25002,#25003,#25004,#25005,
#25006,#25007,#25008,#25009,#25010,#25011,#25012,#25013,#25014,#25015,#25016,
#25017,#25018,#25019,#25020,#25021,#25022,#25023,#25024,#25025,#25026,#25027,
#25028,#25029,#25030,#25031,#25032,#25033,#25034,#25035,#25036,#25037,#25038,
#25039,#25040,#25041,#25042,#25043,#25044,#25045,#25046,#25047,#25048,#25049,
#25050,#25051,#25052,#25053,#25054,#25055,#25056,#25057,#25058,#25059,#25060,
#25061,#25062,#25063,#25064,#25065,#25066,#25067,#25068,#25069,#25070,#25071,
#25072,#25073,#25074,#25075,#25076,#25077,#25078,#25079,#25080,#25081,#25082,
#25083,#25084,#25085,#25086,#25087,#25088,#25089,#25090,#25091,#25092,#25093,
#25094,#25095,#25096,#25097,#25098,#25099,#25100,#25101,#25102,#25103,#25104,
#25105,#25106,#25107,#25108,#25109,#25110,#25111,#25112,#25113,#25114,#25115,
#25116,#25117,#25118,#25119,#25120,#25121,#25122,#25123,#25124,#25125,#25126,
#25127,#25128,#25129,#25130,#25131,#25132,#25133,#25134,#25135,#25136,#25137,
#25138,#25139,#25140,#25141,#25142,#25143,#25144,#25145,#25146,#25147,#25148,
#25149,#25150,#25151,#25152,#25153,#25154,#25155,#25156,#25157,#25158,#25159,
#25160,#25161,#25162,#25163,#25164),.UNSPECIFIED.,.F.,.F.,(4,2,2,2,2,2,
2,2,2,2,2,2,2,2,2,2,2,2,2,2,2,2,2,2,2,2,2,2,2,2,2,2,2,2,2,2,2,2,2,2,2,2,
2,2,2,2,2,2,2,2,2,2,2,2,2,2,2,2,2,2,2,2,2,2,2,2,2,2,2,2,2,2,2,2,2,2,2,2,
2,2,2,2,2,2,2,2,2,2,2,2,2,2,2,2,2,2,2,2,2,2,2,2,2,4),(6.60003561536544E-5,
0.00509830578563299,0.00890644455873718,0.0114573845437381,0.0139160719651195,
0.0166825861635177,0.0209902987440654,0.03409017582065,0.06647418236722,
0.0855619923175944,0.0886430328165784,0.0903311055533978,0.091784398664254,
0.0936739598411391,0.0978782754695145,0.126226386619866,0.155161429625844,
0.162710920271129,0.166126662272053,0.168723817356241,0.171548394241512,
0.176126966844707,0.191492877015373,0.221017561224163,0.238563349854191,
0.242632337087529,0.244517393684056,0.245967181396833,0.247680210037605,
0.250789645678147,0.269555154245992,0.275533038578283,0.295550048962192,
0.308110048280513,0.316786121216338,0.320390074735872,0.323016989327633,
0.325770124806536,0.330014283483755,0.342493432290207,0.377791613484175,
0.389347911648222,0.396200583625539,0.398507288812623,0.400026918185239,
0.401381414683244,0.403610987263217,0.409390832399151,0.439483463495319,
0.468315318180592,0.473396399885783,0.476329237391912,0.478904384337202,
0.482125877371935,0.488620531468662,0.520005940590206,0.540444721812987,
0.546997989771674,0.551571281623472,0.553546348169862,0.555005980228067,
0.556662802150842,0.559522898669054,0.571801619368723,0.596966847608817,
0.620780331464314,0.627113507706498,0.630303211074365,0.632875448740539,
0.6358295739681,0.640877203440268,0.668402643247623,0.693707307415768,0.701029982043089,
0.705994512268106,0.708034513594095,0.709503487799869,0.71112810789276,
0.713915700554983,0.724659913984999,0.750915277546541,0.773322479339483,
0.781000187291292,0.784438529645841,0.787039108445138,0.78985409882879,
0.794387348770099,0.809587693452398,0.839289818077307,0.856898933691147,
0.860975159422045,0.862861819644608,0.864312320386488,0.866025869928257,
0.86913446506561,0.887814613287093,0.908797117278246,0.930370431045197,
0.936416771622968,0.93955066073554,0.941872105170914,0.944781910516068,
0.949752290371324,0.971346799428905),.UNSPECIFIED.);
#257=B_SPLINE_CURVE_WITH_KNOTS('',3,(#25170,#25171,#25172,#25173,#25174,
#25175,#25176,#25177,#25178,#25179,#25180,#25181,#25182,#25183,#25184,#25185,
#25186,#25187,#25188),.UNSPECIFIED.,.F.,.F.,(4,3,3,3,3,3,4),(1.57402034594183E-7,
0.0101506090236634,0.320442688740482,0.5,0.505274663924246,0.820442688740574,
0.999999999999516),.UNSPECIFIED.);
#258=B_SPLINE_CURVE_WITH_KNOTS('',3,(#25191,#25192,#25193,#25194,#25195,
#25196,#25197,#25198,#25199,#25200,#25201,#25202,#25203,#25204,#25205,#25206,
#25207,#25208,#25209,#25210,#25211,#25212,#25213,#25214,#25215,#25216,#25217,
#25218,#25219,#25220,#25221,#25222,#25223,#25224,#25225,#25226,#25227,#25228,
#25229,#25230,#25231,#25232,#25233,#25234,#25235,#25236,#25237,#25238,#25239,
#25240,#25241,#25242,#25243,#25244,#25245,#25246,#25247,#25248,#25249,#25250,
#25251,#25252,#25253,#25254,#25255,#25256,#25257,#25258,#25259,#25260,#25261,
#25262,#25263,#25264,#25265,#25266,#25267,#25268,#25269,#25270,#25271,#25272,
#25273,#25274,#25275,#25276,#25277,#25278,#25279,#25280,#25281,#25282,#25283,
#25284,#25285,#25286,#25287,#25288,#25289,#25290,#25291,#25292,#25293,#25294,
#25295,#25296,#25297,#25298,#25299,#25300),.UNSPECIFIED.,.F.,.F.,(4,2,2,
2,2,2,2,2,2,2,2,2,2,2,2,2,2,2,2,2,2,2,2,2,2,2,2,2,2,2,2,2,2,2,2,2,2,2,2,
2,2,2,2,2,2,2,2,2,2,2,2,2,2,2,4),(8.76930096496887E-5,0.00220428059398837,
0.00568383013496389,0.0303307759043643,0.0544825665568798,0.063817873399979,
0.0708027036708884,0.0741337354038329,0.0767392742264438,0.0796478823154546,
0.0845440334456498,0.104800038983582,0.134919545680411,0.142817236007138,
0.148073965356983,0.150185389521897,0.151687239457442,0.153309199107319,
0.156069872786612,0.166411689581759,0.192839035181447,0.219552369491333,
0.224570259786848,0.227485132444039,0.230055393280623,0.233285060518315,
0.239845606163803,0.268990206379869,0.299238582945375,0.302920325304879,
0.304754474096283,0.306227569333834,0.307766498216407,0.310225728504426,
0.318639456612004,0.334585704901009,0.373007914352284,0.378319946253382,
0.381589915132521,0.38413613061569,0.386965017071062,0.391688725824432,
0.412112790855365,0.440792353930564,0.455795390053634,0.45877543143784,
0.460443509871959,0.461736058117411,0.463548094120491,0.467275124240861,
0.492660976406284,0.527829958215341,0.533497363632991,0.535909822943192,
0.537775768622803),.UNSPECIFIED.);
#259=B_SPLINE_CURVE_WITH_KNOTS('',3,(#25306,#25307,#25308,#25309,#25310,
#25311,#25312,#25313,#25314,#25315,#25316,#25317,#25318,#25319,#25320,#25321,
#25322,#25323,#25324,#25325,#25326,#25327,#25328,#25329,#25330),
 .UNSPECIFIED.,.F.,.F.,(4,3,3,3,3,3,3,3,4),(0.,0.157792862860784,0.25,0.402378442421338,
0.5,0.652378442421304,0.75,0.907792862860534,1.),.UNSPECIFIED.);
#260=B_SPLINE_CURVE_WITH_KNOTS('',3,(#25332,#25333,#25334,#25335),
 .UNSPECIFIED.,.F.,.F.,(4,4),(0.155689172965689,0.175303809248541),
 .UNSPECIFIED.);
#261=B_SPLINE_CURVE_WITH_KNOTS('',3,(#25336,#25337,#25338,#25339,#25340,
#25341,#25342,#25343,#25344,#25345,#25346,#25347,#25348,#25349,#25350,#25351,
#25352,#25353),.UNSPECIFIED.,.F.,.F.,(4,2,2,2,2,2,2,2,4),(0.000250941785903305,
0.151853795676273,0.25,0.396282804485723,0.5,0.646282804485731,0.75,0.901853795676217,
1.),.UNSPECIFIED.);
#262=B_SPLINE_CURVE_WITH_KNOTS('',3,(#25358,#25359,#25360,#25361,#25362,
#25363,#25364,#25365,#25366,#25367,#25368,#25369,#25370,#25371,#25372,#25373,
#25374,#25375,#25376,#25377,#25378,#25379,#25380,#25381,#25382,#25383,#25384,
#25385,#25386,#25387,#25388,#25389,#25390,#25391),.UNSPECIFIED.,.F.,.F.,
(4,2,2,2,2,2,2,2,2,2,2,2,2,2,2,2,4),(0.,0.109988325501573,0.125,0.23296026575946,
0.25,0.358354397029719,0.375,0.483378945338423,0.5,0.608294453235343,0.625,
0.733345732989897,0.75,0.857948705197813,0.875,0.984973198402819,1.),
 .UNSPECIFIED.);
#263=B_SPLINE_CURVE_WITH_KNOTS('',3,(#25392,#25393,#25394,#25395,#25396,
#25397,#25398,#25399,#25400,#25401,#25402,#25403,#25404,#25405,#25406,#25407,
#25408,#25409,#25410,#25411,#25412,#25413,#25414,#25415,#25416,#25417,#25418,
#25419,#25420,#25421,#25422,#25423,#25424,#25425,#25426,#25427,#25428,#25429,
#25430,#25431,#25432,#25433,#25434,#25435,#25436,#25437,#25438,#25439,#25440),
 .UNSPECIFIED.,.F.,.F.,(4,3,3,3,3,3,3,3,3,3,3,3,3,3,3,3,4),(0.,0.109983686962011,
0.125,0.232957075765626,0.25,0.358356399835469,0.375,0.48333605083713,0.5,
0.608336050836012,0.625,0.733356399835935,0.75,0.857957075765578,0.875,
0.984983686958202,1.),.UNSPECIFIED.);
#264=B_SPLINE_CURVE_WITH_KNOTS('',3,(#25445,#25446,#25447,#25448,#25449,
#25450,#25451,#25452,#25453,#25454,#25455,#25456,#25457,#25458,#25459,#25460,
#25461,#25462,#25463,#25464,#25465,#25466,#25467,#25468,#25469,#25470,#25471,
#25472,#25473,#25474,#25475,#25476,#25477,#25478,#25479,#25480,#25481,#25482,
#25483,#25484,#25485,#25486,#25487,#25488,#25489,#25490,#25491,#25492,#25493,
#25494,#25495,#25496,#25497,#25498,#25499,#25500,#25501,#25502,#25503,#25504,
#25505,#25506,#25507,#25508,#25509,#25510,#25511,#25512,#25513,#25514,#25515,
#25516,#25517,#25518,#25519,#25520,#25521,#25522,#25523,#25524,#25525,#25526,
#25527,#25528,#25529,#25530,#25531,#25532,#25533,#25534,#25535,#25536,#25537,
#25538,#25539,#25540,#25541,#25542,#25543,#25544,#25545,#25546,#25547,#25548,
#25549,#25550,#25551,#25552,#25553,#25554,#25555,#25556,#25557,#25558,#25559,
#25560,#25561,#25562,#25563,#25564,#25565,#25566,#25567,#25568,#25569,#25570,
#25571,#25572,#25573,#25574,#25575,#25576,#25577,#25578,#25579,#25580,#25581,
#25582,#25583,#25584,#25585,#25586,#25587,#25588,#25589,#25590,#25591,#25592,
#25593,#25594,#25595,#25596,#25597,#25598,#25599,#25600,#25601,#25602,#25603,
#25604,#25605,#25606),.UNSPECIFIED.,.F.,.F.,(4,2,2,2,2,2,2,2,2,2,2,2,2,
2,2,2,2,2,2,2,2,2,2,2,2,2,2,2,2,2,2,2,2,2,2,2,2,2,2,2,2,2,2,2,2,2,2,2,2,
2,2,2,2,2,2,2,2,2,2,2,2,2,2,2,2,2,2,2,2,2,2,2,2,2,2,2,2,2,2,2,4),(-0.796526705481827,
-0.787640941015784,-0.784969985598708,-0.782706384755367,-0.780066614844884,
-0.775590151703796,-0.752801998234308,-0.73096932875452,-0.724386701502598,
-0.71991097401508,-0.715876616314145,-0.709260547728906,-0.681773468829423,
-0.665143928783108,-0.660440991667095,-0.657755123073246,-0.655160601070774,
-0.650908753296221,-0.627054474899414,-0.608279469465114,-0.600484027535724,
-0.595786471325523,-0.591384813002343,-0.585256042011791,-0.554279156357543,
-0.538493813991255,-0.534598057960354,-0.532069788794442,-0.52927476598896,
-0.524020352992956,-0.500326602124289,-0.481261567992463,-0.474440690591909,
-0.469922950426694,-0.465399475628605,-0.458546529915877,-0.440686428309571,
-0.425391380671531,-0.413012908116307,-0.409308093122338,-0.406810597119231,
-0.403936202063164,-0.398260952268314,-0.39025630621729,-0.358566344318047,
-0.350503878294458,-0.345757258247316,-0.341376223416114,-0.335384734570859,
-0.317516357450394,-0.293206087121349,-0.286391165134631,-0.283319629305644,
-0.281106856460015,-0.277898786226338,-0.270189289902916,-0.257367379611346,
-0.230930817331304,-0.224189463729992,-0.220135590777724,-0.215681118104049,
-0.209220088675575,-0.186443729527482,-0.164265495805742,-0.159845809532047,
-0.157217849351324,-0.154571289264464,-0.150060852240392,-0.135115780808072,
-0.104662437121048,-0.0984557913681036,-0.0940863041535525,-0.0894270559394841,
-0.0818344157323819,-0.0609587772238571,-0.0392274395486936,-0.0347847589950281,
-0.032152190913683,-0.0295111793780467,-0.0250260607396291,0.),
 .UNSPECIFIED.);
#265=B_SPLINE_CURVE_WITH_KNOTS('',3,(#25607,#25608,#25609,#25610,#25611,
#25612,#25613,#25614,#25615,#25616,#25617,#25618,#25619,#25620,#25621,#25622,
#25623,#25624,#25625,#25626,#25627,#25628,#25629,#25630,#25631,#25632,#25633,
#25634,#25635,#25636,#25637,#25638,#25639,#25640,#25641,#25642,#25643,#25644,
#25645,#25646,#25647,#25648,#25649,#25650,#25651,#25652,#25653,#25654,#25655),
 .UNSPECIFIED.,.F.,.F.,(4,3,3,3,3,3,3,3,3,3,3,3,3,3,3,3,4),(0.,0.110009589359278,
0.125,0.232983376003898,0.25,0.358382691626032,0.375,0.483362296118791,
0.5,0.60836229611875,0.625,0.733382691626039,0.75,0.857983376004365,0.875,
0.985009589359391,1.),.UNSPECIFIED.);
#266=B_SPLINE_CURVE_WITH_KNOTS('',3,(#25660,#25661,#25662,#25663,#25664,
#25665,#25666,#25667,#25668,#25669,#25670,#25671,#25672,#25673,#25674,#25675,
#25676,#25677,#25678,#25679,#25680,#25681,#25682,#25683,#25684,#25685,#25686,
#25687,#25688,#25689,#25690,#25691,#25692,#25693,#25694,#25695,#25696,#25697,
#25698,#25699,#25700,#25701,#25702,#25703,#25704,#25705,#25706,#25707,#25708,
#25709,#25710,#25711,#25712,#25713,#25714,#25715,#25716,#25717,#25718,#25719,
#25720,#25721,#25722,#25723,#25724,#25725,#25726,#25727,#25728,#25729,#25730,
#25731,#25732,#25733,#25734,#25735,#25736,#25737,#25738,#25739,#25740,#25741,
#25742,#25743,#25744,#25745,#25746,#25747,#25748,#25749,#25750,#25751,#25752,
#25753,#25754,#25755,#25756,#25757,#25758,#25759,#25760,#25761,#25762,#25763,
#25764,#25765,#25766,#25767,#25768,#25769,#25770,#25771,#25772,#25773,#25774,
#25775,#25776,#25777,#25778,#25779,#25780,#25781,#25782,#25783,#25784,#25785,
#25786,#25787,#25788,#25789,#25790,#25791,#25792,#25793,#25794,#25795,#25796,
#25797,#25798,#25799,#25800,#25801,#25802,#25803,#25804,#25805,#25806,#25807,
#25808,#25809,#25810,#25811,#25812,#25813),.UNSPECIFIED.,.F.,.F.,(4,2,2,
2,2,2,2,2,2,2,2,2,2,2,2,2,2,2,2,2,2,2,2,2,2,2,2,2,2,2,2,2,2,2,2,2,2,2,2,
2,2,2,2,2,2,2,2,2,2,2,2,2,2,2,2,2,2,2,2,2,2,2,2,2,2,2,2,2,2,2,2,2,2,2,2,
2,4),(-0.796626433927326,-0.793640581520238,-0.785620283949,-0.75568028508624,
-0.74255056199915,-0.738714547085683,-0.73620663770818,-0.733360336449524,
-0.727905815584501,-0.702584421545849,-0.683830192055982,-0.677728192881519,
-0.673303483107345,-0.668540221178598,-0.660520256434299,-0.630581497681404,
-0.617452316442157,-0.613616460357274,-0.61110865492475,-0.608262471886745,
-0.602808178121058,-0.577487851267826,-0.558734374603957,-0.552632627560487,
-0.548208101052797,-0.543445036838665,-0.535425406142308,-0.505487886405355,
-0.492359247875895,-0.488523550523903,-0.486015848759443,-0.483169782763419,
-0.477715712637789,-0.452396403724468,-0.433643743522045,-0.42754224966276,
-0.423117905796551,-0.418355037238492,-0.410335733214807,-0.380399452822331,
-0.367271365456845,-0.363435827135068,-0.360928229209102,-0.358082281479942,
-0.352628437398602,-0.327310173459904,-0.308558292665218,-0.30245705240812,
-0.298032892820156,-0.293270223102979,-0.285251255457627,-0.255316218204372,
-0.242188661692694,-0.238353282169347,-0.235845788770509,-0.232999961134182,
-0.227546351013326,-0.202229260735234,-0.183477996658464,-0.177377005022688,
-0.172953028529602,-0.168190558605416,-0.160171934513209,-0.130238130612887,
-0.11711111636167,-0.113275894959867,-0.110768503919532,-0.107922787699957,
-0.102469385145431,-0.0771530864554135,-0.0584029324467546,-0.0523021985126006,
-0.0478784013394972,-0.043116116880782,-0.0350977835281825,-0.00516521924404225,
-1.00000002178913E-6),.UNSPECIFIED.);
#267=B_SPLINE_CURVE_WITH_KNOTS('',3,(#25814,#25815,#25816,#25817,#25818,
#25819,#25820,#25821,#25822,#25823,#25824,#25825,#25826,#25827,#25828,#25829,
#25830,#25831,#25832,#25833,#25834,#25835,#25836,#25837,#25838,#25839,#25840,
#25841,#25842,#25843,#25844,#25845,#25846,#25847,#25848,#25849,#25850,#25851,
#25852,#25853,#25854,#25855,#25856,#25857,#25858,#25859,#25860,#25861,#25862),
 .UNSPECIFIED.,.F.,.F.,(4,3,3,3,3,3,3,3,3,3,3,3,3,3,3,3,4),(0.,0.109981554777347,
0.125,0.232954910826536,0.25,0.358354235590002,0.375,0.483333890418085,
0.5,0.608333890420568,0.625,0.73335423558997,0.75,0.857954910826484,0.875,
0.984981554779499,1.),.UNSPECIFIED.);
#268=B_SPLINE_CURVE_WITH_KNOTS('',3,(#25867,#25868,#25869,#25870,#25871,
#25872,#25873,#25874,#25875,#25876,#25877,#25878,#25879,#25880,#25881,#25882,
#25883,#25884,#25885,#25886,#25887,#25888,#25889,#25890,#25891,#25892,#25893,
#25894,#25895,#25896,#25897,#25898,#25899,#25900,#25901,#25902,#25903,#25904,
#25905,#25906,#25907,#25908,#25909,#25910,#25911,#25912,#25913,#25914,#25915,
#25916,#25917,#25918,#25919,#25920,#25921,#25922,#25923,#25924,#25925,#25926,
#25927,#25928,#25929,#25930,#25931,#25932,#25933,#25934,#25935,#25936,#25937,
#25938,#25939,#25940,#25941,#25942,#25943,#25944,#25945,#25946,#25947,#25948,
#25949,#25950,#25951,#25952,#25953,#25954,#25955,#25956,#25957,#25958,#25959,
#25960,#25961,#25962,#25963,#25964,#25965,#25966,#25967,#25968,#25969,#25970,
#25971,#25972,#25973,#25974,#25975,#25976,#25977,#25978,#25979,#25980,#25981,
#25982,#25983,#25984,#25985,#25986,#25987,#25988,#25989,#25990,#25991,#25992,
#25993,#25994,#25995,#25996,#25997,#25998,#25999,#26000,#26001,#26002,#26003,
#26004,#26005,#26006,#26007,#26008,#26009,#26010,#26011,#26012,#26013,#26014,
#26015,#26016,#26017,#26018,#26019,#26020),.UNSPECIFIED.,.F.,.F.,(4,2,2,
2,2,2,2,2,2,2,2,2,2,2,2,2,2,2,2,2,2,2,2,2,2,2,2,2,2,2,2,2,2,2,2,2,2,2,2,
2,2,2,2,2,2,2,2,2,2,2,2,2,2,2,2,2,2,2,2,2,2,2,2,2,2,2,2,2,2,2,2,2,2,2,2,
2,4),(-1.59344183207227,-1.5631015427112,-1.55534294381678,-1.55062716576884,
-1.54617987037097,-1.53993408148607,-1.51654561466502,-1.49445274621809,
-1.49001106992231,-1.4873650768753,-1.48469019848849,-1.48010649463389,
-1.46467298378037,-1.43511927646285,-1.42875749255833,-1.42433622713228,
-1.41966731840556,-1.41216025549249,-1.38170451660708,-1.36811341680057,
-1.36427989319193,-1.36177198004572,-1.35892372442787,-1.35346089649308,
-1.32802390503159,-1.30938174237699,-1.30328092048709,-1.29885564348651,
-1.29409048430771,-1.28606396015132,-1.25612283918375,-1.24299539285905,
-1.23915898984057,-1.23665070166086,-1.23380382118636,-1.22834784155515,
-1.20301380936049,-1.18426530506198,-1.17816246981553,-1.17373704793275,
-1.1689729236065,-1.16095125641983,-1.13100764563381,-1.1178767335622,-1.11404026314902,
-1.11153204316617,-1.10868537408301,-1.10323011271367,-1.07790468242545,
-1.05914900274413,-1.05304625632506,-1.04862099392943,-1.04385712734113,
-1.03583611901101,-1.00589361659963,-0.992762836478716,-0.988926501716389,
-0.986418381926754,-0.983571840315769,-0.978116855299387,-0.952793247609392,
-0.934037529225433,-0.927935018739069,-0.923509937172587,-0.918746274075594,
-0.910725631441768,-0.880784356481209,-0.867654076886061,-0.863817898541952,
-0.861309882207993,-0.85846345937844,-0.853008705277776,-0.827686223767837,
-0.808931201282278,-0.80282894179811,-0.798404043147548,-0.796626433927326),
 .UNSPECIFIED.);
#269=B_SPLINE_CURVE_WITH_KNOTS('',3,(#26021,#26022,#26023,#26024,#26025,
#26026,#26027,#26028,#26029,#26030,#26031,#26032,#26033,#26034,#26035,#26036,
#26037,#26038,#26039,#26040,#26041,#26042,#26043,#26044,#26045,#26046,#26047,
#26048,#26049,#26050,#26051,#26052,#26053,#26054,#26055,#26056,#26057,#26058,
#26059,#26060,#26061,#26062,#26063,#26064,#26065,#26066,#26067,#26068,#26069),
 .UNSPECIFIED.,.F.,.F.,(4,3,3,3,3,3,3,3,3,3,3,3,3,3,3,3,4),(0.,0.109981188115351,
0.125,0.232954538531684,0.25,0.358353863414904,0.375,0.48333351890363,0.5,
0.608333518903562,0.625,0.733353863414284,0.75,0.857954538531691,0.875,
0.984981188108003,1.),.UNSPECIFIED.);
#270=B_SPLINE_CURVE_WITH_KNOTS('',3,(#26074,#26075,#26076,#26077,#26078,
#26079,#26080,#26081,#26082,#26083,#26084,#26085,#26086,#26087,#26088,#26089,
#26090,#26091,#26092,#26093,#26094,#26095,#26096,#26097,#26098,#26099,#26100,
#26101,#26102,#26103,#26104,#26105,#26106,#26107,#26108,#26109,#26110,#26111,
#26112,#26113,#26114,#26115,#26116,#26117,#26118,#26119,#26120,#26121,#26122,
#26123,#26124,#26125,#26126,#26127,#26128,#26129,#26130,#26131,#26132,#26133,
#26134,#26135,#26136,#26137,#26138,#26139,#26140,#26141,#26142,#26143,#26144,
#26145,#26146,#26147,#26148,#26149,#26150,#26151,#26152,#26153,#26154,#26155,
#26156,#26157,#26158,#26159,#26160,#26161,#26162,#26163,#26164,#26165,#26166,
#26167,#26168,#26169,#26170,#26171,#26172,#26173,#26174,#26175,#26176,#26177,
#26178,#26179,#26180,#26181,#26182,#26183,#26184,#26185,#26186,#26187,#26188,
#26189,#26190,#26191,#26192,#26193,#26194,#26195,#26196,#26197,#26198,#26199,
#26200,#26201,#26202,#26203,#26204,#26205,#26206,#26207,#26208,#26209,#26210,
#26211,#26212,#26213,#26214,#26215,#26216,#26217,#26218,#26219,#26220,#26221,
#26222,#26223,#26224,#26225,#26226,#26227,#26228,#26229,#26230,#26231,#26232,
#26233,#26234,#26235,#26236,#26237,#26238,#26239,#26240,#26241,#26242,#26243,
#26244,#26245),.UNSPECIFIED.,.F.,.F.,(4,2,2,2,2,2,2,2,2,2,2,2,2,2,2,2,2,
2,2,2,2,2,2,2,2,2,2,2,2,2,2,2,2,2,2,2,2,2,2,2,2,2,2,2,2,2,2,2,2,2,2,2,2,
2,2,2,2,2,2,2,2,2,2,2,2,2,2,2,2,2,2,2,2,2,2,2,2,2,2,2,2,2,2,2,2,4),(-2.3902143501497,
-2.38554194577431,-2.37447330888417,-2.36950293640176,-2.36547360999595,
-2.36290730182847,-2.36012121013131,-2.3549810250734,-2.33114463532179,
-2.31204084732371,-2.30519157752972,-2.30064291951131,-2.29607627997444,
-2.28912645358936,-2.26886526315001,-2.25201845896579,-2.24578010835845,
-2.24101853522758,-2.23830773888958,-2.23569266117793,-2.23140494962123,
-2.2077432918209,-2.18555443767192,-2.1793330561332,-2.17488984483387,-2.17016681139977,
-2.16236723224184,-2.13072108025255,-2.12242046362916,-2.11659236808856,
-2.11367617722163,-2.11116241447302,-2.10745463890786,-2.09595699927284,
-2.07195583167083,-2.06287276797988,-2.0554987540172,-2.05085433544024,
-2.04641828763313,-2.03996521998969,-2.01108021899938,-1.99944540031978,
-1.99432996199589,-1.99021365590509,-1.98763133580489,-1.98487279251223,
-1.97987276871724,-1.95588491249837,-1.93671199725028,-1.92985340205595,
-1.92530300165537,-1.92073795328766,-1.91379742170667,-1.88949057636316,
-1.8697685298415,-1.86536422909586,-1.86272586726691,-1.86004288106547,
-1.8554188677267,-1.83975708712326,-1.82010937990871,-1.80812066085723,
-1.80270299401605,-1.79834900762235,-1.79320692548309,-1.78303650531064,
-1.75443173353944,-1.7466634593118,-1.74109683931642,-1.73822895069798,
-1.73572809115556,-1.73194035125851,-1.71955185148558,-1.68969650166847,
-1.68112832509411,-1.67626353586041,-1.67186991134657,-1.66610863690228,
-1.65182484725151,-1.62135953938078,-1.61589392031055,-1.61304501981348,
-1.6105371549527,-1.60670451035262,-1.59365382166334,-1.59344183207227),
 .UNSPECIFIED.);
#271=B_SPLINE_CURVE_WITH_KNOTS('',3,(#26246,#26247,#26248,#26249,#26250,
#26251,#26252,#26253,#26254,#26255,#26256,#26257,#26258,#26259,#26260,#26261,
#26262,#26263,#26264,#26265,#26266,#26267,#26268,#26269,#26270,#26271,#26272,
#26273,#26274,#26275,#26276,#26277,#26278,#26279,#26280,#26281,#26282,#26283,
#26284,#26285,#26286,#26287,#26288,#26289,#26290,#26291,#26292,#26293,#26294),
 .UNSPECIFIED.,.F.,.F.,(4,3,3,3,3,3,3,3,3,3,3,3,3,3,3,3,4),(0.,0.110009462588615,
0.125,0.232983247289302,0.25,0.358382562953094,0.375,0.483362167673359,
0.5,0.60836216767328,0.625,0.733382562953116,0.75,0.857983247290714,0.875,
0.985009462590842,1.),.UNSPECIFIED.);
#272=B_SPLINE_CURVE_WITH_KNOTS('',3,(#26300,#26301,#26302,#26303,#26304,
#26305,#26306,#26307,#26308,#26309,#26310,#26311,#26312,#26313,#26314,#26315,
#26316,#26317,#26318,#26319,#26320,#26321,#26322,#26323,#26324),
 .UNSPECIFIED.,.F.,.F.,(4,3,3,3,3,3,3,3,4),(0.,0.125,0.25,0.375,0.5,0.625,
0.75,0.875,1.),.UNSPECIFIED.);
#273=B_SPLINE_CURVE_WITH_KNOTS('',3,(#26327,#26328,#26329,#26330,#26331,
#26332,#26333,#26334,#26335,#26336,#26337,#26338,#26339,#26340,#26341,#26342,
#26343,#26344,#26345,#26346,#26347,#26348,#26349,#26350,#26351,#26352,#26353,
#26354,#26355,#26356,#26357,#26358,#26359,#26360,#26361,#26362,#26363,#26364,
#26365,#26366,#26367,#26368,#26369,#26370,#26371,#26372,#26373,#26374,#26375),
 .UNSPECIFIED.,.F.,.F.,(4,3,3,3,3,3,3,3,3,3,3,3,3,3,3,3,4),(0.,0.109988800771746,
0.125,0.232962268129454,0.25,0.358361590536211,0.375,0.483341232350794,
0.5,0.608341232350757,0.625,0.733361590536065,0.75,0.857962268128102,0.875,
0.984988800771637,0.999999856346085),.UNSPECIFIED.);
#274=B_SPLINE_CURVE_WITH_KNOTS('',3,(#26381,#26382,#26383,#26384,#26385,
#26386,#26387,#26388,#26389,#26390,#26391,#26392,#26393,#26394,#26395,#26396,
#26397,#26398,#26399,#26400,#26401,#26402,#26403,#26404,#26405),
 .UNSPECIFIED.,.F.,.F.,(4,3,3,3,3,3,3,3,4),(0.,0.148099938408352,0.25,0.392428578596628,
0.5,0.642428578596597,0.75,0.898099938408575,1.),.UNSPECIFIED.);
#275=B_SPLINE_CURVE_WITH_KNOTS('',3,(#26408,#26409,#26410,#26411,#26412,
#26413,#26414,#26415,#26416,#26417,#26418,#26419,#26420,#26421,#26422,#26423,
#26424,#26425,#26426,#26427,#26428,#26429,#26430,#26431,#26432),
 .UNSPECIFIED.,.F.,.F.,(4,3,3,3,3,3,3,3,4),(0.,0.125,0.25,0.375,0.5,0.625,
0.75,0.875,1.),.UNSPECIFIED.);
#276=B_SPLINE_CURVE_WITH_KNOTS('',3,(#26437,#26438,#26439,#26440,#26441,
#26442,#26443,#26444,#26445,#26446,#26447,#26448,#26449,#26450,#26451,#26452,
#26453,#26454,#26455,#26456,#26457,#26458,#26459,#26460,#26461,#26462,#26463,
#26464,#26465,#26466,#26467,#26468,#26469,#26470,#26471,#26472,#26473,#26474,
#26475,#26476,#26477,#26478,#26479,#26480,#26481,#26482,#26483,#26484,#26485),
 .UNSPECIFIED.,.F.,.F.,(4,3,3,3,3,3,3,3,3,3,3,3,3,3,3,3,4),(0.,0.109988656217671,
0.125,0.232962121355374,0.25,0.358361443808927,0.375,0.483341085883086,
0.5,0.608341085883097,0.625,0.733361443808902,0.75,0.85796212135537,0.875,
0.984988656217777,1.),.UNSPECIFIED.);
#277=B_SPLINE_CURVE_WITH_KNOTS('',3,(#26486,#26487,#26488,#26489,#26490,
#26491,#26492,#26493,#26494,#26495,#26496,#26497,#26498,#26499,#26500,#26501,
#26502,#26503,#26504,#26505,#26506,#26507,#26508,#26509,#26510,#26511,#26512,
#26513,#26514,#26515,#26516,#26517,#26518,#26519,#26520,#26521,#26522,#26523,
#26524,#26525,#26526,#26527,#26528,#26529,#26530,#26531,#26532,#26533,#26534),
 .UNSPECIFIED.,.F.,.F.,(4,3,3,3,3,3,3,3,3,3,3,3,3,3,3,3,4),(0.,0.110665262381513,
0.125,0.232406990370153,0.25,0.354480944471444,0.375,0.4375,0.5,0.5625,
0.625,0.743596242461822,0.75,0.849347812241323,0.875,0.967457627501634,
1.),.UNSPECIFIED.);
#278=B_SPLINE_CURVE_WITH_KNOTS('',3,(#26539,#26540,#26541,#26542,#26543,
#26544,#26545,#26546,#26547,#26548,#26549,#26550,#26551,#26552,#26553,#26554,
#26555,#26556,#26557,#26558,#26559,#26560,#26561,#26562,#26563,#26564,#26565,
#26566,#26567,#26568,#26569,#26570,#26571,#26572,#26573,#26574,#26575,#26576,
#26577,#26578,#26579,#26580,#26581,#26582,#26583,#26584,#26585,#26586,#26587),
 .UNSPECIFIED.,.F.,.F.,(4,3,3,3,3,3,3,3,3,3,3,3,3,3,3,3,4),(0.,0.110008283622672,
0.125,0.232982050215023,0.25,0.358381366264466,0.375,0.483360973100441,
0.5,0.608360973100499,0.625,0.733381366264475,0.75,0.857982050215031,0.875,
0.985008283625021,1.),.UNSPECIFIED.);
#279=B_SPLINE_CURVE_WITH_KNOTS('',3,(#26588,#26589,#26590,#26591,#26592,
#26593,#26594,#26595,#26596,#26597,#26598,#26599,#26600,#26601,#26602,#26603,
#26604,#26605,#26606,#26607,#26608,#26609,#26610,#26611,#26612,#26613,#26614,
#26615,#26616,#26617,#26618,#26619,#26620,#26621,#26622,#26623,#26624,#26625,
#26626,#26627,#26628,#26629,#26630,#26631,#26632,#26633,#26634,#26635,#26636),
 .UNSPECIFIED.,.F.,.F.,(4,3,3,3,3,3,3,3,3,3,3,3,3,3,3,3,4),(0.,0.109995624518602,
0.125,0.232969196690076,0.25,0.358368516873247,0.375,0.483348146433747,
0.5,0.60834814643373,0.625,0.733368516873222,0.75,0.857969196690087,0.875,
0.984995624518607,1.),.UNSPECIFIED.);
#280=B_SPLINE_CURVE_WITH_KNOTS('',3,(#26641,#26642,#26643,#26644,#26645,
#26646,#26647,#26648,#26649,#26650,#26651,#26652,#26653,#26654,#26655,#26656,
#26657,#26658,#26659,#26660,#26661,#26662,#26663,#26664,#26665,#26666,#26667,
#26668,#26669,#26670,#26671,#26672,#26673,#26674,#26675,#26676,#26677,#26678,
#26679,#26680,#26681,#26682,#26683,#26684,#26685,#26686,#26687,#26688,#26689),
 .UNSPECIFIED.,.F.,.F.,(4,3,3,3,3,3,3,3,3,3,3,3,3,3,3,3,4),(0.,0.109988095064951,
0.125,0.232961551582756,0.25,0.35836087421893,0.375,0.483340517301036,0.5,
0.608340517300975,0.625,0.733360874218944,0.75,0.857961551582776,0.875,
0.984988095064888,1.),.UNSPECIFIED.);
#281=B_SPLINE_CURVE_WITH_KNOTS('',3,(#26690,#26691,#26692,#26693,#26694,
#26695,#26696,#26697,#26698,#26699,#26700,#26701,#26702,#26703,#26704,#26705,
#26706,#26707,#26708,#26709,#26710,#26711,#26712,#26713,#26714,#26715,#26716,
#26717,#26718,#26719,#26720,#26721,#26722,#26723,#26724,#26725,#26726,#26727,
#26728,#26729,#26730,#26731,#26732,#26733,#26734,#26735,#26736,#26737,#26738),
 .UNSPECIFIED.,.F.,.F.,(4,3,3,3,3,3,3,3,3,3,3,3,3,3,3,3,4),(0.,0.110003210421414,
0.125,0.232976899099387,0.25,0.358376216809013,0.375,0.483355832748265,
0.5,0.608355832752626,0.625,0.733376216808992,0.75,0.857976899101109,0.875,
0.98500321042069,1.),.UNSPECIFIED.);
#282=B_SPLINE_CURVE_WITH_KNOTS('',3,(#26743,#26744,#26745,#26746,#26747,
#26748,#26749,#26750,#26751,#26752,#26753,#26754,#26755,#26756,#26757,#26758,
#26759,#26760,#26761,#26762,#26763,#26764,#26765,#26766,#26767,#26768,#26769,
#26770,#26771,#26772,#26773,#26774,#26775,#26776),.UNSPECIFIED.,.F.,.F.,
(4,2,2,2,2,2,2,2,2,2,2,2,2,2,2,2,4),(0.,0.109985596045135,0.125,0.23295933697955,
0.25,0.358356487411939,0.375,0.483342521801201,0.5,0.608357003630201,0.625,
0.733317144881367,0.75,0.857951550631935,0.875,0.984974973868141,1.),
 .UNSPECIFIED.);
#283=B_SPLINE_CURVE_WITH_KNOTS('',3,(#26777,#26778,#26779,#26780,#26781,
#26782,#26783,#26784,#26785,#26786,#26787,#26788,#26789,#26790,#26791,#26792,
#26793,#26794,#26795,#26796,#26797,#26798,#26799,#26800,#26801,#26802,#26803,
#26804,#26805,#26806,#26807,#26808,#26809,#26810,#26811,#26812,#26813,#26814,
#26815,#26816,#26817,#26818,#26819,#26820,#26821,#26822,#26823,#26824,#26825,
#26826,#26827,#26828,#26829,#26830,#26831,#26832,#26833,#26834,#26835,#26836,
#26837,#26838,#26839,#26840,#26841,#26842,#26843,#26844,#26845,#26846),
 .UNSPECIFIED.,.F.,.F.,(4,3,3,3,3,3,3,3,3,3,3,3,3,3,3,3,3,3,3,3,3,3,3,4),
(0.,0.0586198091601681,0.0625,0.125,0.1875,0.25,0.3125,0.375,0.40625,0.4375,
0.46875,0.484375,0.48828125,0.5,0.515625,0.53125,0.5625,0.625,0.6875,0.75,
0.858448953897341,0.875,0.984200206485096,1.),.UNSPECIFIED.);
#284=B_SPLINE_CURVE_WITH_KNOTS('',3,(#26851,#26852,#26853,#26854,#26855,
#26856,#26857,#26858,#26859,#26860,#26861,#26862,#26863,#26864,#26865,#26866,
#26867,#26868,#26869,#26870,#26871,#26872,#26873,#26874,#26875,#26876,#26877,
#26878,#26879,#26880,#26881,#26882,#26883,#26884,#26885,#26886,#26887,#26888,
#26889,#26890,#26891,#26892,#26893,#26894,#26895,#26896,#26897,#26898,#26899),
 .UNSPECIFIED.,.F.,.F.,(4,3,3,3,3,3,3,3,3,3,3,3,3,3,3,3,4),(0.,0.109997341214618,
0.125,0.23297093975572,0.25,0.35837025937904,0.375,0.483349885857099,0.5,
0.608349885857203,0.625,0.733370259379004,0.75,0.857970939755706,0.875,
0.984997341214533,1.),.UNSPECIFIED.);
#285=B_SPLINE_CURVE_WITH_KNOTS('',3,(#26900,#26901,#26902,#26903,#26904,
#26905,#26906,#26907,#26908,#26909,#26910,#26911,#26912,#26913,#26914,#26915,
#26916,#26917,#26918,#26919,#26920,#26921,#26922,#26923,#26924,#26925,#26926,
#26927,#26928,#26929,#26930,#26931,#26932,#26933,#26934,#26935,#26936,#26937,
#26938,#26939,#26940,#26941,#26942,#26943,#26944,#26945,#26946,#26947,#26948),
 .UNSPECIFIED.,.F.,.F.,(4,3,3,3,3,3,3,3,3,3,3,3,3,3,3,3,4),(0.,0.109983123479305,
0.125,0.23295650362664,0.25,0.358355827880222,0.375,0.483335479892581,0.5,
0.608335479892553,0.625,0.733355827880202,0.75,0.857956503626664,0.875,
0.984983123479114,1.),.UNSPECIFIED.);
#286=B_SPLINE_CURVE_WITH_KNOTS('',3,(#26953,#26954,#26955,#26956,#26957,
#26958,#26959,#26960,#26961,#26962,#26963,#26964,#26965,#26966,#26967,#26968,
#26969,#26970,#26971,#26972,#26973,#26974,#26975,#26976,#26977,#26978,#26979,
#26980,#26981,#26982,#26983,#26984,#26985,#26986,#26987,#26988,#26989,#26990,
#26991,#26992,#26993,#26994,#26995,#26996,#26997,#26998,#26999,#27000,#27001),
 .UNSPECIFIED.,.F.,.F.,(4,3,3,3,3,3,3,3,3,3,3,3,3,3,3,3,4),(0.,0.109997882182062,
0.125,0.232971489029442,0.25,0.358370808476237,0.375,0.48335043398321,0.5,
0.608350433983159,0.625,0.733370808476259,0.75,0.857971489029473,0.875,
0.984997882181992,1.),.UNSPECIFIED.);
#287=B_SPLINE_CURVE_WITH_KNOTS('',3,(#27002,#27003,#27004,#27005,#27006,
#27007,#27008,#27009,#27010,#27011,#27012,#27013,#27014,#27015,#27016,#27017,
#27018,#27019,#27020,#27021,#27022,#27023,#27024,#27025,#27026,#27027,#27028,
#27029,#27030,#27031,#27032,#27033,#27034,#27035,#27036,#27037,#27038,#27039,
#27040,#27041,#27042,#27043,#27044,#27045,#27046,#27047,#27048,#27049,#27050),
 .UNSPECIFIED.,.F.,.F.,(4,3,3,3,3,3,3,3,3,3,3,3,3,3,3,3,4),(0.,0.110006491219228,
0.125,0.232980230285482,0.25,0.358379546919392,0.375,0.483359156973627,
0.5,0.608359156973173,0.625,0.733379546920954,0.75,0.857980230285446,0.875,
0.985006491219265,1.),.UNSPECIFIED.);
#288=B_SPLINE_CURVE_WITH_KNOTS('',3,(#27055,#27056,#27057,#27058,#27059,
#27060,#27061,#27062,#27063,#27064,#27065,#27066,#27067,#27068,#27069,#27070,
#27071,#27072,#27073,#27074,#27075,#27076,#27077,#27078,#27079,#27080,#27081,
#27082,#27083,#27084,#27085,#27086,#27087,#27088,#27089,#27090,#27091,#27092,
#27093,#27094,#27095,#27096,#27097,#27098,#27099,#27100,#27101,#27102,#27103,
#27104,#27105,#27106,#27107,#27108,#27109,#27110,#27111,#27112,#27113,#27114,
#27115),.UNSPECIFIED.,.F.,.F.,(4,3,3,3,3,3,3,3,3,3,3,3,3,3,3,3,3,3,3,3,
4),(0.,0.109229796985621,0.125,0.233476713981996,0.25,0.3125,0.375,0.4375,
0.46875,0.484375,0.5,0.515625,0.53125,0.5625,0.625,0.6875,0.75,0.833497889959173,
0.875,0.9375,1.),.UNSPECIFIED.);
#289=B_SPLINE_CURVE_WITH_KNOTS('',3,(#27116,#27117,#27118,#27119,#27120,
#27121,#27122,#27123,#27124,#27125,#27126,#27127,#27128,#27129,#27130,#27131,
#27132,#27133,#27134,#27135,#27136,#27137,#27138,#27139,#27140,#27141,#27142,
#27143,#27144,#27145,#27146,#27147,#27148,#27149,#27150,#27151,#27152,#27153,
#27154,#27155,#27156,#27157,#27158,#27159,#27160,#27161,#27162,#27163,#27164),
 .UNSPECIFIED.,.F.,.F.,(4,3,3,3,3,3,3,3,3,3,3,3,3,3,3,3,4),(0.,0.109993207336737,
0.125,0.232966742381088,0.25,0.35836606335207,0.375,0.48334569725311,0.5,
0.608345697254482,0.625,0.733366063352394,0.75,0.8579667423811,0.875,0.984993207336734,
1.),.UNSPECIFIED.);
#290=B_SPLINE_CURVE_WITH_KNOTS('',3,(#27169,#27170,#27171,#27172,#27173,
#27174,#27175,#27176,#27177,#27178,#27179,#27180,#27181,#27182,#27183,#27184,
#27185,#27186,#27187,#27188,#27189,#27190,#27191,#27192,#27193,#27194,#27195,
#27196,#27197,#27198,#27199,#27200,#27201,#27202,#27203,#27204,#27205,#27206,
#27207,#27208,#27209,#27210,#27211,#27212,#27213,#27214,#27215,#27216,#27217),
 .UNSPECIFIED.,.F.,.F.,(4,3,3,3,3,3,3,3,3,3,3,3,3,3,3,3,4),(0.,0.109987471059102,
0.125,0.232960917994534,0.25,0.358360240830988,0.375,0.483339885033845,
0.5,0.608339885033874,0.625,0.733360240831014,0.75,0.857960917994191,0.875,
0.984987471059085,1.),.UNSPECIFIED.);
#291=B_SPLINE_CURVE_WITH_KNOTS('',3,(#27218,#27219,#27220,#27221,#27222,
#27223,#27224,#27225,#27226,#27227,#27228,#27229,#27230,#27231,#27232,#27233,
#27234,#27235,#27236,#27237,#27238,#27239,#27240,#27241,#27242,#27243,#27244,
#27245,#27246,#27247,#27248,#27249,#27250,#27251,#27252,#27253,#27254,#27255,
#27256,#27257,#27258,#27259,#27260,#27261,#27262,#27263),.UNSPECIFIED.,
 .F.,.F.,(4,3,3,3,3,3,3,3,3,3,3,3,3,3,3,4),(0.,0.109411056806016,0.125,
0.233524594880298,0.25,0.361851047408981,0.375,0.467122237965085,0.5,0.625,
0.729792305576865,0.75,0.85487283082487,0.875,0.978749428137399,1.),
 .UNSPECIFIED.);
#292=B_SPLINE_CURVE_WITH_KNOTS('',3,(#27268,#27269,#27270,#27271,#27272,
#27273,#27274,#27275,#27276,#27277,#27278,#27279,#27280,#27281,#27282,#27283,
#27284,#27285,#27286,#27287,#27288,#27289,#27290,#27291,#27292,#27293,#27294,
#27295,#27296,#27297,#27298,#27299,#27300,#27301,#27302,#27303,#27304,#27305,
#27306,#27307,#27308,#27309,#27310,#27311,#27312,#27313,#27314,#27315,#27316),
 .UNSPECIFIED.,.F.,.F.,(4,3,3,3,3,3,3,3,3,3,3,3,3,3,3,3,4),(0.,0.110008212483426,
0.125,0.232981977989281,0.25,0.358381294058765,0.375,0.48336090102248,0.5,
0.608360901022441,0.625,0.733381294058795,0.75,0.857981977986097,0.875,
0.985008212482492,1.),.UNSPECIFIED.);
#293=B_SPLINE_CURVE_WITH_KNOTS('',3,(#27317,#27318,#27319,#27320,#27321,
#27322,#27323,#27324,#27325,#27326,#27327,#27328,#27329,#27330,#27331,#27332,
#27333,#27334,#27335,#27336,#27337,#27338,#27339,#27340,#27341,#27342,#27343,
#27344,#27345,#27346,#27347,#27348,#27349,#27350,#27351,#27352,#27353,#27354,
#27355,#27356,#27357,#27358,#27359,#27360,#27361,#27362,#27363,#27364,#27365),
 .UNSPECIFIED.,.F.,.F.,(4,3,3,3,3,3,3,3,3,3,3,3,3,3,3,3,4),(0.,0.109994646065219,
0.125,0.232968203208124,0.25,0.35836752370985,0.375,0.483347155027715,0.5,
0.608347155027694,0.625,0.733367523710364,0.75,0.857968203208095,0.875,
0.984994646065316,1.),.UNSPECIFIED.);
#294=B_SPLINE_CURVE_WITH_KNOTS('',3,(#27370,#27371,#27372,#27373,#27374,
#27375,#27376,#27377,#27378,#27379,#27380,#27381,#27382,#27383,#27384,#27385,
#27386,#27387,#27388,#27389,#27390,#27391,#27392,#27393,#27394,#27395,#27396,
#27397,#27398,#27399,#27400,#27401,#27402,#27403,#27404,#27405,#27406,#27407,
#27408,#27409,#27410,#27411,#27412,#27413,#27414,#27415,#27416,#27417,#27418),
 .UNSPECIFIED.,.F.,.F.,(4,3,3,3,3,3,3,3,3,3,3,3,3,3,3,3,4),(0.,0.109989675774911,
0.125,0.232963156575604,0.25,0.358362478695303,0.375,0.483342118938395,
0.5,0.608342118938392,0.625,0.733362478695318,0.75,0.857963156572259,0.875,
0.984989675774944,1.),.UNSPECIFIED.);
#295=B_SPLINE_CURVE_WITH_KNOTS('',3,(#27419,#27420,#27421,#27422,#27423,
#27424,#27425,#27426,#27427,#27428,#27429,#27430,#27431,#27432,#27433,#27434,
#27435,#27436,#27437,#27438,#27439,#27440,#27441,#27442,#27443,#27444,#27445,
#27446,#27447,#27448,#27449,#27450,#27451,#27452,#27453,#27454,#27455,#27456,
#27457,#27458,#27459,#27460,#27461,#27462,#27463,#27464,#27465,#27466,#27467),
 .UNSPECIFIED.,.F.,.F.,(4,3,3,3,3,3,3,3,3,3,3,3,3,3,3,3,4),(0.,0.110004858025113,
0.125,0.232978572010577,0.25,0.358377889178609,0.375,0.483357502162731,
0.5,0.608357502162803,0.625,0.73337788917867,0.75,0.857978572010549,0.875,
0.985004858024923,1.),.UNSPECIFIED.);
#296=B_SPLINE_CURVE_WITH_KNOTS('',3,(#27473,#27474,#27475,#27476,#27477,
#27478,#27479,#27480,#27481,#27482,#27483,#27484,#27485,#27486,#27487,#27488,
#27489,#27490,#27491,#27492,#27493,#27494,#27495,#27496,#27497),
 .UNSPECIFIED.,.F.,.F.,(4,3,3,3,3,3,3,3,4),(0.,0.125,0.25,0.375,0.5,0.625,
0.75,0.875,1.),.UNSPECIFIED.);
#297=B_SPLINE_CURVE_WITH_KNOTS('',3,(#27500,#27501,#27502,#27503,#27504,
#27505,#27506,#27507,#27508,#27509,#27510,#27511,#27512,#27513,#27514,#27515,
#27516,#27517,#27518,#27519,#27520,#27521,#27522,#27523,#27524,#27525,#27526,
#27527,#27528,#27529,#27530,#27531,#27532,#27533,#27534,#27535,#27536,#27537,
#27538,#27539,#27540,#27541,#27542,#27543,#27544,#27545,#27546,#27547,#27548),
 .UNSPECIFIED.,.F.,.F.,(4,3,3,3,3,3,3,3,3,3,3,3,3,3,3,3,4),(1.05676601839088E-5,
0.110007241592374,0.125,0.232970353736968,0.25,0.358369673547411,0.375,
0.483349301063305,0.5,0.60834930106321,0.625,0.733369673548882,0.75,0.857970353739919,
0.875,0.98499676406314,1.),.UNSPECIFIED.);
#298=B_SPLINE_CURVE_WITH_KNOTS('',3,(#27550,#27551,#27552,#27553,#27554,
#27555,#27556,#27557,#27558,#27559,#27560,#27561,#27562,#27563,#27564,#27565,
#27566,#27567,#27568,#27569,#27570,#27571,#27572,#27573,#27574,#27575,#27576,
#27577,#27578,#27579,#27580,#27581,#27582,#27583),.UNSPECIFIED.,.F.,.F.,
(4,2,2,2,2,2,2,2,2,2,2,2,2,2,2,2,4),(0.,0.1099839788089,0.125,0.232958793615559,
0.25,0.358357719328499,0.375,0.483320936683858,0.5,0.608394468603398,0.625,
0.733299780434519,0.75,0.857953179030985,0.875,0.984975935865878,1.),
 .UNSPECIFIED.);
#299=B_SPLINE_CURVE_WITH_KNOTS('',3,(#27584,#27585,#27586,#27587,#27588,
#27589,#27590,#27591,#27592,#27593,#27594,#27595,#27596,#27597,#27598,#27599,
#27600,#27601,#27602,#27603,#27604,#27605,#27606,#27607,#27608,#27609,#27610,
#27611,#27612,#27613,#27614,#27615,#27616,#27617,#27618,#27619,#27620,#27621,
#27622,#27623,#27624,#27625,#27626,#27627,#27628,#27629,#27630,#27631,#27632),
 .UNSPECIFIED.,.F.,.F.,(4,3,3,3,3,3,3,3,3,3,3,3,3,3,3,3,4),(0.,0.109981115336569,
0.125,0.232954464634818,0.25,0.358353789540815,0.375,0.483333445161142,
0.5,0.608333445161148,0.625,0.733353789541188,0.75,0.857954464634781,0.875,
0.984981115336604,1.),.UNSPECIFIED.);
#300=B_SPLINE_CURVE_WITH_KNOTS('',3,(#27634,#27635,#27636,#27637,#27638,
#27639,#27640,#27641,#27642,#27643,#27644,#27645,#27646,#27647,#27648,#27649,
#27650,#27651,#27652,#27653,#27654,#27655,#27656,#27657,#27658,#27659,#27660,
#27661,#27662,#27663,#27664,#27665,#27666,#27667,#27668,#27669,#27670,#27671,
#27672,#27673,#27674,#27675,#27676,#27677,#27678,#27679,#27680,#27681,#27682,
#27683,#27684,#27685,#27686,#27687,#27688,#27689,#27690,#27691,#27692,#27693,
#27694,#27695,#27696,#27697,#27698,#27699,#27700,#27701,#27702,#27703,#27704,
#27705,#27706,#27707,#27708,#27709,#27710,#27711,#27712,#27713,#27714,#27715,
#27716,#27717,#27718,#27719,#27720,#27721,#27722,#27723,#27724,#27725,#27726,
#27727,#27728,#27729,#27730,#27731,#27732,#27733,#27734,#27735,#27736,#27737,
#27738,#27739,#27740,#27741,#27742,#27743,#27744,#27745,#27746,#27747,#27748,
#27749,#27750,#27751,#27752,#27753,#27754,#27755,#27756,#27757,#27758,#27759,
#27760,#27761,#27762,#27763,#27764,#27765,#27766,#27767,#27768,#27769,#27770,
#27771,#27772,#27773,#27774,#27775,#27776,#27777,#27778,#27779,#27780,#27781,
#27782,#27783,#27784,#27785,#27786,#27787,#27788,#27789,#27790,#27791,#27792,
#27793,#27794,#27795,#27796,#27797,#27798,#27799,#27800,#27801,#27802,#27803,
#27804,#27805),.UNSPECIFIED.,.F.,.F.,(4,2,2,2,2,2,2,2,2,2,2,2,2,2,2,2,2,
2,2,2,2,2,2,2,2,2,2,2,2,2,2,2,2,2,2,2,2,2,2,2,2,2,2,2,2,2,2,2,2,2,2,2,2,
2,2,2,2,2,2,2,2,2,2,2,2,2,2,2,2,2,2,2,2,2,2,2,2,2,2,2,2,2,2,2,2,4),(-3.18698728124793,
-3.18221150041198,-3.17770115961186,-3.17351534682041,-3.16794534503497,
-3.15510289974664,-3.14041186020985,-3.12656711296006,-3.12093142351134,
-3.11650988030342,-3.11386727450745,-3.11118717587842,-3.10657791508633,
-3.08620123136938,-3.06968503536365,-3.06202460328115,-3.05550292678536,
-3.05101124207204,-3.04692417253542,-3.04012330120204,-3.014050467194,-3.00106332653079,
-2.99562143285543,-2.99131261770304,-2.98869354071747,-2.98598864056323,
-2.98125503114169,-2.95697590185544,-2.9376706591066,-2.93079521268944,
-2.92624246073123,-2.92168170266288,-2.91476142321413,-2.89012631427218,
-2.87634138783952,-2.87071936786336,-2.86630615065774,-2.86366633762864,
-2.86098581479334,-2.8563731997087,-2.84113361751968,-2.82481174903563,
-2.81000401317442,-2.80424557943887,-2.79986443220269,-2.79494715004204,
-2.78633314665999,-2.75567772970282,-2.74774096640098,-2.74209068126568,
-2.7392071999634,-2.73668320320541,-2.73290562150034,-2.72063041979193,
-2.69068302951113,-2.68209322477362,-2.67722480156804,-2.67283260709197,
-2.6670800611951,-2.65287898102453,-2.62264197141188,-2.6169720173207,-2.61408498279469,
-2.61156230645776,-2.60779316367471,-2.59562470690211,-2.57223410085811,
-2.56324261321821,-2.5559217426326,-2.55128725491093,-2.54684510531043,
-2.54035402504735,-2.51174648636987,-2.4999883969495,-2.49266513269346,
-2.48949927524476,-2.48702287507504,-2.48375590382051,-2.47631287383972,
-2.44835612981682,-2.43877060704842,-2.43110978873152,-2.42641227829457,
-2.42200605065057,-2.41574067915496,-2.3902143501497),.UNSPECIFIED.);
#301=B_SPLINE_CURVE_WITH_KNOTS('',3,(#27806,#27807,#27808,#27809,#27810,
#27811,#27812,#27813,#27814,#27815,#27816,#27817,#27818,#27819,#27820,#27821,
#27822,#27823,#27824,#27825,#27826,#27827,#27828,#27829,#27830,#27831,#27832,
#27833,#27834,#27835,#27836,#27837,#27838,#27839,#27840,#27841,#27842,#27843,
#27844,#27845,#27846,#27847,#27848,#27849,#27850,#27851,#27852,#27853,#27854),
 .UNSPECIFIED.,.F.,.F.,(4,3,3,3,3,3,3,3,3,3,3,3,3,3,3,3,4),(0.,0.109984428745348,
0.125,0.232957828943971,0.25,0.358357152774683,0.375,0.483336802439457,
0.5,0.608336802440611,0.625,0.733357152772898,0.75,0.857957828943944,0.875,
0.984984428745393,1.),.UNSPECIFIED.);
#302=B_SPLINE_CURVE_WITH_KNOTS('',2,(#27983,#27984,#27985),
 .UNSPECIFIED.,.F.,.F.,(3,3),(0.,0.115758369027897),.UNSPECIFIED.);
#303=B_SPLINE_CURVE_WITH_KNOTS('',3,(#27997,#27998,#27999,#28000),
 .UNSPECIFIED.,.F.,.F.,(4,4),(0.,1.),.UNSPECIFIED.);
#304=B_SPLINE_CURVE_WITH_KNOTS('',3,(#28021,#28022,#28023,#28024,#28025,
#28026,#28027,#28028,#28029,#28030,#28031,#28032,#28033,#28034,#28035,#28036,
#28037,#28038,#28039,#28040,#28041,#28042,#28043,#28044,#28045),
 .UNSPECIFIED.,.F.,.F.,(4,3,3,3,3,3,3,3,4),(-0.226770318913044,-0.176070092740286,
-0.141340884398364,-0.125369866567527,-0.0941292001496635,-0.0702859439456138,
-0.0114755323037468,-0.00261123297662246,0.),.UNSPECIFIED.);
#305=B_SPLINE_CURVE_WITH_KNOTS('',3,(#28046,#28047,#28048,#28049,#28050,
#28051,#28052,#28053,#28054,#28055,#28056,#28057,#28058,#28059,#28060,#28061,
#28062,#28063,#28064,#28065,#28066,#28067,#28068,#28069,#28070,#28071,#28072,
#28073),.UNSPECIFIED.,.F.,.F.,(4,3,3,3,3,3,3,3,3,4),(-0.528419249915466,
-0.3824987601112,-0.313797789423033,-0.236578270306934,-0.180178655007884,
-0.091691640876666,-0.0576929606469953,-0.03032436788477,-0.00320462674544752,
-0.0001765620571701),.UNSPECIFIED.);
#306=B_SPLINE_CURVE_WITH_KNOTS('',3,(#28079,#28080,#28081,#28082),
 .UNSPECIFIED.,.F.,.F.,(4,4),(0.,1.),.UNSPECIFIED.);
#307=B_SPLINE_CURVE_WITH_KNOTS('',3,(#28104,#28105,#28106,#28107,#28108,
#28109,#28110,#28111,#28112,#28113,#28114,#28115,#28116,#28117,#28118,#28119,
#28120,#28121,#28122,#28123,#28124,#28125,#28126,#28127,#28128,#28129,#28130,
#28131,#28132,#28133,#28134,#28135,#28136,#28137,#28138,#28139,#28140,#28141,
#28142,#28143,#28144,#28145,#28146,#28147,#28148,#28149,#28150,#28151,#28152),
 .UNSPECIFIED.,.F.,.F.,(4,3,3,3,3,3,3,3,3,3,3,3,3,3,3,3,4),(0.,0.0927497600106301,
0.125,0.216040635762613,0.25,0.34137739623301,0.375,0.466360239331372,0.5,
0.591360239331263,0.625,0.716377396232998,0.75,0.841040635762724,0.875,
0.967749760010667,1.),.UNSPECIFIED.);
#308=B_SPLINE_CURVE_WITH_KNOTS('',3,(#28154,#28155,#28156,#28157,#28158,
#28159,#28160,#28161,#28162,#28163,#28164,#28165,#28166,#28167,#28168,#28169,
#28170,#28171,#28172,#28173,#28174,#28175,#28176,#28177,#28178,#28179,#28180,
#28181,#28182,#28183,#28184,#28185,#28186,#28187,#28188,#28189,#28190,#28191,
#28192,#28193,#28194,#28195,#28196,#28197,#28198,#28199,#28200,#28201,#28202),
 .UNSPECIFIED.,.F.,.F.,(4,3,3,3,3,3,3,3,3,3,3,3,3,3,3,3,4),(0.,0.0927530928142782,
0.125,0.216044019764289,0.25,0.341380779151096,0.375,0.466363616262366,
0.5,0.591363616262178,0.625,0.716380779151037,0.75,0.841044019764313,0.875,
0.967753092814524,1.),.UNSPECIFIED.);
#309=B_SPLINE_CURVE_WITH_KNOTS('',3,(#28204,#28205,#28206,#28207,#28208,
#28209,#28210,#28211,#28212,#28213,#28214,#28215,#28216,#28217,#28218,#28219,
#28220,#28221,#28222,#28223,#28224,#28225,#28226,#28227,#28228,#28229,#28230,
#28231,#28232,#28233,#28234,#28235,#28236,#28237,#28238,#28239,#28240,#28241,
#28242,#28243,#28244,#28245,#28246,#28247,#28248,#28249,#28250,#28251,#28252),
 .UNSPECIFIED.,.F.,.F.,(4,3,3,3,3,3,3,3,3,3,3,3,3,3,3,3,4),(0.,0.0927719347706172,
0.125,0.216063151119803,0.25,0.341399904362238,0.375,0.466382707642218,
0.5,0.591382707642052,0.625,0.716399904361949,0.75,0.841063151120002,0.875,
0.967771934770454,1.),.UNSPECIFIED.);
#310=B_SPLINE_CURVE_WITH_KNOTS('',3,(#28254,#28255,#28256,#28257,#28258,
#28259,#28260,#28261,#28262,#28263,#28264,#28265,#28266,#28267,#28268,#28269,
#28270,#28271,#28272,#28273,#28274,#28275,#28276,#28277,#28278,#28279,#28280,
#28281,#28282,#28283,#28284,#28285,#28286,#28287,#28288,#28289,#28290,#28291,
#28292,#28293,#28294,#28295,#28296,#28297,#28298,#28299,#28300,#28301,#28302,
#28303,#28304,#28305,#28306,#28307,#28308,#28309,#28310,#28311,#28312,#28313,
#28314,#28315,#28316,#28317,#28318,#28319,#28320,#28321,#28322,#28323,#28324,
#28325,#28326,#28327,#28328,#28329,#28330,#28331,#28332,#28333,#28334,#28335,
#28336,#28337,#28338,#28339,#28340,#28341,#28342,#28343,#28344,#28345,#28346,
#28347,#28348,#28349,#28350,#28351,#28352,#28353,#28354,#28355,#28356,#28357,
#28358,#28359,#28360,#28361,#28362,#28363,#28364,#28365,#28366,#28367,#28368,
#28369,#28370,#28371,#28372,#28373,#28374,#28375,#28376,#28377),
 .UNSPECIFIED.,.F.,.F.,(4,3,3,3,3,3,3,3,3,3,3,3,3,3,3,3,3,3,3,3,3,3,3,3,
3,3,3,3,3,3,3,3,3,3,3,3,3,3,3,3,3,4),(0.,0.0468270325633607,0.0625,0.064586021838547,
0.11912898254499,0.125,0.168623487537581,0.1875,0.25,0.3125,0.323789195493357,
0.375,0.4375,0.46875,0.484375,0.4921875,0.5,0.515625,0.53125,0.5625,0.625,
0.636035971190133,0.65625,0.6875,0.703125,0.71875,0.734375,0.741588067961916,
0.746426043014038,0.748801135923832,0.75216626473836,0.756085815752169,
0.764372920225663,0.78125,0.796875,0.8125,0.84375,0.875,0.92634083787367,
0.9375,0.995557989972811,1.),.UNSPECIFIED.);
#311=B_SPLINE_CURVE_WITH_KNOTS('',3,(#28379,#28380,#28381,#28382,#28383,
#28384,#28385,#28386,#28387,#28388,#28389,#28390,#28391,#28392,#28393,#28394,
#28395,#28396,#28397,#28398,#28399,#28400,#28401,#28402,#28403,#28404,#28405,
#28406,#28407,#28408,#28409,#28410,#28411,#28412,#28413,#28414,#28415,#28416,
#28417,#28418,#28419,#28420,#28421,#28422,#28423,#28424,#28425,#28426,#28427),
 .UNSPECIFIED.,.F.,.F.,(4,3,3,3,3,3,3,3,3,3,3,3,3,3,3,3,4),(0.,0.0927574051465889,
0.125,0.21604839833824,0.25,0.341385156321511,0.375,0.46636798568725,0.5,
0.591367985687259,0.625,0.716385156321534,0.75,0.841048398338404,0.875,
0.967757405146268,1.),.UNSPECIFIED.);
#312=B_SPLINE_CURVE_WITH_KNOTS('',3,(#28429,#28430,#28431,#28432,#28433,
#28434,#28435,#28436,#28437,#28438,#28439,#28440,#28441,#28442,#28443,#28444,
#28445,#28446,#28447,#28448,#28449,#28450,#28451,#28452,#28453,#28454,#28455,
#28456,#28457,#28458,#28459,#28460,#28461,#28462,#28463,#28464,#28465,#28466,
#28467,#28468,#28469,#28470,#28471,#28472,#28473,#28474,#28475,#28476,#28477),
 .UNSPECIFIED.,.F.,.F.,(4,3,3,3,3,3,3,3,3,3,3,3,3,3,3,3,4),(0.,0.0927663738152036,
0.125,0.21605750476053,0.25,0.341394259819506,0.375,0.466377073081152,0.5,
0.591377073081215,0.625,0.716394259819437,0.75,0.841057504760613,0.875,
0.967766373815486,1.),.UNSPECIFIED.);
#313=B_SPLINE_CURVE_WITH_KNOTS('',3,(#28479,#28480,#28481,#28482,#28483,
#28484,#28485,#28486,#28487,#28488,#28489,#28490,#28491,#28492,#28493,#28494,
#28495,#28496,#28497,#28498,#28499,#28500,#28501,#28502,#28503,#28504,#28505,
#28506,#28507,#28508,#28509,#28510,#28511,#28512),.UNSPECIFIED.,.F.,.F.,
(4,2,2,2,2,2,2,2,2,2,2,2,2,2,2,2,4),(0.,0.0927498161032601,0.125,0.216043543384793,
0.25,0.3413826281949,0.375,0.466317384484732,0.5,0.591468261682124,0.625,
0.716305724457278,0.75,0.841042047534153,0.875,0.967746874834895,1.),
 .UNSPECIFIED.);
#314=B_SPLINE_CURVE_WITH_KNOTS('',3,(#28514,#28515,#28516,#28517,#28518,
#28519,#28520,#28521,#28522,#28523,#28524,#28525,#28526,#28527,#28528,#28529,
#28530,#28531,#28532,#28533,#28534,#28535,#28536,#28537,#28538,#28539,#28540,
#28541,#28542,#28543,#28544,#28545,#28546,#28547,#28548,#28549,#28550,#28551,
#28552,#28553,#28554,#28555,#28556,#28557,#28558,#28559,#28560,#28561,#28562),
 .UNSPECIFIED.,.F.,.F.,(4,3,3,3,3,3,3,3,3,3,3,3,3,3,3,3,4),(0.,0.0927616901918672,
0.125,0.216052749201994,0.25,0.341389505789046,0.375,0.466372327459579,
0.5,0.591372327459986,0.625,0.716389505788987,0.75,0.841052749202119,0.875,
0.967761690191907,1.),.UNSPECIFIED.);
#315=B_SPLINE_CURVE_WITH_KNOTS('',3,(#28564,#28565,#28566,#28567,#28568,
#28569,#28570,#28571,#28572,#28573,#28574,#28575,#28576,#28577,#28578,#28579,
#28580,#28581,#28582,#28583,#28584,#28585,#28586,#28587,#28588,#28589,#28590,
#28591,#28592,#28593,#28594,#28595,#28596,#28597,#28598,#28599,#28600,#28601,
#28602,#28603,#28604,#28605,#28606,#28607,#28608,#28609,#28610,#28611,#28612),
 .UNSPECIFIED.,.F.,.F.,(4,3,3,3,3,3,3,3,3,3,3,3,3,3,3,3,4),(0.,0.0927693846977541,
0.125,0.216060561884735,0.25,0.341397315960308,0.375,0.466380123817375,
0.5,0.591380123817283,0.625,0.716397315960319,0.75,0.841060561884845,0.875,
0.967769384698343,1.),.UNSPECIFIED.);
#316=B_SPLINE_CURVE_WITH_KNOTS('',3,(#28614,#28615,#28616,#28617,#28618,
#28619,#28620,#28621,#28622,#28623,#28624,#28625,#28626,#28627,#28628,#28629,
#28630,#28631,#28632,#28633,#28634,#28635,#28636,#28637,#28638,#28639,#28640,
#28641,#28642,#28643,#28644,#28645,#28646,#28647,#28648,#28649,#28650),
 .UNSPECIFIED.,.F.,.F.,(4,3,3,3,3,3,3,3,3,3,3,3,4),(-0.157708230401766,
-0.138862257038452,-0.126648343324981,-0.119614872623337,-0.113538993032145,
-0.106944773722366,-0.0982823459339201,-0.0786512255255752,-0.0450114713913922,
-0.0124390832211188,-0.00494329693926847,-0.00231862606359825,0.),
 .UNSPECIFIED.);
#317=B_SPLINE_CURVE_WITH_KNOTS('',3,(#28654,#28655,#28656,#28657,#28658,
#28659,#28660,#28661,#28662,#28663,#28664,#28665,#28666),.UNSPECIFIED.,
 .F.,.F.,(4,3,3,3,4),(4.17257076022422E-7,0.41302767210967,0.5,0.913027257516351,
1.),.UNSPECIFIED.);
#318=B_SPLINE_CURVE_WITH_KNOTS('',3,(#28668,#28669,#28670,#28671,#28672,
#28673,#28674,#28675,#28676,#28677,#28678,#28679,#28680,#28681,#28682,#28683,
#28684,#28685,#28686,#28687,#28688,#28689,#28690,#28691,#28692,#28693,#28694,
#28695,#28696,#28697,#28698,#28699,#28700,#28701,#28702,#28703,#28704,#28705,
#28706,#28707,#28708,#28709,#28710,#28711,#28712,#28713,#28714,#28715,#28716),
 .UNSPECIFIED.,.F.,.F.,(4,3,3,3,3,3,3,3,3,3,3,3,3,3,3,3,4),(0.,0.0927564231352309,
0.125,0.216045703373452,0.25,0.341377418388321,0.375,0.466406748023344,
0.5,0.591313174398933,0.625,0.71637725021057,0.75,0.841035152620575,0.875,
0.967742717294513,1.),.UNSPECIFIED.);
#319=B_SPLINE_CURVE_WITH_KNOTS('',3,(#28718,#28719,#28720,#28721,#28722,
#28723,#28724,#28725,#28726,#28727,#28728,#28729,#28730,#28731,#28732,#28733,
#28734,#28735,#28736,#28737,#28738,#28739,#28740,#28741,#28742,#28743,#28744,
#28745,#28746,#28747,#28748,#28749,#28750,#28751,#28752,#28753,#28754,#28755,
#28756,#28757,#28758,#28759,#28760,#28761,#28762,#28763,#28764,#28765,#28766),
 .UNSPECIFIED.,.F.,.F.,(4,3,3,3,3,3,3,3,3,3,3,3,3,3,3,3,4),(0.,0.0927584978174006,
0.125,0.21604950779295,0.25,0.341386265420333,0.375,0.466369092823765,0.5,
0.591369092823743,0.625,0.716386265420279,0.75,0.841049507793065,0.875,
0.967758497817597,1.),.UNSPECIFIED.);
#320=B_SPLINE_CURVE_WITH_KNOTS('',3,(#28768,#28769,#28770,#28771,#28772,
#28773,#28774,#28775,#28776,#28777,#28778,#28779,#28780,#28781,#28782,#28783,
#28784,#28785,#28786,#28787,#28788,#28789,#28790,#28791,#28792,#28793,#28794,
#28795,#28796,#28797,#28798,#28799,#28800,#28801,#28802,#28803,#28804,#28805,
#28806,#28807,#28808,#28809,#28810,#28811,#28812,#28813,#28814,#28815,#28816),
 .UNSPECIFIED.,.F.,.F.,(4,3,3,3,3,3,3,3,3,3,3,3,3,3,3,3,4),(0.,0.0927642788375456,
0.125,0.21605537760672,0.25,0.341392133349299,0.375,0.466374950372504,0.5,
0.59137495037261,0.625,0.716392133349448,0.75,0.841055377606904,0.875,0.967764278837053,
1.),.UNSPECIFIED.);
#321=B_SPLINE_CURVE_WITH_KNOTS('',3,(#28818,#28819,#28820,#28821,#28822,
#28823,#28824,#28825,#28826,#28827,#28828,#28829,#28830,#28831,#28832,#28833,
#28834,#28835,#28836,#28837,#28838,#28839,#28840,#28841,#28842,#28843,#28844,
#28845,#28846,#28847,#28848,#28849,#28850,#28851,#28852,#28853,#28854,#28855,
#28856,#28857,#28858,#28859,#28860,#28861,#28862,#28863,#28864,#28865,#28866),
 .UNSPECIFIED.,.F.,.F.,(4,3,3,3,3,3,3,3,3,3,3,3,3,3,3,3,4),(0.,0.0928180932521736,
0.125,0.215969156459661,0.25,0.341016499097481,0.375,0.469480461922614,
0.5,0.58699659830702,0.625,0.7167307792291,0.75,0.841380676583067,0.875,
0.968438688021389,1.),.UNSPECIFIED.);
#322=B_SPLINE_CURVE_WITH_KNOTS('',3,(#28868,#28869,#28870,#28871,#28872,
#28873,#28874,#28875,#28876,#28877,#28878,#28879,#28880,#28881,#28882,#28883,
#28884,#28885,#28886,#28887,#28888,#28889,#28890,#28891,#28892,#28893,#28894,
#28895,#28896,#28897,#28898,#28899,#28900,#28901,#28902,#28903,#28904,#28905,
#28906,#28907,#28908,#28909,#28910,#28911,#28912,#28913,#28914,#28915,#28916),
 .UNSPECIFIED.,.F.,.F.,(4,3,3,3,3,3,3,3,3,3,3,3,3,3,3,3,4),(0.,0.0927640659933894,
0.125,0.216055161493703,0.25,0.341391917305785,0.375,0.466374734710861,
0.5,0.591374734710935,0.625,0.716391917305873,0.75,0.841055161493749,0.875,
0.967764065993903,1.),.UNSPECIFIED.);
#323=B_SPLINE_CURVE_WITH_KNOTS('',3,(#28918,#28919,#28920,#28921,#28922,
#28923,#28924,#28925,#28926,#28927,#28928,#28929,#28930,#28931,#28932,#28933,
#28934,#28935,#28936,#28937,#28938,#28939,#28940,#28941,#28942,#28943,#28944,
#28945,#28946,#28947,#28948,#28949,#28950,#28951,#28952,#28953,#28954,#28955,
#28956,#28957,#28958,#28959,#28960,#28961,#28962,#28963,#28964,#28965,#28966),
 .UNSPECIFIED.,.F.,.F.,(4,3,3,3,3,3,3,3,3,3,3,3,3,3,3,3,4),(0.,0.0927585881876831,
0.125,0.216049599551051,0.25,0.341386357148991,0.375,0.466369184390078,
0.5,0.591369184389981,0.625,0.716386357148919,0.75,0.841049599551146,0.875,
0.967758588187543,1.),.UNSPECIFIED.);
#324=B_SPLINE_CURVE_WITH_KNOTS('',3,(#28968,#28969,#28970,#28971,#28972,
#28973,#28974,#28975,#28976,#28977,#28978,#28979,#28980,#28981,#28982,#28983,
#28984,#28985,#28986,#28987,#28988,#28989,#28990,#28991,#28992,#28993,#28994,
#28995,#28996,#28997,#28998,#28999,#29000,#29001,#29002,#29003,#29004,#29005,
#29006,#29007,#29008,#29009,#29010,#29011,#29012,#29013,#29014,#29015,#29016,
#29017,#29018,#29019,#29020,#29021,#29022,#29023,#29024,#29025,#29026,#29027,
#29028,#29029,#29030,#29031,#29032,#29033,#29034,#29035,#29036,#29037,#29038,
#29039,#29040,#29041,#29042,#29043,#29044,#29045,#29046,#29047,#29048,#29049,
#29050,#29051,#29052,#29053,#29054,#29055,#29056,#29057,#29058,#29059,#29060,
#29061,#29062,#29063,#29064,#29065,#29066,#29067),.UNSPECIFIED.,.F.,.F.,
(4,3,3,3,3,3,3,3,3,3,3,3,3,3,3,3,3,3,3,3,3,3,3,3,3,3,3,3,3,3,3,3,3,4),(0.,
0.0939730383414856,0.0972745498842664,0.125,0.1875,0.25,0.254701161761956,
0.3125,0.375,0.40625,0.412096773522505,0.4375,0.46875,0.484375,0.4921875,
0.5,0.50390625,0.5078125,0.515625,0.53125,0.5625,0.59375,0.625,0.648660762160911,
0.6875,0.75,0.8125,0.815195003357837,0.875,0.929951775124377,0.932307451240959,
0.9375,0.989835529327015,1.),.UNSPECIFIED.);
#325=B_SPLINE_CURVE_WITH_KNOTS('',3,(#29069,#29070,#29071,#29072,#29073,
#29074,#29075,#29076,#29077,#29078,#29079,#29080,#29081,#29082,#29083,#29084,
#29085,#29086,#29087,#29088,#29089,#29090,#29091,#29092,#29093,#29094,#29095,
#29096,#29097,#29098,#29099,#29100,#29101,#29102,#29103,#29104,#29105,#29106,
#29107,#29108,#29109,#29110,#29111,#29112,#29113,#29114,#29115,#29116,#29117),
 .UNSPECIFIED.,.F.,.F.,(4,3,3,3,3,3,3,3,3,3,3,3,3,3,3,3,4),(0.,0.0927704812620034,
0.125,0.216061675289301,0.25,0.341398429006514,0.375,0.466381234895823,
0.5,0.591381234895582,0.625,0.716398429006577,0.75,0.841061675289124,0.875,
0.967770481262084,1.),.UNSPECIFIED.);
#326=B_SPLINE_CURVE_WITH_KNOTS('',3,(#29119,#29120,#29121,#29122,#29123,
#29124,#29125,#29126,#29127,#29128,#29129,#29130,#29131,#29132,#29133,#29134,
#29135,#29136,#29137,#29138,#29139,#29140,#29141,#29142,#29143,#29144,#29145,
#29146,#29147,#29148,#29149,#29150,#29151,#29152,#29153,#29154,#29155,#29156,
#29157,#29158,#29159,#29160,#29161,#29162,#29163,#29164,#29165,#29166,#29167),
 .UNSPECIFIED.,.F.,.F.,(4,3,3,3,3,3,3,3,3,3,3,3,3,3,3,3,4),(0.,0.092754524514728,
0.125,0.216045473457587,0.25,0.34138223237852,0.375,0.466365066918033,0.5,
0.591365066918176,0.625,0.716382232378618,0.75,0.841045473457608,0.875,
0.967754524515514,1.),.UNSPECIFIED.);
#327=B_SPLINE_CURVE_WITH_KNOTS('',3,(#29168,#29169,#29170,#29171,#29172,
#29173,#29174,#29175,#29176,#29177,#29178,#29179,#29180,#29181,#29182,#29183,
#29184,#29185,#29186,#29187,#29188,#29189,#29190,#29191,#29192,#29193,#29194,
#29195,#29196,#29197,#29198,#29199,#29200,#29201,#29202,#29203,#29204,#29205,
#29206,#29207,#29208,#29209,#29210,#29211,#29212,#29213,#29214,#29215,#29216),
 .UNSPECIFIED.,.F.,.F.,(4,3,3,3,3,3,3,3,3,3,3,3,3,3,3,3,4),(0.,0.106472604170083,
0.125,0.229954011808637,0.25,0.35528007535872,0.375,0.4802448705967,0.5,
0.605244870596807,0.625,0.730280075360275,0.75,0.854954011808786,0.875,
0.98147260417198,1.),.UNSPECIFIED.);
#328=B_SPLINE_CURVE_WITH_KNOTS('',3,(#29217,#29218,#29219,#29220,#29221,
#29222,#29223,#29224,#29225,#29226,#29227,#29228,#29229,#29230,#29231,#29232,
#29233,#29234,#29235,#29236,#29237,#29238,#29239,#29240,#29241,#29242,#29243,
#29244,#29245,#29246,#29247,#29248,#29249,#29250,#29251,#29252,#29253,#29254,
#29255,#29256,#29257,#29258,#29259,#29260,#29261,#29262,#29263,#29264,#29265),
 .UNSPECIFIED.,.F.,.F.,(4,3,3,3,3,3,3,3,3,3,3,3,3,3,3,3,4),(0.,0.0927744783480364,
0.125,0.216065733758611,0.25,0.341402486168678,0.375,0.466385284884496,
0.5,0.591385284884159,0.625,0.716402486168833,0.75,0.841065733758618,0.875,
0.967774478348059,1.),.UNSPECIFIED.);
#329=B_SPLINE_CURVE_WITH_KNOTS('',3,(#29270,#29271,#29272,#29273,#29274,
#29275,#29276,#29277,#29278,#29279,#29280,#29281,#29282,#29283,#29284,#29285),
 .UNSPECIFIED.,.F.,.F.,(4,3,3,3,3,4),(-0.529687579579074,-0.331590427453144,
-0.219920121605962,-0.150766908575684,-0.0882648636903197,0.),
 .UNSPECIFIED.);
#330=B_SPLINE_CURVE_WITH_KNOTS('',3,(#29286,#29287,#29288,#29289,#29290,
#29291,#29292,#29293,#29294,#29295,#29296,#29297,#29298,#29299,#29300,#29301,
#29302,#29303,#29304),.UNSPECIFIED.,.F.,.F.,(4,3,3,3,3,3,4),(-0.425594667631933,
-0.326610996136396,-0.263194447999632,-0.22762732464086,-0.156642940697186,
-0.119119097859436,-0.000122244586405741),.UNSPECIFIED.);
#331=B_SPLINE_CURVE_WITH_KNOTS('',3,(#29306,#29307,#29308,#29309,#29310,
#29311,#29312,#29313,#29314,#29315,#29316,#29317,#29318,#29319,#29320,#29321,
#29322,#29323,#29324,#29325,#29326,#29327,#29328,#29329,#29330),
 .UNSPECIFIED.,.F.,.F.,(4,3,3,3,3,3,3,3,4),(-0.188664084190461,-0.152061353030785,
-0.128429664012943,-0.115458621871108,-0.0964653635667077,-0.0843255862211543,
-0.0416444979807187,-0.00599163753997056,0.),.UNSPECIFIED.);
#332=B_SPLINE_CURVE_WITH_KNOTS('',3,(#29331,#29332,#29333,#29334,#29335,
#29336,#29337,#29338,#29339,#29340,#29341,#29342,#29343,#29344,#29345,#29346,
#29347,#29348,#29349,#29350,#29351,#29352),.UNSPECIFIED.,.F.,.F.,(4,3,3,
3,3,3,3,4),(-0.312582490464858,-0.230760194515857,-0.19070267351417,-0.148937898566855,
-0.112852497416037,-0.0497426635164272,-0.0051444580421514,-0.000153083505448296),
 .UNSPECIFIED.);
#333=B_SPLINE_CURVE_WITH_KNOTS('',3,(#29372,#29373,#29374,#29375),
 .UNSPECIFIED.,.F.,.F.,(4,4),(0.537775768622803,0.537783217741629),
 .UNSPECIFIED.);
#334=B_SPLINE_CURVE_WITH_KNOTS('',3,(#29376,#29377,#29378,#29379,#29380,
#29381,#29382,#29383,#29384,#29385,#29386,#29387,#29388,#29389,#29390,#29391,
#29392,#29393,#29394,#29395,#29396,#29397,#29398,#29399,#29400,#29401,#29402,
#29403,#29404,#29405,#29406,#29407,#29408,#29409,#29410,#29411,#29412,#29413,
#29414,#29415,#29416,#29417,#29418,#29419,#29420,#29421,#29422,#29423,#29424,
#29425,#29426,#29427,#29428,#29429,#29430,#29431,#29432,#29433,#29434,#29435,
#29436,#29437,#29438,#29439,#29440,#29441,#29442,#29443,#29444,#29445,#29446,
#29447,#29448,#29449,#29450,#29451,#29452,#29453,#29454,#29455,#29456,#29457,
#29458,#29459,#29460,#29461,#29462,#29463,#29464,#29465,#29466,#29467,#29468,
#29469,#29470,#29471,#29472,#29473,#29474,#29475,#29476,#29477,#29478,#29479,
#29480,#29481,#29482,#29483,#29484,#29485,#29486,#29487,#29488,#29489,#29490,
#29491,#29492,#29493,#29494,#29495,#29496,#29497,#29498,#29499,#29500,#29501,
#29502,#29503,#29504,#29505,#29506,#29507,#29508,#29509,#29510,#29511,#29512,
#29513,#29514,#29515,#29516,#29517,#29518,#29519,#29520,#29521,#29522,#29523,
#29524,#29525,#29526,#29527,#29528,#29529,#29530,#29531,#29532,#29533,#29534,
#29535,#29536,#29537,#29538,#29539,#29540,#29541,#29542,#29543,#29544,#29545,
#29546,#29547,#29548,#29549,#29550,#29551,#29552,#29553,#29554,#29555,#29556,
#29557,#29558,#29559,#29560,#29561,#29562,#29563,#29564,#29565,#29566,#29567,
#29568,#29569,#29570,#29571,#29572,#29573,#29574,#29575),.UNSPECIFIED.,
 .F.,.F.,(4,2,2,2,2,2,2,2,2,2,2,2,2,2,2,2,2,2,2,2,2,2,2,2,2,2,2,2,2,2,2,
2,2,2,2,2,2,2,2,2,2,2,2,2,2,2,2,2,2,2,2,2,2,2,2,2,2,2,2,2,2,2,2,2,2,2,2,
2,2,2,2,2,2,2,2,2,2,2,2,2,2,2,2,2,2,2,2,2,2,2,2,2,2,2,2,2,2,2,2,4),(9.99999999815765E-7,
0.00248984042910974,0.00561629617446753,0.0121505941808296,0.0438670508689377,
0.0636585190425291,0.0732302639569316,0.0758178509753012,0.077398537873236,
0.0788665251219267,0.08100030653153,0.0862126925358243,0.129907811692407,
0.141218827496,0.149251312086533,0.152742148855637,0.155342482793766,0.15811933761236,
0.162508433617683,0.176408600881536,0.207278298350196,0.225317859375305,
0.229432767972491,0.231321325149154,0.232765166695651,0.234459828153989,
0.237510479782257,0.254272786683191,0.262028243731876,0.281367431819593,
0.294532997169395,0.303498302270635,0.307135984844374,0.30975812507255,
0.312480066164869,0.316623123308372,0.32834715694087,0.364471526036297,
0.380291775425887,0.384158484259675,0.385999655135213,0.387301916129383,
0.388973360713079,0.391915906101928,0.405858359578526,0.429859743425932,
0.453147683202867,0.459406094113763,0.462573915587413,0.465135685236222,
0.468085519691301,0.473144478384027,0.501090709371585,0.521197818454051,
0.53636743591904,0.539302624890517,0.540955700493059,0.542408832475035,
0.544336594881267,0.548611971336903,0.571807280426291,0.592595049163689,
0.610579334485302,0.615178136700596,0.617999412220788,0.620582974606797,
0.623908305821585,0.629473657635745,0.665762139295943,0.682938890144216,
0.691756005977596,0.694268762485516,0.695828724746857,0.697301533320525,
0.699125290134432,0.703657331174639,0.748249961533015,0.75961599685998,
0.767677212752748,0.771171716058845,0.773771451873097,0.77620897017638,
0.780277868989691,0.791420660087405,0.82814652339523,0.844065228409776,
0.847944836739026,0.849789541995181,0.851092821102683,0.852763168663429,
0.855701021110849,0.869548363739972,0.89361605863966,0.919124215601457,
0.92410332658099,0.92700652159823,0.929572811348499,0.932805875765826,0.939183891755464,
0.971367835775262),.UNSPECIFIED.);
#335=B_SPLINE_CURVE_WITH_KNOTS('',3,(#29576,#29577,#29578,#29579,#29580,
#29581,#29582,#29583,#29584,#29585,#29586,#29587,#29588,#29589,#29590,#29591,
#29592,#29593,#29594,#29595,#29596,#29597,#29598,#29599,#29600,#29601,#29602,
#29603,#29604,#29605,#29606,#29607,#29608,#29609,#29610,#29611,#29612,#29613,
#29614,#29615,#29616,#29617,#29618,#29619,#29620,#29621,#29622,#29623,#29624,
#29625,#29626,#29627,#29628,#29629,#29630,#29631,#29632,#29633,#29634,#29635,
#29636,#29637,#29638,#29639,#29640,#29641,#29642,#29643,#29644,#29645,#29646,
#29647,#29648,#29649,#29650,#29651,#29652,#29653,#29654,#29655,#29656,#29657,
#29658,#29659,#29660,#29661,#29662,#29663,#29664,#29665,#29666,#29667,#29668,
#29669,#29670,#29671,#29672,#29673,#29674,#29675,#29676,#29677,#29678,#29679,
#29680,#29681,#29682,#29683,#29684,#29685,#29686,#29687,#29688,#29689,#29690,
#29691,#29692,#29693,#29694,#29695,#29696,#29697,#29698,#29699,#29700,#29701,
#29702,#29703,#29704,#29705,#29706,#29707,#29708,#29709,#29710,#29711,#29712,
#29713,#29714,#29715,#29716,#29717,#29718,#29719,#29720,#29721,#29722,#29723,
#29724,#29725,#29726,#29727,#29728,#29729,#29730,#29731,#29732,#29733,#29734,
#29735,#29736,#29737,#29738,#29739,#29740,#29741,#29742,#29743,#29744,#29745,
#29746,#29747,#29748,#29749,#29750,#29751,#29752,#29753,#29754,#29755,#29756,
#29757,#29758,#29759,#29760,#29761,#29762,#29763,#29764,#29765,#29766,#29767,
#29768,#29769,#29770,#29771,#29772,#29773,#29774,#29775,#29776,#29777),
 .UNSPECIFIED.,.F.,.F.,(4,2,2,2,2,2,2,2,2,2,2,2,2,2,2,2,2,2,2,2,2,2,2,2,
2,2,2,2,2,2,2,2,2,2,2,2,2,2,2,2,2,2,2,2,2,2,2,2,2,2,2,2,2,2,2,2,2,2,2,2,
2,2,2,2,2,2,2,2,2,2,2,2,2,2,2,2,2,2,2,2,2,2,2,2,2,2,2,2,2,2,2,2,2,2,2,2,
2,2,2,2,4),(0.971346799428905,0.971393807723292,1.00248341395968,1.01353394040873,
1.01634507260716,1.01797506879581,1.01944139297462,1.02146845289682,1.02635989237911,
1.03353697284982,1.05784397528317,1.08664086907653,1.09167811617992,1.09462850001616,
1.09719882336612,1.10038783299113,1.10672505869199,1.1305881102961,1.1558491195431,
1.16802449405939,1.17090891968254,1.17255390322787,1.17401592605357,1.17601090279887,
1.18070182549438,1.18748175325983,1.20924226483471,1.23888227027299,1.24542305047163,
1.2486545037329,1.25123175338879,1.25416069957369,1.25921891469424,1.28695703721142,
1.31500785019909,1.32328028209969,1.32583578429263,1.32741103473521,1.32891094151386,
1.33109984015253,1.33701466447982,1.3463446509391,1.36734901133354,1.39560911445701,
1.40064758494378,1.40360463071679,1.40618467363479,1.40939112042748,1.41578264892817,
1.4400019745184,1.46593835726208,1.47718972238715,1.48001583436438,1.48164936741866,
1.48310707516813,1.48511120146793,1.48991414039928,1.49692632679696,1.52017464631029,
1.5480883158423,1.55467124583728,1.55789628881885,1.56045551001211,1.56334972438136,
1.56831028187733,1.59351167928391,1.60966700083135,1.63145055180715,1.6345771526172,
1.63628830128374,1.63773585107037,1.63961237947638,1.6436244231757,1.66060259999796,
1.69020088389503,1.70640405493955,1.71104625692704,1.71389500144778,1.71650470961001,
1.71992322841228,1.72742402960879,1.75269629251805,1.78351522487468,1.7883188449285,
1.79020759590426,1.79171760304882,1.79332027787656,1.79587382904581,1.80459989585764,
1.82143880069531,1.85626652138392,1.86181256634905,1.8652032056099,1.86783345108478,
1.87074782342507,1.87560101473461,1.89663034549709,1.92531077105376,1.93825773548782,
1.94103475003504,1.94279591973499),.UNSPECIFIED.);
#336=B_SPLINE_CURVE_WITH_KNOTS('',3,(#30118,#30119,#30120,#30121,#30122,
#30123,#30124,#30125,#30126,#30127,#30128,#30129,#30130,#30131,#30132,#30133,
#30134,#30135,#30136,#30137,#30138,#30139,#30140,#30141,#30142,#30143,#30144,
#30145),.UNSPECIFIED.,.F.,.F.,(4,3,3,3,3,3,3,3,3,4),(0.,0.0461567016013966,
0.10481637338886,0.141987909893012,0.148065501794539,0.187793278496004,
0.22417637037208,0.275733961853634,0.32759864266339,0.331419002748183),
 .UNSPECIFIED.);
#337=B_SPLINE_CURVE_WITH_KNOTS('',3,(#30486,#30487,#30488,#30489,#30490,
#30491,#30492,#30493,#30494,#30495,#30496,#30497,#30498,#30499,#30500,#30501,
#30502,#30503,#30504,#30505,#30506,#30507,#30508,#30509,#30510),
 .UNSPECIFIED.,.F.,.F.,(4,3,3,3,3,3,3,3,4),(0.,0.0451591013560227,0.0863053370931954,
0.114402431924666,0.128866540493028,0.15651567637735,0.208426240523224,
0.23219202465052,0.233592218228785),.UNSPECIFIED.);
#338=B_SPLINE_CURVE_WITH_KNOTS('',3,(#30515,#30516,#30517,#30518,#30519,
#30520,#30521),.UNSPECIFIED.,.F.,.F.,(4,3,4),(-0.0356563315348787,-0.0168385637965097,
-6.00712216046093E-6),.UNSPECIFIED.);
#339=B_SPLINE_CURVE_WITH_KNOTS('',3,(#30523,#30524,#30525,#30526),
 .UNSPECIFIED.,.F.,.F.,(4,4),(0.0706728850407956,0.0856518761238354),
 .UNSPECIFIED.);
#340=B_SPLINE_CURVE_WITH_KNOTS('',3,(#30528,#30529,#30530,#30531,#30532,
#30533),.UNSPECIFIED.,.F.,.F.,(4,2,4),(-0.0693808026657025,-0.0346741578608072,
-9.99911564922296E-7),.UNSPECIFIED.);
#341=B_SPLINE_CURVE_WITH_KNOTS('',3,(#30535,#30536,#30537,#30538,#30539,
#30540),.UNSPECIFIED.,.F.,.F.,(4,2,4),(0.220967788015232,0.232496868866944,
0.26115278337561),.UNSPECIFIED.);
#342=B_SPLINE_CURVE_WITH_KNOTS('',3,(#30541,#30542,#30543,#30544,#30545,
#30546,#30547,#30548,#30549,#30550,#30551,#30552,#30553,#30554,#30555,#30556,
#30557,#30558,#30559,#30560,#30561,#30562,#30563,#30564),.UNSPECIFIED.,
 .F.,.F.,(4,2,2,2,2,2,2,2,2,2,2,4),(-0.0545071100794137,-0.0346117647175132,
-0.0288940964902406,-0.027947926335196,-0.0276921717992136,-0.0275391564768281,
-0.0274029213244984,-0.0272315883107351,-0.0268910373658706,-0.02438570236167,
-0.0184895448929481,-0.000174302815414135),.UNSPECIFIED.);
#343=B_SPLINE_CURVE_WITH_KNOTS('',3,(#30566,#30567,#30568,#30569,#30570,
#30571),.UNSPECIFIED.,.F.,.F.,(4,2,4),(-0.0566586033688786,-0.0284132480267369,
-0.000146512503515223),.UNSPECIFIED.);
#344=B_SPLINE_CURVE_WITH_KNOTS('',3,(#30573,#30574,#30575,#30576,#30577,
#30578),.UNSPECIFIED.,.F.,.F.,(4,2,4),(0.296274329747878,0.305955146920116,
0.308739916339329),.UNSPECIFIED.);
#345=B_SPLINE_CURVE_WITH_KNOTS('',3,(#30580,#30581,#30582,#30583,#30584,
#30585,#30586),.UNSPECIFIED.,.F.,.F.,(4,3,4),(-0.0322922670327419,-0.0168989031257184,
0.),.UNSPECIFIED.);
#346=B_SPLINE_CURVE_WITH_KNOTS('',3,(#30590,#30591,#30592,#30593,#30594,
#30595),.UNSPECIFIED.,.F.,.F.,(4,2,4),(-0.0526090819005489,-0.0263046029830051,
-9.9999999843628E-7),.UNSPECIFIED.);
#347=B_SPLINE_CURVE_WITH_KNOTS('',3,(#30599,#30600,#30601,#30602,#30603,
#30604,#30605,#30606),.UNSPECIFIED.,.F.,.F.,(4,2,2,4),(-0.0944036996742436,
-0.0771433030461012,-0.0485319215546893,0.),.UNSPECIFIED.);
#348=B_SPLINE_CURVE_WITH_KNOTS('',3,(#30610,#30611,#30612,#30613,#30614,
#30615,#30616),.UNSPECIFIED.,.F.,.F.,(4,3,4),(-0.0357121223372438,-0.0174889920223166,
0.),.UNSPECIFIED.);
#349=B_SPLINE_CURVE_WITH_KNOTS('',3,(#30618,#30619,#30620,#30621),
 .UNSPECIFIED.,.F.,.F.,(4,4),(0.,0.997468283692927),.UNSPECIFIED.);
#350=B_SPLINE_CURVE_WITH_KNOTS('',3,(#30622,#30623,#30624,#30625,#30626,
#30627,#30628,#30629,#30630,#30631,#30632,#30633,#30634,#30635,#30636,#30637,
#30638,#30639,#30640,#30641,#30642,#30643,#30644,#30645,#30646,#30647,#30648,
#30649),.UNSPECIFIED.,.F.,.F.,(4,2,2,2,2,2,2,2,2,2,2,2,2,4),(-0.125771117028632,
-0.0864552223641016,-0.0678485902550579,-0.0594428399644161,-0.0575924114249427,
-0.0571183863442095,-0.0568468165768063,-0.0566394520287764,-0.0563729061938286,
-0.0559085649950657,-0.0539526314959845,-0.0456980560831236,-0.0292561698449011,
0.),.UNSPECIFIED.);
#351=B_SPLINE_CURVE_WITH_KNOTS('',3,(#30651,#30652,#30653,#30654,#30655,
#30656,#30657),.UNSPECIFIED.,.F.,.F.,(4,3,4),(-0.0385164580871794,-0.0188401674254162,
0.),.UNSPECIFIED.);
#352=B_SPLINE_CURVE_WITH_KNOTS('',3,(#30661,#30662,#30663,#30664,#30665,
#30666,#30667),.UNSPECIFIED.,.F.,.F.,(4,3,4),(-0.0626263501111082,-0.0313079089847344,
-0.000161268437901824),.UNSPECIFIED.);
#353=B_SPLINE_CURVE_WITH_KNOTS('',3,(#30669,#30670,#30671,#30672),
 .UNSPECIFIED.,.F.,.F.,(4,4),(0.754529901247614,0.766860984898717),
 .UNSPECIFIED.);
#354=B_SPLINE_CURVE_WITH_KNOTS('',3,(#30674,#30675,#30676,#30677,#30678,
#30679,#30680),.UNSPECIFIED.,.F.,.F.,(4,3,4),(-0.0311458227321188,-0.0161494601786653,
0.),.UNSPECIFIED.);
#355=B_SPLINE_CURVE_WITH_KNOTS('',3,(#30965,#30966,#30967,#30968,#30969,
#30970,#30971,#30972,#30973,#30974,#30975,#30976,#30977,#30978,#30979,#30980,
#30981,#30982,#30983,#30984,#30985,#30986,#30987,#30988,#30989,#30990,#30991,
#30992,#30993,#30994,#30995,#30996,#30997,#30998,#30999,#31000,#31001,#31002,
#31003,#31004,#31005,#31006,#31007,#31008,#31009,#31010,#31011,#31012,#31013),
 .UNSPECIFIED.,.F.,.F.,(4,3,3,3,3,3,3,3,3,3,3,3,3,3,3,3,4),(-0.503648702838972,
-0.478239118516134,-0.425663343805114,-0.419651033765898,-0.414757025337115,
-0.360029409919934,-0.345036067010815,-0.332450646380526,-0.328029406469616,
-0.242050926335671,-0.24008266664698,-0.222356647888336,-0.119796523329524,
-0.115154566521774,-0.11055320579857,-0.0210267271158198,-3.70377469171095E-5),
 .UNSPECIFIED.);
#356=B_SPLINE_CURVE_WITH_KNOTS('',3,(#31015,#31016,#31017,#31018,#31019,
#31020,#31021,#31022,#31023,#31024,#31025,#31026,#31027),.UNSPECIFIED.,
 .F.,.F.,(4,3,3,3,4),(0.,0.304030668972893,0.5,0.804030668972894,0.999999999999386),
 .UNSPECIFIED.);
#357=B_SPLINE_CURVE_WITH_KNOTS('',3,(#31029,#31030,#31031,#31032,#31033,
#31034,#31035,#31036,#31037,#31038,#31039,#31040,#31041,#31042,#31043,#31044,
#31045,#31046,#31047,#31048,#31049,#31050,#31051,#31052,#31053,#31054,#31055,
#31056,#31057,#31058,#31059,#31060,#31061,#31062,#31063,#31064,#31065,#31066,
#31067,#31068,#31069,#31070,#31071,#31072,#31073,#31074,#31075,#31076,#31077),
 .UNSPECIFIED.,.F.,.F.,(4,3,3,3,3,3,3,3,3,3,3,3,3,3,3,3,4),(0.,0.0886407066381885,
0.125,0.212008098936426,0.25,0.337329846599543,0.375,0.462313411756197,
0.5,0.587313411756187,0.625,0.712329846599542,0.75,0.837008098936432,0.875,
0.963640706638148,1.),.UNSPECIFIED.);
#358=B_SPLINE_CURVE_WITH_KNOTS('',3,(#31079,#31080,#31081,#31082,#31083,
#31084,#31085,#31086,#31087,#31088,#31089,#31090,#31091,#31092,#31093,#31094,
#31095,#31096,#31097,#31098,#31099,#31100,#31101,#31102,#31103,#31104,#31105,
#31106,#31107,#31108,#31109,#31110,#31111,#31112,#31113,#31114,#31115,#31116,
#31117,#31118,#31119,#31120,#31121,#31122,#31123,#31124,#31125,#31126,#31127),
 .UNSPECIFIED.,.F.,.F.,(4,3,3,3,3,3,3,3,3,3,3,3,3,3,3,3,4),(0.,0.0886171082475257,
0.125,0.211984138088812,0.25,0.337305893446915,0.375,0.46228950097559,0.5,
0.587289500975586,0.625,0.712305893446908,0.75,0.836984138088813,0.875,
0.963617108247523,1.),.UNSPECIFIED.);
#359=B_SPLINE_CURVE_WITH_KNOTS('',3,(#31129,#31130,#31131,#31132,#31133,
#31134,#31135,#31136,#31137,#31138,#31139,#31140,#31141,#31142,#31143,#31144,
#31145,#31146,#31147,#31148,#31149,#31150,#31151,#31152,#31153,#31154,#31155,
#31156,#31157,#31158,#31159,#31160,#31161,#31162,#31163,#31164,#31165,#31166,
#31167,#31168,#31169,#31170,#31171,#31172,#31173,#31174,#31175,#31176,#31177),
 .UNSPECIFIED.,.F.,.F.,(4,3,3,3,3,3,3,3,3,3,3,3,3,3,3,3,4),(0.,0.088620284495184,
0.125,0.211987363129608,0.25,0.337309117454998,0.375,0.462292719277718,
0.5,0.587292719277716,0.625,0.712309117455,0.75,0.836987363129601,0.875,
0.963620284495189,1.),.UNSPECIFIED.);
#360=B_SPLINE_CURVE_WITH_KNOTS('',3,(#31179,#31180,#31181,#31182,#31183,
#31184,#31185,#31186,#31187,#31188,#31189,#31190,#31191,#31192,#31193,#31194,
#31195,#31196,#31197,#31198,#31199,#31200,#31201,#31202,#31203,#31204,#31205,
#31206,#31207,#31208,#31209,#31210,#31211,#31212,#31213,#31214,#31215,#31216,
#31217,#31218,#31219,#31220,#31221,#31222,#31223,#31224,#31225,#31226,#31227),
 .UNSPECIFIED.,.F.,.F.,(4,3,3,3,3,3,3,3,3,3,3,3,3,3,3,3,4),(0.,0.0886382763954242,
0.125,0.212005631372845,0.25,0.337327379830824,0.375,0.462310949348795,
0.5,0.587310949348818,0.625,0.712327379830809,0.75,0.837005631372844,0.875,
0.963638276395463,1.),.UNSPECIFIED.);
#361=B_SPLINE_CURVE_WITH_KNOTS('',3,(#31229,#31230,#31231,#31232,#31233,
#31234,#31235,#31236,#31237,#31238,#31239,#31240,#31241,#31242,#31243,#31244,
#31245,#31246,#31247,#31248,#31249,#31250,#31251,#31252,#31253,#31254,#31255,
#31256,#31257,#31258,#31259,#31260,#31261,#31262,#31263,#31264,#31265,#31266,
#31267,#31268,#31269,#31270,#31271,#31272,#31273,#31274,#31275,#31276,#31277),
 .UNSPECIFIED.,.F.,.F.,(4,3,3,3,3,3,3,3,3,3,3,3,3,3,3,3,4),(0.,0.0886104150389065,
0.125,0.211978952212712,0.25,0.337305502283307,0.375,0.462245050243597,
0.5,0.587333772189201,0.625,0.712305979497255,0.75,0.836989031823058,0.875,
0.96362351292812,1.),.UNSPECIFIED.);
#362=B_SPLINE_CURVE_WITH_KNOTS('',3,(#31279,#31280,#31281,#31282,#31283,
#31284,#31285,#31286,#31287,#31288,#31289,#31290,#31291,#31292,#31293,#31294,
#31295,#31296,#31297,#31298,#31299,#31300,#31301,#31302,#31303,#31304,#31305,
#31306,#31307,#31308,#31309,#31310,#31311,#31312,#31313,#31314,#31315,#31316,
#31317,#31318,#31319,#31320,#31321,#31322,#31323,#31324,#31325,#31326,#31327),
 .UNSPECIFIED.,.F.,.F.,(4,3,3,3,3,3,3,3,3,3,3,3,3,3,3,3,4),(0.,0.0886243992808492,
0.125,0.211991541122404,0.25,0.337313294108582,0.375,0.462296888540609,
0.5,0.587296888540603,0.625,0.712313294108576,0.75,0.836991541122409,0.875,
0.96362439928086,1.),.UNSPECIFIED.);
#363=B_SPLINE_CURVE_WITH_KNOTS('',3,(#31329,#31330,#31331,#31332,#31333,
#31334,#31335,#31336,#31337,#31338,#31339,#31340,#31341,#31342,#31343,#31344,
#31345,#31346,#31347,#31348,#31349,#31350,#31351,#31352,#31353,#31354,#31355,
#31356,#31357,#31358,#31359,#31360,#31361,#31362,#31363,#31364,#31365,#31366,
#31367,#31368,#31369,#31370,#31371,#31372,#31373,#31374,#31375,#31376,#31377),
 .UNSPECIFIED.,.F.,.F.,(4,3,3,3,3,3,3,3,3,3,3,3,3,3,3,3,4),(0.,0.0886329632205807,
0.125,0.212000236599526,0.25,0.337321986793343,0.375,0.462305565848219,
0.5,0.587305565848244,0.625,0.712321986793333,0.75,0.83700023659952,0.875,
0.963632963220574,1.),.UNSPECIFIED.);
#364=B_SPLINE_CURVE_WITH_KNOTS('',3,(#31379,#31380,#31381,#31382,#31383,
#31384,#31385,#31386,#31387,#31388,#31389,#31390,#31391,#31392,#31393,#31394,
#31395,#31396,#31397,#31398,#31399,#31400,#31401,#31402,#31403,#31404,#31405,
#31406,#31407,#31408,#31409,#31410,#31411,#31412,#31413,#31414,#31415,#31416,
#31417,#31418,#31419,#31420,#31421,#31422,#31423,#31424,#31425,#31426,#31427,
#31428,#31429,#31430,#31431,#31432,#31433,#31434,#31435,#31436,#31437,#31438,
#31439,#31440,#31441,#31442,#31443,#31444,#31445,#31446,#31447,#31448,#31449,
#31450,#31451,#31452,#31453,#31454,#31455,#31456,#31457),.UNSPECIFIED.,
 .F.,.F.,(4,3,3,3,3,3,3,3,3,3,3,3,3,3,3,3,3,3,3,3,3,3,3,3,3,3,4),(0.,0.0888061128071974,
0.103629824354861,0.125,0.211608444540927,0.25,0.261105648823599,0.337106991491099,
0.375,0.418504729011411,0.4375,0.46875,0.484375,0.5,0.515625,0.53125,0.5625,
0.592028433976737,0.625,0.6875,0.75,0.760059091463865,0.831314636644941,
0.875,0.907035057496371,0.948814674685162,1.),.UNSPECIFIED.);
#365=B_SPLINE_CURVE_WITH_KNOTS('',3,(#31459,#31460,#31461,#31462,#31463,
#31464,#31465,#31466,#31467,#31468,#31469,#31470,#31471,#31472,#31473,#31474,
#31475,#31476,#31477,#31478,#31479,#31480,#31481,#31482,#31483,#31484,#31485,
#31486,#31487,#31488,#31489,#31490,#31491,#31492,#31493,#31494,#31495,#31496,
#31497,#31498,#31499,#31500,#31501,#31502,#31503,#31504,#31505,#31506,#31507),
 .UNSPECIFIED.,.F.,.F.,(4,3,3,3,3,3,3,3,3,3,3,3,3,3,3,3,4),(0.,0.0886284882868581,
0.125,0.211995692935443,0.25,0.337317444589203,0.375,0.462301031678349,
0.5,0.587301031678344,0.625,0.712317444589205,0.75,0.836995692935444,0.875,
0.963628488286822,1.),.UNSPECIFIED.);
#366=B_SPLINE_CURVE_WITH_KNOTS('',3,(#31508,#31509,#31510,#31511,#31512,
#31513,#31514,#31515,#31516,#31517,#31518,#31519,#31520,#31521,#31522,#31523,
#31524,#31525,#31526,#31527,#31528,#31529,#31530,#31531,#31532,#31533,#31534,
#31535,#31536,#31537,#31538,#31539,#31540,#31541,#31542,#31543,#31544,#31545,
#31546,#31547,#31548,#31549,#31550,#31551,#31552,#31553,#31554,#31555,#31556),
 .UNSPECIFIED.,.F.,.F.,(4,3,3,3,3,3,3,3,3,3,3,3,3,3,3,3,4),(0.,0.109960626274433,
0.125,0.233606518241178,0.25,0.358908048100772,0.375,0.483868300041721,
0.5,0.608868300041721,0.625,0.733908048100777,0.75,0.858606518241174,0.875,
0.984960626274394,1.),.UNSPECIFIED.);
#367=B_SPLINE_CURVE_WITH_KNOTS('',3,(#31834,#31835,#31836,#31837,#31838,
#31839,#31840,#31841,#31842,#31843,#31844,#31845,#31846,#31847,#31848,#31849,
#31850,#31851,#31852,#31853,#31854,#31855,#31856,#31857,#31858,#31859,#31860,
#31861,#31862,#31863,#31864,#31865,#31866,#31867,#31868,#31869,#31870,#31871,
#31872,#31873,#31874,#31875,#31876,#31877,#31878,#31879,#31880,#31881,#31882),
 .UNSPECIFIED.,.F.,.F.,(4,3,3,3,3,3,3,3,3,3,3,3,3,3,3,3,4),(-0.501724005229533,
-0.472416574319748,-0.414389357077405,-0.407358038783487,-0.400886943772423,
-0.314043010674865,-0.309619504665006,-0.305251689160703,-0.222333474861526,
-0.217225768055783,-0.208375447427435,-0.203501118200736,-0.199345077371566,
-0.101201676292347,-0.096184718783614,-0.017180163401669,0.),
 .UNSPECIFIED.);
#368=B_SPLINE_CURVE_WITH_KNOTS('',3,(#31884,#31885,#31886,#31887,#31888,
#31889,#31890,#31891,#31892,#31893,#31894,#31895,#31896,#31897,#31898,#31899,
#31900,#31901,#31902,#31903,#31904,#31905,#31906,#31907,#31908),
 .UNSPECIFIED.,.F.,.F.,(4,3,3,3,3,3,3,3,4),(0.,0.172429158239796,0.25,0.41907286168834,
0.5,0.669072861688337,0.75,0.922429158239836,0.999999999999765),
 .UNSPECIFIED.);
#369=B_SPLINE_CURVE_WITH_KNOTS('',3,(#31910,#31911,#31912,#31913,#31914,
#31915,#31916,#31917,#31918,#31919,#31920,#31921,#31922,#31923,#31924,#31925,
#31926,#31927,#31928,#31929,#31930,#31931,#31932,#31933,#31934,#31935,#31936,
#31937,#31938,#31939,#31940,#31941,#31942,#31943,#31944,#31945,#31946,#31947,
#31948,#31949,#31950,#31951,#31952,#31953,#31954,#31955,#31956,#31957,#31958,
#31959,#31960,#31961,#31962,#31963,#31964,#31965,#31966,#31967,#31968,#31969,
#31970,#31971,#31972,#31973,#31974,#31975,#31976,#31977,#31978,#31979,#31980,
#31981,#31982,#31983,#31984,#31985,#31986,#31987,#31988,#31989,#31990,#31991,
#31992,#31993,#31994,#31995,#31996,#31997,#31998,#31999,#32000,#32001,#32002,
#32003,#32004,#32005,#32006,#32007,#32008,#32009,#32010,#32011,#32012,#32013,
#32014,#32015,#32016,#32017,#32018,#32019,#32020,#32021,#32022,#32023,#32024,
#32025,#32026,#32027,#32028,#32029,#32030,#32031,#32032,#32033,#32034,#32035,
#32036,#32037,#32038,#32039,#32040,#32041,#32042,#32043,#32044,#32045,#32046,
#32047,#32048,#32049,#32050,#32051,#32052,#32053,#32054,#32055,#32056,#32057,
#32058,#32059,#32060,#32061,#32062,#32063,#32064,#32065,#32066,#32067,#32068,
#32069,#32070,#32071,#32072,#32073,#32074,#32075,#32076,#32077,#32078,#32079,
#32080,#32081,#32082,#32083,#32084,#32085,#32086,#32087,#32088,#32089,#32090,
#32091,#32092,#32093,#32094,#32095,#32096,#32097,#32098,#32099,#32100,#32101,
#32102,#32103,#32104,#32105,#32106,#32107,#32108,#32109,#32110,#32111),
 .UNSPECIFIED.,.F.,.F.,(4,2,2,2,2,2,2,2,2,2,2,2,2,2,2,2,2,2,2,2,2,2,2,2,
2,2,2,2,2,2,2,2,2,2,2,2,2,2,2,2,2,2,2,2,2,2,2,2,2,2,2,2,2,2,2,2,2,2,2,2,
2,2,2,2,2,2,2,2,2,2,2,2,2,2,2,2,2,2,2,2,2,2,2,2,2,2,2,2,2,2,2,2,2,2,2,2,
2,2,2,2,4),(0.000124435018137221,0.01427599667095,0.0243402584564738,0.0301983218783695,
0.0358628192640442,0.0422528806565145,0.0523393192149522,0.0865312582670473,
0.136171966071755,0.160734773100723,0.170657187299706,0.178238857463452,
0.182210202789374,0.185547378691446,0.189861506823648,0.199464405494597,
0.258108251018683,0.311375935039054,0.323142446876579,0.329888503625282,
0.3358138160006,0.343259360311408,0.355110933842989,0.432903026416704,0.457832505183502,
0.472529140837405,0.477657541990267,0.481106345805127,0.484724116078588,
0.490657440458818,0.511293397342995,0.560725822381833,0.59403432898518,
0.608643282163014,0.620455708549381,0.627206506509566,0.633123230873407,
0.640540751689568,0.652311271688271,0.730499159782864,0.76401724395515,
0.772388244729275,0.776515381350157,0.779839988738716,0.784031102655559,
0.792726815870931,0.843911347931676,0.866563405595919,0.894661236322197,
0.9138157939059,0.92192335961171,0.927933113919541,0.934348506148276,0.944544647984111,
0.98350704921781,1.01906819990235,1.06052822829088,1.06941574992997,1.07364670922496,
1.07698254932194,1.0811015062499,1.08937175975122,1.12189836898887,1.20140338238339,
1.21282063103088,1.22014726103616,1.22607532585814,1.23293240138814,1.24518927319071,
1.28493904976871,1.34126667017682,1.36246187645625,1.36844893652607,1.37208155635995,
1.37550091354802,1.38055206013141,1.3948237395594,1.41869783627087,1.49959570793514,
1.51088580859953,1.51814116132588,1.52401511182766,1.53081150366052,1.54295879950415,
1.58227574527781,1.63299918458442,1.65952038956469,1.66588272908685,1.66958353729213,
1.67298028478349,1.67782785422248,1.69042829604107,1.74635120632815,1.79242737219772,
1.8081116244709,1.81564980836978,1.82160777711801,1.82834799265712,1.83538252057036,
1.85275364928988,1.88917416055493),.UNSPECIFIED.);
#370=B_SPLINE_CURVE_WITH_KNOTS('',3,(#32113,#32114,#32115,#32116,#32117,
#32118,#32119,#32120,#32121,#32122,#32123,#32124,#32125,#32126,#32127,#32128,
#32129,#32130,#32131,#32132,#32133,#32134,#32135,#32136,#32137,#32138,#32139,
#32140,#32141,#32142,#32143,#32144,#32145,#32146,#32147,#32148,#32149,#32150,
#32151,#32152,#32153,#32154,#32155,#32156,#32157,#32158,#32159,#32160,#32161,
#32162,#32163,#32164,#32165,#32166,#32167,#32168,#32169,#32170,#32171,#32172,
#32173,#32174,#32175,#32176,#32177,#32178,#32179,#32180,#32181,#32182,#32183,
#32184,#32185,#32186,#32187,#32188,#32189,#32190,#32191,#32192,#32193,#32194,
#32195,#32196,#32197,#32198,#32199,#32200,#32201,#32202,#32203,#32204,#32205,
#32206,#32207,#32208,#32209,#32210,#32211,#32212,#32213,#32214,#32215,#32216,
#32217,#32218,#32219,#32220,#32221,#32222,#32223,#32224,#32225,#32226,#32227,
#32228,#32229,#32230,#32231,#32232,#32233,#32234,#32235,#32236,#32237,#32238,
#32239,#32240,#32241,#32242,#32243,#32244,#32245,#32246,#32247,#32248,#32249,
#32250,#32251,#32252,#32253,#32254,#32255,#32256,#32257,#32258,#32259,#32260,
#32261,#32262,#32263,#32264,#32265,#32266,#32267,#32268,#32269,#32270,#32271,
#32272,#32273,#32274,#32275,#32276,#32277,#32278,#32279,#32280,#32281,#32282,
#32283,#32284,#32285,#32286,#32287,#32288,#32289,#32290,#32291,#32292,#32293,
#32294,#32295,#32296,#32297,#32298,#32299,#32300,#32301,#32302,#32303,#32304,
#32305,#32306,#32307,#32308,#32309,#32310,#32311,#32312,#32313,#32314,#32315,
#32316,#32317,#32318,#32319,#32320,#32321,#32322,#32323,#32324,#32325,#32326,
#32327,#32328,#32329,#32330,#32331,#32332,#32333,#32334,#32335,#32336,#32337,
#32338,#32339,#32340,#32341,#32342,#32343,#32344,#32345,#32346,#32347,#32348,
#32349,#32350,#32351,#32352,#32353,#32354,#32355,#32356,#32357,#32358,#32359,
#32360,#32361,#32362,#32363,#32364,#32365,#32366,#32367,#32368,#32369,#32370,
#32371,#32372,#32373,#32374,#32375,#32376,#32377,#32378,#32379,#32380,#32381,
#32382,#32383,#32384,#32385,#32386,#32387,#32388,#32389,#32390,#32391,#32392,
#32393,#32394,#32395,#32396,#32397,#32398,#32399,#32400,#32401,#32402,#32403,
#32404,#32405,#32406,#32407,#32408,#32409,#32410,#32411,#32412,#32413,#32414,
#32415,#32416,#32417,#32418,#32419,#32420,#32421,#32422,#32423,#32424,#32425,
#32426,#32427,#32428,#32429,#32430,#32431,#32432,#32433,#32434,#32435,#32436,
#32437,#32438,#32439,#32440,#32441,#32442,#32443,#32444,#32445,#32446,#32447,
#32448,#32449,#32450,#32451,#32452,#32453,#32454,#32455,#32456,#32457,#32458,
#32459,#32460,#32461,#32462,#32463,#32464,#32465,#32466,#32467,#32468,#32469,
#32470,#32471,#32472,#32473,#32474,#32475,#32476,#32477,#32478,#32479,#32480,
#32481,#32482,#32483,#32484,#32485,#32486,#32487,#32488,#32489,#32490,#32491,
#32492,#32493,#32494,#32495,#32496,#32497,#32498,#32499,#32500,#32501,#32502,
#32503,#32504,#32505,#32506,#32507,#32508,#32509,#32510,#32511,#32512,#32513,
#32514,#32515,#32516,#32517,#32518,#32519,#32520,#32521,#32522,#32523,#32524,
#32525,#32526,#32527,#32528,#32529,#32530,#32531,#32532,#32533,#32534,#32535,
#32536,#32537,#32538,#32539,#32540,#32541,#32542,#32543,#32544,#32545,#32546,
#32547,#32548,#32549,#32550,#32551,#32552,#32553,#32554,#32555,#32556,#32557,
#32558,#32559,#32560,#32561,#32562,#32563,#32564,#32565,#32566,#32567,#32568,
#32569,#32570,#32571,#32572,#32573,#32574,#32575,#32576,#32577,#32578,#32579,
#32580,#32581,#32582,#32583,#32584,#32585,#32586,#32587,#32588,#32589,#32590,
#32591,#32592,#32593,#32594,#32595,#32596,#32597,#32598,#32599,#32600,#32601,
#32602,#32603,#32604,#32605,#32606,#32607,#32608,#32609,#32610,#32611,#32612,
#32613,#32614,#32615,#32616,#32617,#32618,#32619,#32620,#32621,#32622,#32623,
#32624,#32625,#32626,#32627,#32628,#32629,#32630,#32631,#32632,#32633,#32634,
#32635,#32636,#32637,#32638,#32639,#32640,#32641,#32642,#32643,#32644,#32645,
#32646,#32647,#32648,#32649,#32650,#32651,#32652,#32653,#32654,#32655,#32656,
#32657,#32658,#32659,#32660,#32661,#32662,#32663,#32664,#32665,#32666,#32667,
#32668,#32669,#32670,#32671,#32672,#32673,#32674,#32675,#32676,#32677,#32678,
#32679,#32680,#32681,#32682,#32683,#32684,#32685,#32686,#32687,#32688,#32689,
#32690,#32691,#32692,#32693,#32694,#32695,#32696,#32697,#32698,#32699,#32700,
#32701,#32702,#32703,#32704,#32705,#32706,#32707,#32708,#32709,#32710,#32711,
#32712,#32713,#32714,#32715,#32716,#32717,#32718,#32719,#32720,#32721,#32722,
#32723,#32724,#32725,#32726,#32727,#32728,#32729,#32730,#32731,#32732,#32733,
#32734,#32735,#32736,#32737,#32738,#32739,#32740,#32741,#32742,#32743,#32744,
#32745,#32746,#32747,#32748,#32749,#32750,#32751,#32752,#32753,#32754,#32755,
#32756,#32757,#32758,#32759,#32760,#32761,#32762,#32763,#32764,#32765,#32766,
#32767,#32768,#32769,#32770,#32771,#32772,#32773,#32774,#32775,#32776,#32777,
#32778,#32779,#32780,#32781,#32782,#32783,#32784,#32785,#32786,#32787,#32788,
#32789,#32790,#32791,#32792,#32793,#32794,#32795,#32796,#32797,#32798,#32799,
#32800,#32801,#32802,#32803,#32804,#32805,#32806,#32807,#32808,#32809,#32810,
#32811,#32812,#32813,#32814,#32815,#32816,#32817,#32818,#32819,#32820,#32821,
#32822,#32823,#32824,#32825,#32826,#32827,#32828,#32829,#32830,#32831,#32832,
#32833,#32834,#32835,#32836,#32837,#32838,#32839,#32840,#32841,#32842,#32843,
#32844,#32845,#32846,#32847,#32848,#32849,#32850,#32851,#32852,#32853,#32854,
#32855,#32856,#32857,#32858,#32859,#32860,#32861,#32862,#32863,#32864,#32865,
#32866,#32867,#32868,#32869,#32870,#32871,#32872,#32873,#32874,#32875,#32876,
#32877,#32878,#32879,#32880,#32881,#32882,#32883,#32884,#32885,#32886,#32887,
#32888,#32889,#32890,#32891,#32892,#32893,#32894,#32895,#32896,#32897,#32898,
#32899,#32900,#32901,#32902,#32903,#32904,#32905,#32906,#32907,#32908,#32909,
#32910,#32911,#32912,#32913,#32914,#32915,#32916,#32917,#32918,#32919,#32920,
#32921,#32922,#32923,#32924,#32925,#32926,#32927,#32928,#32929,#32930,#32931,
#32932,#32933,#32934,#32935,#32936,#32937,#32938,#32939,#32940,#32941,#32942,
#32943,#32944,#32945,#32946,#32947,#32948,#32949,#32950,#32951,#32952,#32953,
#32954,#32955,#32956,#32957,#32958,#32959,#32960,#32961,#32962,#32963,#32964,
#32965,#32966,#32967,#32968,#32969,#32970,#32971,#32972,#32973,#32974,#32975,
#32976,#32977,#32978,#32979,#32980,#32981,#32982,#32983,#32984,#32985,#32986,
#32987,#32988,#32989,#32990,#32991,#32992,#32993,#32994,#32995,#32996,#32997,
#32998,#32999,#33000,#33001,#33002,#33003,#33004,#33005,#33006,#33007,#33008,
#33009,#33010,#33011,#33012,#33013,#33014,#33015,#33016,#33017,#33018,#33019,
#33020,#33021,#33022,#33023,#33024,#33025,#33026,#33027,#33028,#33029,#33030,
#33031,#33032,#33033,#33034,#33035,#33036,#33037,#33038,#33039,#33040,#33041,
#33042,#33043,#33044,#33045,#33046,#33047,#33048,#33049,#33050,#33051,#33052,
#33053,#33054,#33055,#33056,#33057,#33058,#33059,#33060,#33061,#33062,#33063,
#33064,#33065,#33066,#33067,#33068),.UNSPECIFIED.,.F.,.F.,(4,2,2,2,2,2,
2,2,2,2,2,2,2,2,2,2,2,2,2,2,2,2,2,2,2,2,2,2,2,2,2,2,2,2,2,2,2,2,2,2,2,2,
2,2,2,2,2,2,2,2,2,2,2,2,2,2,2,2,2,2,2,2,2,2,2,2,2,2,2,2,2,2,2,2,2,2,2,2,
2,2,2,2,2,2,2,2,2,2,2,2,2,2,2,2,2,2,2,2,2,2,2,2,2,2,2,2,2,2,2,2,2,2,2,2,
2,2,2,2,2,2,2,2,2,2,2,2,2,2,2,2,2,2,2,2,2,2,2,2,2,2,2,2,2,2,2,2,2,2,2,2,
2,2,2,2,2,2,2,2,2,2,2,2,2,2,2,2,2,2,2,2,2,2,2,2,2,2,2,2,2,2,2,2,2,2,2,2,
2,2,2,2,2,2,2,2,2,2,2,2,2,2,2,2,2,2,2,2,2,2,2,2,2,2,2,2,2,2,2,2,2,2,2,2,
2,2,2,2,2,2,2,2,2,2,2,2,2,2,2,2,2,2,2,2,2,2,2,2,2,2,2,2,2,2,2,2,2,2,2,2,
2,2,2,2,2,2,2,2,2,2,2,2,2,2,2,2,2,2,2,2,2,2,2,2,2,2,2,2,2,2,2,2,2,2,2,2,
2,2,2,2,2,2,2,2,2,2,2,2,2,2,2,2,2,2,2,2,2,2,2,2,2,2,2,2,2,2,2,2,2,2,2,2,
2,2,2,2,2,2,2,2,2,2,2,2,2,2,2,2,2,2,2,2,2,2,2,2,2,2,2,2,2,2,2,2,2,2,2,2,
2,2,2,2,2,2,2,2,2,2,2,2,2,2,2,2,2,2,2,2,2,2,2,2,2,2,2,2,2,2,2,2,2,2,2,2,
2,2,2,2,2,2,2,2,2,2,2,2,2,2,2,2,2,2,2,2,2,2,2,2,2,2,2,2,2,2,2,2,2,2,2,2,
2,2,2,2,2,2,2,2,2,2,2,2,2,2,2,2,2,2,2,2,2,2,2,2,2,2,2,2,2,2,2,2,2,2,2,2,
2,2,2,4),(-9.44801459109388,-9.38140150084239,-9.34815307375884,-9.3397733122265,
-9.33561663537882,-9.33225378008983,-9.32799071259287,-9.31905658329978,
-9.27397782766007,-9.24605993230467,-9.20678224637513,-9.1945529386011,
-9.18766664830278,-9.18168688299225,-9.17426078843188,-9.16261390842311,
-9.08368022309558,-9.05927549305772,-9.04475201202775,-9.03961331655339,
-9.03613604670442,-9.03245759347394,-9.02637064532016,-9.00451019539947,
-8.93588411286869,-8.90434566150039,-8.89466860785615,-8.88831729461598,
-8.88224542535717,-8.8736928858359,-8.85332759114986,-8.78310118949654,
-8.76072151462188,-8.74701110333882,-8.74197976410823,-8.73852235435341,
-8.73480741534788,-8.72855242072028,-8.7046364214805,-8.65755567876359,
-8.62521788113793,-8.60412035295504,-8.59566826595096,-8.58955328469147,
-8.58391982570317,-8.57469917726005,-8.54986049164039,-8.47731845713547,
-8.46014871667201,-8.44873949200216,-8.44404703344266,-8.44064512482223,
-8.43678423638304,-8.43003418547347,-8.39194149309516,-8.33738491019732,
-8.30878024248757,-8.29939356560362,-8.2931015766456,-8.28698928792847,
-8.27820980996388,-8.25642512952648,-8.19370446365244,-8.1585501145342,
-8.14995636697368,-8.14575783055956,-8.14239510702805,-8.13817473266887,
-8.12946754333187,-8.07793054335651,-8.01670043505502,-8.00452596885187,
-7.99765056798857,-7.99166898523602,-7.98422592414056,-7.97252247708097,
-7.8938738263871,-7.86066075349899,-7.85228450469096,-7.8481280819492,-7.8447645565344,
-7.84049944600987,-7.83155709452065,-7.78904103073035,-7.75156723620115,
-7.72734503233419,-7.71006411934689,-7.7022162165618,-7.69619298907036,
-7.68955971441796,-7.67854030273919,-7.62740450201838,-7.59040136208314,
-7.56980758607235,-7.55685046786673,-7.55192439245928,-7.54848575170843,
-7.54473104830477,-7.53829327360408,-7.51155731942445,-7.44749720694638,
-7.41677671628374,-7.407177054837,-7.40084179059471,-7.39476012119845,-7.38615071257267,
-7.36539298548847,-7.3016527453641,-7.26614649689816,-7.2575143071448,-7.25330835823292,
-7.24994567168884,-7.24573282343006,-7.23706475751706,-7.18359426703734,
-7.12419443906607,-7.11204523107344,-7.10517513772245,-7.0991931209321,
-7.09174292611686,-7.08001483595798,-7.00149021910906,-6.96821193010324,
-6.95982827081709,-6.95567044196668,-6.95230699996828,-6.94804354564547,
-6.93910985791524,-6.89721235634368,-6.86145789766708,-6.83588214896809,
-6.81791848298812,-6.80995505538576,-6.80391646931734,-6.79733806475074,
-6.78657801810568,-6.7431633551587,-6.68926937411523,-6.66657169756683,
-6.66060724504058,-6.65695546532664,-6.65350227022196,-6.64831075722368,
-6.63451424289507,-6.57387958106604,-6.54232854957359,-6.52157245422814,
-6.51317015182879,-6.50706337703936,-6.50141822384321,-6.49213377339782,
-6.46678587097665,-6.3948183166293,-6.37769227248631,-6.36630353578805,
-6.361614120516,-6.35821242681708,-6.35434947101118,-6.34759097047796,-6.30851126663551,
-6.25471179875971,-6.23564945629639,-6.22115493142345,-6.21381420632902,
-6.20783850025273,-6.20088439296461,-6.18867362680956,-6.11716012429545,
-6.08701174843069,-6.07039559609442,-6.06500366536181,-6.06147523455011,
-6.05830466409053,-6.05295693064295,-6.03804938684816,-5.97815387171798,
-5.94704609230536,-5.92648511437095,-5.91811172397377,-5.91200976675774,
-5.90635779694922,-5.89703580185859,-5.87137147078792,-5.79975667049674,
-5.78265802182167,-5.77128223173348,-5.76659484406917,-5.76319339893564,
-5.75932931137846,-5.75256588712318,-5.71199701004625,-5.66088844554639,
-5.64119845058641,-5.62634876688777,-5.61894010707252,-5.61296037015986,
-5.60605860238916,-5.59408810099918,-5.5207853909241,-5.49158442404803,
-5.47529285464654,-5.46993787466782,-5.46641704496184,-5.46323965003657,
-5.4578556422307,-5.44267823903434,-5.38295500572268,-5.35195446670996,
-5.33144085523658,-5.32307442667898,-5.31697353927857,-5.31131976938189,
-5.30198826430322,-5.27624267865937,-5.20471613540599,-5.18762418430387,
-5.17625150321997,-5.17156455165107,-5.16816311014979,-5.16429866479983,
-5.15753386009215,-5.11662493523327,-5.06421146559669,-5.04538448250777,
-5.03102419215982,-5.02370920671893,-5.01773455639421,-5.01075913091909,
-4.99845089379714,-4.92769225407288,-4.8971317583695,-4.88037652093655,
-4.87496884510086,-4.87143705739459,-4.86826914425481,-4.86293608995139,
-4.84813733285144,-4.77216866854091,-4.73955944340199,-4.72978541974077,
-4.72341409763979,-4.71728508030098,-4.70875355879654,-4.68710543773134,
-4.65347547499122,-4.60315876849961,-4.58379643505322,-4.57793785359249,
-4.57430924445518,-4.57079841284659,-4.56549110081198,-4.54960587936143,
-4.52155682535197,-4.45132434035121,-4.4363506246857,-4.42891887753103,
-4.4229380604913,-4.4160543904857,-4.40384010853783,-4.36467212114955,-4.33757975952056,
-4.29152906339711,-4.28263734796421,-4.27838200487283,-4.27501897262567,
-4.27085422934785,-4.26243422825157,-4.22883404607388,-4.15087278503415,
-4.13902768490065,-4.13154376510978,-4.12555963179594,-4.11871426639979,
-4.1066821864288,-4.05578402163054,-4.0009557887622,-3.9873789719632,-3.98222032925095,
-3.97877386492966,-3.97511298574257,-3.96910482641362,-3.94582884713075,
-3.88872202696743,-3.848807165819,-3.83822590455367,-3.83168611880757,-3.82563652149612,
-3.81758907639446,-3.79910978651272,-3.77248623293831,-3.73750593573787,
-3.69336144107036,-3.68655143702741,-3.68267747448146,-3.67927966221325,
-3.67461386659972,-3.66336877846622,-3.6465415708106,-3.57824420478216,
-3.54951724535958,-3.53986461136127,-3.53351924490027,-3.52737604181771,
-3.5187592475767,-3.4964954449991,-3.46136771442216,-3.40722855515764,-3.39283293567694,
-3.38755669924319,-3.38439992223998,-3.38085669982481,-3.37539096646288,
-3.35809885988307,-3.32589683547393,-3.25803333672706,-3.24650315445813,
-3.23911162051876,-3.23313458114653,-3.22622357528891,-3.21387288832576,
-3.17374093045621,-3.14625463864198,-3.10190993516612,-3.09296845260623,
-3.08870425603886,-3.08534170708683,-3.08118683093758,-3.07281463652837,
-3.0396247106185,-2.96091840573627,-2.94922660990018,-2.94178820740471,
-2.93580862945455,-2.92893362897039,-2.91675458596445,-2.87781625765677,
-2.85362489022765,-2.80429910656731,-2.79548804678734,-2.791248784751,-2.7878870466656,
-2.78370969121696,-2.77522088521722,-2.74099827724974,-2.68093558388414,
-2.65633628424758,-2.64714864811203,-2.64152244101963,-2.63540537762009,
-2.62693187525845,-2.60567330503028,-2.57295712586263,-2.52488226036302,
-2.5024526591567,-2.49630814054109,-2.49261812789441,-2.48914957546455,
-2.48405241078808,-2.46984039298301,-2.44621771852627,-2.36533814786787,
-2.35300527788872,-2.34602679532548,-2.34005569729569,-2.33275281606529,
-2.31844241759414,-2.29970098142884,-2.24773828191848,-2.20634305381292,
-2.19958037884252,-2.1957176834768,-2.1923182087446,-2.18763450888408,-2.17627250123387,
-2.15919774392155,-2.08786671937614,-2.06196055820317,-2.05261416807905,
-2.0469599235255,-2.04086504318408,-2.03251865515358,-2.0121182842402,-1.9813665842259,
-1.92209006676937,-1.90635033768349,-1.90089509969131,-1.89770548156087,
-1.89420153180413,-1.88892224122803,-1.87325821023931,-1.84581628823902,
-1.7779310930747,-1.76088496037318,-1.75316391812636,-1.74714289100281,
-1.74051779870824,-1.72952574448648,-1.67165027446578,-1.6141137366604,
-1.60578913268532,-1.6016441560872,-1.59828212067461,-1.59400905741946,
-1.58501730969047,-1.54605340165214,-1.47257568502694,-1.46063697916326,
-1.45374472712599,-1.44776810455151,-1.44035666446211,-1.42547761252992,
-1.36383569034388,-1.31769839126718,-1.30876141342307,-1.30449875439695,
-1.30113711310382,-1.29698298072558,-1.28861115290025,-1.25541379557153,
-1.17675951780695,-1.16506465118156,-1.15762642659685,-1.15164831619072,
-1.1447764563489,-1.13260695447519,-1.07114764691721,-1.01998875394796,
-1.01126783577167,-1.00704633184975,-1.00368552697631,-0.999492905686176,
-0.990922316997083,-0.95595380282485,-0.893758691458273,-0.871447710955773,
-0.862589745951792,-0.856465552584371,-0.850196610590019,-0.840912099766564,
-0.813222167364056,-0.762074718227652,-0.719620316011767,-0.712849558430266,
-0.708985404786666,-0.705586979035008,-0.700907877600257,-0.689571979762603,
-0.672551191841519,-0.601874583043717,-0.575384033983162,-0.565975182833617,
-0.559681425272963,-0.553505877243141,-0.544701971239021,-0.521027315710591,
-0.482266905632647,-0.424787365560533,-0.41646037122685,-0.412315325640752,
-0.408953848625948,-0.404682273267573,-0.395696257012272,-0.356781239752759,
-0.283234093652927,-0.271314841183368,-0.26442753019634,-0.258451515623989,
-0.251036066172714,-0.23613196988513,-0.174482232466516,-0.128424436005239,
-0.11948157411596,-0.115218218598217,-0.111857080207177,-0.107704873064183,
-0.0993408300310918,-0.0662049594753124,-1.00000004543688E-6),
 .UNSPECIFIED.);
#371=B_SPLINE_CURVE_WITH_KNOTS('',3,(#33070,#33071,#33072,#33073,#33074,
#33075,#33076,#33077,#33078,#33079,#33080,#33081,#33082,#33083,#33084,#33085,
#33086,#33087,#33088,#33089,#33090,#33091,#33092,#33093,#33094,#33095,#33096,
#33097,#33098,#33099,#33100,#33101,#33102,#33103,#33104,#33105,#33106,#33107,
#33108,#33109,#33110,#33111,#33112,#33113,#33114,#33115,#33116,#33117,#33118,
#33119,#33120,#33121,#33122,#33123,#33124,#33125,#33126,#33127,#33128,#33129,
#33130,#33131,#33132,#33133,#33134,#33135,#33136,#33137,#33138,#33139,#33140,
#33141,#33142,#33143,#33144,#33145,#33146,#33147,#33148,#33149,#33150,#33151,
#33152,#33153,#33154,#33155,#33156,#33157,#33158,#33159,#33160,#33161,#33162,
#33163,#33164,#33165,#33166,#33167,#33168,#33169,#33170,#33171,#33172,#33173,
#33174,#33175,#33176,#33177,#33178,#33179,#33180,#33181,#33182,#33183,#33184,
#33185,#33186,#33187,#33188,#33189,#33190,#33191,#33192,#33193,#33194,#33195,
#33196,#33197,#33198,#33199,#33200,#33201,#33202,#33203,#33204,#33205,#33206,
#33207,#33208,#33209,#33210,#33211,#33212,#33213,#33214,#33215,#33216,#33217,
#33218,#33219,#33220,#33221,#33222,#33223,#33224,#33225,#33226,#33227,#33228,
#33229,#33230,#33231,#33232,#33233,#33234,#33235,#33236,#33237,#33238,#33239,
#33240,#33241,#33242,#33243,#33244,#33245,#33246,#33247,#33248,#33249,#33250,
#33251,#33252,#33253,#33254,#33255,#33256,#33257,#33258,#33259,#33260,#33261,
#33262,#33263,#33264,#33265,#33266,#33267,#33268,#33269,#33270,#33271,#33272,
#33273,#33274,#33275,#33276,#33277,#33278,#33279,#33280,#33281,#33282,#33283,
#33284,#33285,#33286,#33287,#33288,#33289,#33290,#33291,#33292,#33293,#33294,
#33295,#33296,#33297,#33298,#33299,#33300,#33301,#33302,#33303,#33304,#33305,
#33306,#33307,#33308,#33309,#33310,#33311,#33312,#33313,#33314,#33315,#33316,
#33317,#33318,#33319,#33320,#33321,#33322,#33323,#33324,#33325,#33326,#33327,
#33328,#33329,#33330,#33331,#33332,#33333,#33334,#33335,#33336,#33337,#33338,
#33339,#33340,#33341,#33342,#33343,#33344,#33345,#33346,#33347,#33348,#33349,
#33350,#33351,#33352,#33353,#33354,#33355,#33356,#33357,#33358,#33359,#33360,
#33361,#33362,#33363,#33364,#33365,#33366,#33367,#33368,#33369,#33370,#33371,
#33372,#33373,#33374,#33375,#33376,#33377,#33378,#33379,#33380,#33381,#33382,
#33383,#33384,#33385,#33386,#33387,#33388,#33389,#33390,#33391,#33392,#33393,
#33394,#33395,#33396,#33397,#33398,#33399,#33400,#33401,#33402,#33403,#33404,
#33405,#33406,#33407,#33408,#33409,#33410,#33411,#33412,#33413,#33414,#33415,
#33416,#33417,#33418,#33419,#33420,#33421,#33422,#33423,#33424,#33425,#33426,
#33427,#33428,#33429,#33430,#33431,#33432,#33433,#33434,#33435,#33436,#33437,
#33438,#33439,#33440,#33441,#33442,#33443,#33444,#33445,#33446,#33447,#33448,
#33449,#33450,#33451,#33452,#33453,#33454,#33455,#33456,#33457,#33458,#33459,
#33460,#33461,#33462,#33463,#33464,#33465,#33466,#33467,#33468,#33469,#33470,
#33471,#33472,#33473,#33474,#33475,#33476,#33477,#33478,#33479,#33480,#33481,
#33482,#33483,#33484,#33485,#33486,#33487,#33488,#33489,#33490,#33491,#33492,
#33493,#33494,#33495,#33496,#33497,#33498,#33499,#33500,#33501,#33502,#33503,
#33504,#33505,#33506,#33507,#33508,#33509,#33510,#33511,#33512,#33513,#33514,
#33515,#33516,#33517,#33518,#33519,#33520,#33521,#33522,#33523,#33524,#33525,
#33526,#33527,#33528,#33529,#33530,#33531,#33532,#33533,#33534,#33535,#33536,
#33537,#33538,#33539,#33540,#33541,#33542,#33543,#33544,#33545,#33546,#33547,
#33548,#33549,#33550,#33551,#33552,#33553,#33554,#33555,#33556,#33557,#33558,
#33559,#33560,#33561,#33562,#33563,#33564,#33565,#33566,#33567,#33568,#33569,
#33570,#33571,#33572,#33573,#33574,#33575,#33576,#33577,#33578,#33579,#33580,
#33581,#33582,#33583,#33584,#33585,#33586,#33587,#33588,#33589,#33590,#33591,
#33592,#33593,#33594,#33595,#33596,#33597,#33598,#33599,#33600,#33601,#33602,
#33603,#33604,#33605,#33606,#33607,#33608,#33609,#33610,#33611,#33612,#33613,
#33614,#33615,#33616,#33617,#33618,#33619,#33620,#33621,#33622,#33623,#33624,
#33625,#33626,#33627,#33628,#33629,#33630,#33631,#33632,#33633,#33634,#33635,
#33636,#33637,#33638,#33639,#33640,#33641,#33642,#33643,#33644,#33645),
 .UNSPECIFIED.,.F.,.F.,(4,2,2,2,2,2,2,2,2,2,2,2,2,2,2,2,2,2,2,2,2,2,2,2,
2,2,2,2,2,2,2,2,2,2,2,2,2,2,2,2,2,2,2,2,2,2,2,2,2,2,2,2,2,2,2,2,2,2,2,2,
2,2,2,2,2,2,2,2,2,2,2,2,2,2,2,2,2,2,2,2,2,2,2,2,2,2,2,2,2,2,2,2,2,2,2,2,
2,2,2,2,2,2,2,2,2,2,2,2,2,2,2,2,2,2,2,2,2,2,2,2,2,2,2,2,2,2,2,2,2,2,2,2,
2,2,2,2,2,2,2,2,2,2,2,2,2,2,2,2,2,2,2,2,2,2,2,2,2,2,2,2,2,2,2,2,2,2,2,2,
2,2,2,2,2,2,2,2,2,2,2,2,2,2,2,2,2,2,2,2,2,2,2,2,2,2,2,2,2,2,2,2,2,2,2,2,
2,2,2,2,2,2,2,2,2,2,2,2,2,2,2,2,2,2,2,2,2,2,2,2,2,2,2,2,2,2,2,2,2,2,2,2,
2,2,2,2,2,2,2,2,2,2,2,2,2,2,2,2,2,2,2,2,2,2,2,2,2,2,2,2,2,2,2,2,2,2,2,2,
2,2,2,2,2,2,2,2,2,2,2,4),(-5.66646737981884,-5.65202977713212,-5.64186283566428,
-5.6359415669808,-5.63021907568959,-5.62376470462157,-5.61358008762193,
-5.57889180222527,-5.53149386455273,-5.49696145083533,-5.48843911991611,
-5.48425585305101,-5.48089499215497,-5.47666391120387,-5.46789271648334,
-5.40071699055294,-5.36867042049385,-5.35436837701679,-5.34272537785606,
-5.33596359162933,-5.32997169531042,-5.32236912659647,-5.30645781792764,
-5.23737450623877,-5.20962989004014,-5.19385681219652,-5.18856501589677,
-5.18505883604978,-5.18142915713168,-5.17555884877083,-5.15604763182971,
-5.10584972629597,-5.05770159356469,-5.04570812516265,-5.03887299604999,
-5.03289112831685,-5.02540121392049,-5.01352848728401,-4.93581849064049,
-4.90215156296082,-4.89372632866156,-4.88956187527887,-4.88620063551178,
-4.88194951375378,-4.87307306320735,-4.82732692448115,-4.76865376762382,
-4.75148127709024,-4.74365512824748,-4.7376378501395,-4.7310003805168,-4.71994818150542,
-4.66852054851719,-4.62951266769257,-4.60129393389863,-4.59496694222568,
-4.59123769438089,-4.58782991164676,-4.58287706441957,-4.57060557609999,
-4.49173904485678,-4.45880225807595,-4.4490043152033,-4.44263106136734,
-4.43657894815234,-4.42812272961005,-4.40854861920622,-4.34375606864796,
-4.3171441661649,-4.3017844048574,-4.29654263789846,-4.29304665804954,-4.28940312240255,
-4.28346862934879,-4.2632572406141,-4.21356705024614,-4.18019709557297,
-4.15866449038775,-4.1501530995515,-4.14403081341646,-4.13841492595579,
-4.12927853651629,-4.105048167129,-4.04470564634612,-4.01039232827666,-4.00189477852074,
-3.99771651043792,-3.99435584991646,-3.99012021837193,-3.98132408175168,
-3.93236341124116,-3.90780092781493,-3.86883939843769,-3.85665929536066,
-3.84978546886808,-3.8438079346922,-3.83637340405622,-3.82469047681393,
-3.74602367273248,-3.71286593163613,-3.70449890384632,-3.7003458793686,
-3.6969844451918,-3.69272116041021,-3.68377997677606,-3.63958240022835,
-3.61099131413731,-3.57161724800104,-3.55937711275923,-3.55249046722558,
-3.54651358177317,-3.53909517356085,-3.52746858691514,-3.46075734008769,
-3.42793202837417,-3.41044307007549,-3.40495753887804,-3.40141093651012,
-3.39782991781627,-3.39218425006672,-3.37486457910174,-3.32303508073422,
-3.27388779954679,-3.26188137024388,-3.25504329110571,-3.24906137798557,
-3.24157475642982,-3.22971416504789,-3.15193394422553,-3.11830012773706,
-3.10987838530369,-3.10571446866184,-3.10235302329738,-3.09810083708849,
-3.0892195203075,-3.04360493844914,-3.01611590134675,-2.97690950322173,
-2.96469296457642,-2.95781087128827,-2.95183304806881,-2.94440712878804,
-2.93275592223282,-2.86631148295166,-2.83332018801372,-2.81607802899908,
-2.81044092814242,-2.80686153952506,-2.80331280572969,-2.79781822596739,
-2.78024850318555,-2.74716874247503,-2.68081763348978,-2.66915417275877,
-2.66172465481073,-2.65574652332987,-2.64886692294768,-2.63666254398883,
-2.59754205880952,-2.57075519925782,-2.52445043598243,-2.51552795985129,
-2.51126801152629,-2.50790643096073,-2.50374980368802,-2.49536513270769,
-2.46205548825634,-2.38361345270778,-2.3718762018619,-2.36442564117767,
-2.35844667999993,-2.35158376546011,-2.33945718311512,-2.28112314814783,
-2.2264133737659,-2.21791643273439,-2.21373809305878,-2.21037718609596,
-2.20614101973642,-2.19734305020684,-2.16025938582741,-2.09180103555146,
-2.07549855963712,-2.06779734707669,-2.06177949523892,-2.05514532955771,
-2.04410809581025,-1.98138814047806,-1.9293277717213,-1.92066600566779,
-1.91645582238859,-1.9130949300682,-1.90889077078366,-1.90026122274774,
-1.864755527422,-1.8010049854682,-1.78027906862233,-1.771677803246,-1.76560001299892,
-1.75926718237016,-1.74966792492346,-1.71891115046681,-1.65458661134996,
-1.6282223013374,-1.62182239498349,-1.61807726106605,-1.61463777152781,
-1.60969654482994,-1.59661815542594,-1.5757343467791,-1.53698251164871,
-1.48783016228087,-1.47694154571141,-1.4703389921685,-1.46431314773228,
-1.45641757833719,-1.43883650201319,-1.41401970757328,-1.37742348212445,
-1.33519137293408,-1.3262593361143,-1.32199806356053,-1.31863701205398,
-1.31448306084595,-1.3061102584762,-1.27290050023367,-1.19425650838086,
-1.18255727453901,-1.17511799410073,-1.16914012739284,-1.16226975073057,
-1.15010615416118,-1.0889964529071,-1.0374599219333,-1.02876365735641,-1.02454670641525,
-1.02118490981561,-1.01698498194405,-1.00838295483133,-0.973138996154328,
-0.910123507190809,-0.888702629059718,-0.87998229198576,-0.873881985281281,
-0.867577729458823,-0.858124455948534,-0.828856995839813,-0.778117056820806,
-0.73717460449203,-0.730414977910018,-0.726553195954124,-0.723156579384028,
-0.718477799940821,-0.707126939379542,-0.690070821879275,-0.61894076230909,
-0.592827418822905,-0.583463979045129,-0.57781088894916,-0.571726063796511,
-0.563409669675828,-0.543173184478235,-0.512778117269808,-0.45405516887641,
-0.437429715620349,-0.431868024820915,-0.428660041397706,-0.425178111955145,
-0.420003204802352,-0.405176509138087,-0.379981617743587,-0.320372090636363,
-0.295214332417875,-0.285954937889434,-0.280315707830894,-0.274208218380575,
-0.265791727463636,-0.244923838854528,-0.213104029072987,-0.145572678770187,
-0.136883779871564,-0.132665685856985,-0.129296100761455,-0.1250762439012,
-0.116413307166631,-0.0806871329657728,-0.0158458709233213,-1.00000000013978E-6),
 .UNSPECIFIED.);
#372=B_SPLINE_CURVE_WITH_KNOTS('',3,(#33646,#33647,#33648,#33649,#33650,
#33651,#33652,#33653,#33654,#33655,#33656,#33657,#33658,#33659,#33660,#33661,
#33662,#33663,#33664,#33665,#33666,#33667,#33668,#33669,#33670,#33671,#33672,
#33673,#33674,#33675,#33676,#33677,#33678,#33679,#33680,#33681,#33682,#33683,
#33684,#33685,#33686,#33687,#33688,#33689,#33690,#33691,#33692,#33693,#33694,
#33695,#33696,#33697,#33698,#33699,#33700,#33701,#33702,#33703,#33704,#33705,
#33706,#33707,#33708,#33709,#33710,#33711,#33712,#33713,#33714,#33715,#33716,
#33717,#33718,#33719,#33720,#33721,#33722,#33723,#33724,#33725,#33726,#33727,
#33728,#33729,#33730,#33731,#33732,#33733,#33734,#33735,#33736,#33737,#33738,
#33739,#33740,#33741,#33742,#33743,#33744,#33745,#33746,#33747,#33748,#33749,
#33750,#33751,#33752,#33753,#33754,#33755,#33756,#33757,#33758,#33759,#33760,
#33761,#33762,#33763,#33764,#33765,#33766,#33767,#33768,#33769,#33770,#33771,
#33772,#33773,#33774,#33775),.UNSPECIFIED.,.F.,.F.,(4,2,2,2,2,2,2,2,2,2,
2,2,2,2,2,2,2,2,2,2,2,2,2,2,2,2,2,2,2,2,2,2,2,2,2,2,2,2,2,2,2,2,2,2,2,2,
2,2,2,2,2,2,2,2,2,2,2,2,2,2,2,2,2,2,4),(1.24528113121354E-5,0.028631889083293,
0.0408247356106915,0.045280590035446,0.0485000424796718,0.0517866681795052,
0.0554902755365286,0.0618059384212369,0.0872969915363886,0.130173433480661,
0.162959191226469,0.186192291234085,0.194967556390622,0.201162746958399,
0.206769526698791,0.214297686819927,0.23314806277008,0.296603596769671,
0.331602370103769,0.340207789039151,0.344448021752713,0.347842071702048,
0.352102503717678,0.361032071767464,0.402285316490655,0.437722675474088,
0.463551666330535,0.481609663048884,0.489560110176308,0.495567551977114,
0.502090489839575,0.512706981711773,0.553638735569381,0.608443290521791,
0.633037596026065,0.639303211024447,0.642998592011321,0.646394118103218,
0.651286079343969,0.664335427032788,0.68523798828632,0.723801928508903,
0.773358298195291,0.784093381456232,0.790593287408483,0.796516211751473,
0.804259439528729,0.821393069658049,0.845417609013507,0.883337362202561,
0.888393239049124,0.929780685976583,0.936478787684859,0.940286064788971,
0.943639514542793,0.94823764090924,0.959235542588296,1.01763285273625,1.04597037320218,
1.07375399933964,1.08324582206853,1.08952307352542,1.09514563179514,1.10081989957959,
1.10723007897768),.UNSPECIFIED.);
#373=B_SPLINE_CURVE_WITH_KNOTS('',3,(#33999,#34000,#34001,#34002,#34003,
#34004,#34005),.UNSPECIFIED.,.F.,.F.,(4,1,1,1,4),(0.000143951182684975,
0.249992846908436,0.499984711894009,0.749976576879583,0.999370396581308),
 .UNSPECIFIED.);
#374=B_SPLINE_CURVE_WITH_KNOTS('',3,(#34006,#34007,#34008,#34009,#34010,
#34011,#34012,#34013,#34014,#34015,#34016,#34017,#34018,#34019,#34020,#34021,
#34022,#34023,#34024,#34025,#34026,#34027,#34028,#34029,#34030,#34031,#34032,
#34033,#34034,#34035,#34036,#34037,#34038,#34039,#34040,#34041,#34042,#34043,
#34044,#34045,#34046,#34047,#34048,#34049,#34050,#34051,#34052,#34053,#34054,
#34055,#34056,#34057,#34058,#34059,#34060,#34061,#34062,#34063,#34064,#34065,
#34066,#34067,#34068,#34069,#34070,#34071,#34072,#34073,#34074,#34075,#34076,
#34077,#34078,#34079,#34080,#34081,#34082,#34083,#34084,#34085,#34086,#34087,
#34088,#34089,#34090,#34091,#34092,#34093,#34094,#34095,#34096,#34097,#34098,
#34099,#34100,#34101,#34102,#34103,#34104,#34105,#34106,#34107,#34108,#34109,
#34110,#34111,#34112,#34113,#34114,#34115,#34116,#34117,#34118,#34119,#34120,
#34121,#34122,#34123,#34124,#34125,#34126,#34127,#34128,#34129,#34130,#34131,
#34132,#34133,#34134,#34135,#34136,#34137,#34138,#34139,#34140,#34141,#34142,
#34143,#34144,#34145,#34146,#34147,#34148,#34149,#34150,#34151,#34152,#34153,
#34154,#34155,#34156,#34157,#34158,#34159,#34160,#34161,#34162,#34163,#34164,
#34165,#34166,#34167,#34168,#34169,#34170,#34171),.UNSPECIFIED.,.F.,.F.,
(4,2,2,2,2,2,2,2,2,2,2,2,2,2,2,2,2,2,2,2,2,2,2,2,2,2,2,2,2,2,2,2,2,2,2,
2,2,2,2,2,2,2,2,2,2,2,2,2,2,2,2,2,2,2,2,2,2,2,2,2,2,2,2,2,2,2,2,2,2,2,2,
2,2,2,2,2,2,2,2,2,2,2,4),(-4.85680415953354,-4.8501799720293,-4.82795587041218,
-4.79832010131199,-4.79124321059898,-4.78658794634873,-4.78206143088215,
-4.77542775596836,-4.75470353170186,-4.72943885798795,-4.7176911448229,
-4.71386627329548,-4.71128726556225,-4.70844794529031,-4.703223995751,-4.68410777517529,
-4.65940719494081,-4.64497557392077,-4.63909845834549,-4.63468350385385,
-4.62984784705791,-4.62168669624962,-4.5857391656108,-4.56605598267604,
-4.56177473355638,-4.55914552997483,-4.55652816323524,-4.5522510195785,
-4.53233977338937,-4.50683526203999,-4.49217064740255,-4.48629976032288,
-4.48192574037172,-4.47717271006402,-4.46925412267292,-4.43307835023872,
-4.4147776420783,-4.40968935067262,-4.40690608234038,-4.40442240623259,
-4.40074367439207,-4.39073777460239,-4.35658262888147,-4.33992777921667,
-4.3337911590246,-4.32934665053616,-4.32463014308964,-4.31703043657081,
-4.28065221276563,-4.26238805368253,-4.25728583749115,-4.25448116258635,
-4.25198471393949,-4.2482683555091,-4.23797743673025,-4.20417495177972,
-4.18759984766012,-4.18147950515469,-4.17704430402583,-4.17233613208709,
-4.16474903166549,-4.12527279211248,-4.10808704674472,-4.10391636238359,
-4.10131284399107,-4.09898506640493,-4.09491271650107,-4.08077476576487,
-4.05062559648586,-4.03477044416374,-4.02873478569039,-4.02431666336258,
-4.01958664091511,-4.01187134965379,-3.9803940400591,-3.95594501702431,
-3.95155457371567,-3.94890593978513,-3.94629702828529,-3.94210273808332,
-3.92554506752803,-3.89743871250035,-3.88535150283469),.UNSPECIFIED.);
#375=B_SPLINE_CURVE_WITH_KNOTS('',3,(#34389,#34390,#34391,#34392,#34393,
#34394,#34395,#34396,#34397,#34398,#34399,#34400,#34401,#34402,#34403,#34404,
#34405,#34406,#34407,#34408,#34409,#34410,#34411,#34412,#34413,#34414,#34415,
#34416,#34417,#34418,#34419,#34420,#34421,#34422,#34423,#34424,#34425,#34426,
#34427,#34428,#34429,#34430,#34431,#34432,#34433,#34434,#34435,#34436,#34437,
#34438,#34439,#34440,#34441,#34442,#34443,#34444,#34445,#34446,#34447,#34448,
#34449,#34450,#34451,#34452,#34453,#34454,#34455,#34456,#34457,#34458,#34459,
#34460,#34461,#34462,#34463,#34464,#34465,#34466,#34467,#34468,#34469,#34470,
#34471,#34472,#34473,#34474,#34475,#34476,#34477,#34478,#34479,#34480,#34481,
#34482,#34483,#34484,#34485,#34486,#34487,#34488,#34489,#34490,#34491,#34492,
#34493,#34494,#34495,#34496,#34497,#34498,#34499,#34500,#34501,#34502,#34503,
#34504,#34505,#34506,#34507,#34508,#34509,#34510,#34511,#34512,#34513,#34514,
#34515,#34516,#34517,#34518,#34519,#34520,#34521,#34522,#34523,#34524,#34525,
#34526,#34527,#34528,#34529,#34530,#34531,#34532,#34533,#34534,#34535,#34536,
#34537,#34538,#34539,#34540,#34541,#34542,#34543,#34544,#34545,#34546,#34547,
#34548,#34549,#34550,#34551,#34552,#34553,#34554,#34555,#34556,#34557,#34558,
#34559,#34560,#34561,#34562,#34563,#34564),.UNSPECIFIED.,.F.,.F.,(4,2,2,
2,2,2,2,2,2,2,2,2,2,2,2,2,2,2,2,2,2,2,2,2,2,2,2,2,2,2,2,2,2,2,2,2,2,2,2,
2,2,2,2,2,2,2,2,2,2,2,2,2,2,2,2,2,2,2,2,2,2,2,2,2,2,2,2,2,2,2,2,2,2,2,2,
2,2,2,2,2,2,2,2,2,2,2,2,4),(0.000139559779193673,0.00418312955586237,0.00978488685190961,
0.0413781338730359,0.0574037092840092,0.0666164948624175,0.0700458250993038,
0.0724637085699126,0.0752465177003127,0.08037206612107,0.100124782142703,
0.124948084354604,0.13939323491165,0.145150543418712,0.149416608566436,
0.154022811938123,0.161603791189514,0.199956422345138,0.218677502217384,
0.222845565440813,0.225396316072621,0.227925417719586,0.231996183820311,
0.247481281138077,0.276999600765713,0.29269249409177,0.298599224334203,
0.302884034373717,0.307426724561561,0.31470887053306,0.349892125706388,
0.365065477915852,0.373976686412166,0.377357746153798,0.379762464599789,
0.382557255377237,0.387747460835412,0.408650817284414,0.427703933187463,
0.445734894405103,0.451892404985478,0.456223250300085,0.460169759950361,
0.46662169681185,0.485760179307897,0.503808128813803,0.524013803822886,
0.529158800802302,0.531944757206762,0.534354258517986,0.537758757349042,
0.546831252763403,0.562453735156471,0.596693913331176,0.604091487611082,
0.608659888223021,0.612938810495531,0.618789244053598,0.63398213803354,
0.661455620923727,0.679437337704363,0.683625524980089,0.686180651837019,
0.688707737771483,0.692763739718316,0.709135302875068,0.743836215926229,
0.755132396510595,0.760426365199457,0.764637484032459,0.769486109674433,
0.778300983637962,0.801020550619598,0.830599067149249,0.836196045961441,
0.839039940921639,0.841195115832224,0.844336540072541,0.851610758378909,
0.862698005023155,0.897182523982601,0.908660285201998,0.91398456758211,
0.918198714606633,0.923028089704658,0.931740813946652,0.956469632034719,
0.971411654023308),.UNSPECIFIED.);
#376=B_SPLINE_CURVE_WITH_KNOTS('',3,(#34565,#34566,#34567,#34568),
 .UNSPECIFIED.,.F.,.F.,(4,4),(0.537782073242468,0.537816282017176),
 .UNSPECIFIED.);
#377=B_SPLINE_CURVE_WITH_KNOTS('',3,(#34569,#34570,#34571,#34572,#34573,
#34574,#34575,#34576,#34577,#34578,#34579,#34580,#34581,#34582,#34583,#34584,
#34585,#34586,#34587),.UNSPECIFIED.,.F.,.F.,(4,3,3,3,3,3,4),(0.,0.321652726498616,
0.335818547580298,0.5,0.813168066582452,0.83581854758052,1.),
 .UNSPECIFIED.);
#378=B_SPLINE_CURVE_WITH_KNOTS('',3,(#34600,#34601,#34602,#34603,#34604,
#34605,#34606),.UNSPECIFIED.,.F.,.F.,(4,3,4),(8.942092232521E-7,0.897079636775044,
1.),.UNSPECIFIED.);
#379=B_SPLINE_CURVE_WITH_KNOTS('',3,(#34629,#34630,#34631,#34632,#34633,
#34634,#34635),.UNSPECIFIED.,.F.,.F.,(4,3,4),(0.000178264861484437,0.742416332780832,
0.999844713842845),.UNSPECIFIED.);
#380=B_SPLINE_CURVE_WITH_KNOTS('',3,(#34637,#34638,#34639,#34640,#34641,
#34642,#34643,#34644,#34645,#34646),.UNSPECIFIED.,.F.,.F.,(4,3,3,4),(0.,
0.519872273097902,0.615160302254839,1.),.UNSPECIFIED.);
#381=B_SPLINE_CURVE_WITH_KNOTS('',3,(#34667,#34668,#34669,#34670,#34671,
#34672,#34673,#34674,#34675,#34676),.UNSPECIFIED.,.F.,.F.,(4,2,2,2,4),(3.67941030579461E-9,
0.326260440009545,0.5,0.826260436373397,1.),.UNSPECIFIED.);
#382=B_SPLINE_CURVE_WITH_KNOTS('',3,(#34679,#34680,#34681,#34682,#34683,
#34684,#34685,#34686,#34687,#34688,#34689,#34690,#34691,#34692),
 .UNSPECIFIED.,.F.,.F.,(4,2,2,2,2,2,4),(-0.224981239925635,-0.193512649663793,
-0.161961102829213,-0.112487004321429,-0.062975091378892,-0.0314451815916685,
-1.40071649520604E-6),.UNSPECIFIED.);
#383=B_SPLINE_CURVE_WITH_KNOTS('',3,(#34713,#34714,#34715,#34716,#34717,
#34718,#34719,#34720,#34721,#34722,#34723,#34724,#34725),.UNSPECIFIED.,
 .F.,.F.,(4,3,3,3,4),(1.02472631714155E-12,0.387568508029344,0.49999981776731,
0.887555122346297,0.999873703557718),.UNSPECIFIED.);
#384=B_SPLINE_CURVE_WITH_KNOTS('',3,(#34727,#34728,#34729,#34730,#34731,
#34732,#34733,#34734,#34735,#34736),.UNSPECIFIED.,.F.,.F.,(4,2,2,2,4),(2.94135345515086E-12,
0.448076600669202,0.5,0.948076600665885,0.999999999999085),
 .UNSPECIFIED.);
#385=B_SPLINE_CURVE_WITH_KNOTS('',3,(#34757,#34758,#34759,#34760,#34761,
#34762),.UNSPECIFIED.,.F.,.F.,(4,2,4),(9.99999979321194E-7,0.0329350911858533,
0.0651002228197631),.UNSPECIFIED.);
#386=B_SPLINE_CURVE_WITH_KNOTS('',3,(#34790,#34791,#34792,#34793,#34794,
#34795,#34796,#34797,#34798,#34799,#34800,#34801,#34802,#34803,#34804,#34805,
#34806,#34807,#34808,#34809,#34810,#34811,#34812,#34813,#34814,#34815,#34816,
#34817,#34818,#34819,#34820,#34821,#34822,#34823,#34824,#34825,#34826,#34827,
#34828,#34829,#34830,#34831,#34832,#34833,#34834,#34835,#34836,#34837,#34838),
 .UNSPECIFIED.,.F.,.F.,(4,3,3,3,3,3,3,3,3,3,3,3,3,3,3,3,4),(0.,0.0927605595561279,
0.125,0.216051601199591,0.25,0.341388358155206,0.375,0.46637118185636,0.5,
0.591371181856193,0.625,0.716388358155103,0.75,0.841051601199441,0.875,
0.967760559556323,1.),.UNSPECIFIED.);
#387=B_SPLINE_CURVE_WITH_KNOTS('',3,(#34840,#34841,#34842,#34843,#34844,
#34845,#34846,#34847,#34848,#34849,#34850,#34851,#34852,#34853,#34854,#34855,
#34856,#34857,#34858,#34859,#34860,#34861,#34862,#34863,#34864,#34865,#34866,
#34867,#34868,#34869,#34870,#34871,#34872,#34873,#34874,#34875,#34876,#34877,
#34878,#34879,#34880,#34881,#34882,#34883,#34884,#34885,#34886,#34887,#34888,
#34889,#34890,#34891,#34892,#34893,#34894),.UNSPECIFIED.,.F.,.F.,(4,3,3,
3,3,3,3,3,3,3,3,3,3,3,3,3,3,3,4),(1.15710129956961E-6,0.0927580101727587,
0.125,0.215560207328814,0.25,0.343554436628594,0.375,0.4375,0.46875,0.5,
0.53125,0.5625,0.625,0.6875,0.75,0.835314126539692,0.875,0.952649745898871,
0.999999206802969),.UNSPECIFIED.);
#388=B_SPLINE_CURVE_WITH_KNOTS('',3,(#34896,#34897,#34898,#34899,#34900,
#34901,#34902,#34903,#34904,#34905,#34906,#34907,#34908,#34909,#34910,#34911,
#34912,#34913,#34914,#34915,#34916,#34917,#34918,#34919,#34920,#34921,#34922,
#34923,#34924,#34925,#34926,#34927,#34928,#34929,#34930,#34931,#34932,#34933,
#34934,#34935,#34936,#34937,#34938,#34939,#34940,#34941,#34942,#34943,#34944),
 .UNSPECIFIED.,.F.,.F.,(4,3,3,3,3,3,3,3,3,3,3,3,3,3,3,3,4),(0.,0.0927652271086669,
0.125,0.216056340442133,0.25,0.341393095875492,0.375,0.466375911195523,
0.5,0.59137591119598,0.625,0.716393095875431,0.75,0.841056340442169,0.875,
0.967765227108083,1.),.UNSPECIFIED.);
#389=B_SPLINE_CURVE_WITH_KNOTS('',3,(#34946,#34947,#34948,#34949,#34950,
#34951,#34952,#34953,#34954,#34955,#34956,#34957,#34958,#34959,#34960,#34961,
#34962,#34963,#34964,#34965,#34966,#34967,#34968,#34969,#34970,#34971,#34972,
#34973,#34974,#34975,#34976,#34977,#34978,#34979,#34980,#34981,#34982,#34983,
#34984,#34985,#34986,#34987,#34988,#34989,#34990,#34991,#34992,#34993,#34994),
 .UNSPECIFIED.,.F.,.F.,(4,3,3,3,3,3,3,3,3,3,3,3,3,3,3,3,4),(0.,0.0927588912582948,
0.125,0.216049907277145,0.25,0.34138666477614,0.375,0.466369491473306,0.5,
0.591369491472985,0.625,0.716386664776259,0.75,0.841049907277114,0.875,
0.967758891258586,1.),.UNSPECIFIED.);
#390=B_SPLINE_CURVE_WITH_KNOTS('',3,(#34996,#34997,#34998,#34999,#35000,
#35001,#35002,#35003,#35004,#35005,#35006,#35007,#35008,#35009,#35010,#35011,
#35012,#35013,#35014,#35015,#35016,#35017,#35018,#35019,#35020,#35021,#35022,
#35023,#35024,#35025,#35026,#35027,#35028,#35029,#35030,#35031,#35032,#35033,
#35034,#35035,#35036,#35037,#35038,#35039,#35040,#35041,#35042,#35043,#35044,
#35045,#35046,#35047,#35048,#35049,#35050,#35051,#35052,#35053,#35054,#35055,
#35056,#35057,#35058,#35059,#35060,#35061,#35062,#35063,#35064,#35065,#35066,
#35067,#35068,#35069,#35070,#35071),.UNSPECIFIED.,.F.,.F.,(4,3,3,3,3,3,
3,3,3,3,3,3,3,3,3,3,3,3,3,3,3,3,3,3,3,4),(1.15508471750028E-6,0.092144029884165,
0.125,0.216529255746127,0.25,0.3125,0.375,0.40625,0.4375,0.46875,0.484375,
0.4921875,0.5,0.5078125,0.515625,0.53125,0.5625,0.59375,0.625,0.6875,0.75,
0.8125,0.875,0.9375,0.995454104613646,0.999999596646375),.UNSPECIFIED.);
#391=B_SPLINE_CURVE_WITH_KNOTS('',3,(#35073,#35074,#35075,#35076,#35077,
#35078,#35079,#35080,#35081,#35082,#35083,#35084,#35085,#35086,#35087,#35088,
#35089,#35090,#35091,#35092,#35093,#35094,#35095,#35096,#35097,#35098,#35099,
#35100,#35101,#35102,#35103,#35104,#35105,#35106,#35107,#35108,#35109,#35110,
#35111,#35112,#35113,#35114,#35115,#35116,#35117,#35118,#35119,#35120,#35121),
 .UNSPECIFIED.,.F.,.F.,(4,3,3,3,3,3,3,3,3,3,3,3,3,3,3,3,4),(0.,0.0927687029302607,
0.125,0.216059869646637,0.25,0.341396623944995,0.375,0.466379433025891,
0.5,0.59137943302596,0.625,0.71639662394496,0.75,0.841059869646648,0.875,
0.967768702930745,1.),.UNSPECIFIED.);
#392=B_SPLINE_CURVE_WITH_KNOTS('',3,(#35123,#35124,#35125,#35126,#35127,
#35128,#35129,#35130,#35131,#35132,#35133,#35134,#35135,#35136,#35137,#35138,
#35139,#35140,#35141,#35142,#35143,#35144,#35145,#35146,#35147,#35148,#35149,
#35150,#35151,#35152,#35153,#35154,#35155,#35156,#35157,#35158,#35159,#35160,
#35161,#35162,#35163,#35164,#35165,#35166,#35167,#35168,#35169,#35170,#35171),
 .UNSPECIFIED.,.F.,.F.,(4,3,3,3,3,3,3,3,3,3,3,3,3,3,3,3,4),(0.,0.0927568833925016,
0.125,0.216047868569561,0.25,0.34138462672263,0.375,0.46636745702548,0.5,
0.59136745702557,0.625,0.716384626722753,0.75,0.841047868569713,0.875,0.967756883392973,
1.),.UNSPECIFIED.);
#393=B_SPLINE_CURVE_WITH_KNOTS('',3,(#35173,#35174,#35175,#35176,#35177,
#35178,#35179,#35180,#35181,#35182,#35183,#35184,#35185,#35186,#35187,#35188,
#35189,#35190,#35191,#35192,#35193,#35194,#35195,#35196,#35197,#35198,#35199,
#35200,#35201,#35202,#35203,#35204,#35205,#35206,#35207,#35208,#35209,#35210,
#35211,#35212,#35213,#35214,#35215,#35216,#35217,#35218,#35219,#35220,#35221),
 .UNSPECIFIED.,.F.,.F.,(4,3,3,3,3,3,3,3,3,3,3,3,3,3,3,3,4),(1.00511200959296E-6,
0.0927437682042961,0.125,0.216035219771111,0.25,0.341376986124011,0.375,
0.466313829040159,0.5,0.591406458509517,0.625,0.716377484365712,0.75,0.841045743313971,
0.875,0.967756443545387,0.99999978647056),.UNSPECIFIED.);
#394=B_SPLINE_CURVE_WITH_KNOTS('',3,(#35223,#35224,#35225,#35226,#35227,
#35228,#35229,#35230,#35231,#35232,#35233,#35234,#35235,#35236,#35237,#35238,
#35239,#35240,#35241,#35242,#35243,#35244,#35245,#35246,#35247,#35248,#35249,
#35250,#35251,#35252,#35253,#35254,#35255,#35256,#35257,#35258,#35259,#35260,
#35261,#35262,#35263,#35264,#35265,#35266,#35267,#35268,#35269,#35270,#35271),
 .UNSPECIFIED.,.F.,.F.,(4,3,3,3,3,3,3,3,3,3,3,3,3,3,3,3,4),(0.,0.0927720508247614,
0.125,0.216063268956037,0.25,0.341400022160318,0.375,0.466382825231913,
0.5,0.591382825232266,0.625,0.716400022160194,0.75,0.841063268956108,0.875,
0.967772050824302,1.),.UNSPECIFIED.);
#395=B_SPLINE_CURVE_WITH_KNOTS('',3,(#35277,#35278,#35279,#35280,#35281,
#35282,#35283,#35284,#35285,#35286,#35287,#35288,#35289,#35290,#35291,#35292,
#35293,#35294,#35295,#35296,#35297,#35298,#35299,#35300,#35301),
 .UNSPECIFIED.,.F.,.F.,(4,3,3,3,3,3,3,3,4),(0.,0.125,0.25,0.375,0.5,0.625,
0.75,0.875,0.999999474719706),.UNSPECIFIED.);
#396=B_SPLINE_CURVE_WITH_KNOTS('',3,(#35303,#35304,#35305,#35306,#35307,
#35308,#35309,#35310,#35311,#35312,#35313,#35314,#35315,#35316,#35317,#35318,
#35319,#35320,#35321,#35322,#35323,#35324,#35325,#35326,#35327,#35328,#35329,
#35330,#35331,#35332,#35333,#35334,#35335,#35336,#35337,#35338,#35339,#35340,
#35341,#35342,#35343,#35344,#35345,#35346,#35347,#35348,#35349,#35350,#35351),
 .UNSPECIFIED.,.F.,.F.,(4,3,3,3,3,3,3,3,3,3,3,3,3,3,3,3,4),(0.,0.092751628903762,
0.125,0.216042533365587,0.25,0.341379293228406,0.375,0.466362132969287,
0.5,0.591362132969264,0.625,0.716379293228501,0.75,0.841042533365549,0.875,
0.967751628903877,1.),.UNSPECIFIED.);
#397=B_SPLINE_CURVE_WITH_KNOTS('',3,(#35353,#35354,#35355,#35356,#35357,
#35358,#35359,#35360,#35361,#35362,#35363,#35364,#35365,#35366,#35367,#35368,
#35369,#35370,#35371,#35372,#35373,#35374,#35375,#35376,#35377,#35378,#35379,
#35380,#35381,#35382,#35383,#35384,#35385,#35386,#35387,#35388,#35389,#35390,
#35391,#35392,#35393,#35394,#35395,#35396,#35397,#35398,#35399,#35400,#35401),
 .UNSPECIFIED.,.F.,.F.,(4,3,3,3,3,3,3,3,3,3,3,3,3,3,3,3,4),(0.,0.0927733010189759,
0.125,0.216064538349619,0.25,0.341401291145062,0.375,0.4663840919732,0.5,
0.591384091973165,0.625,0.716401291144964,0.75,0.841064538349631,0.875,
0.967773301019603,1.),.UNSPECIFIED.);
#398=B_SPLINE_CURVE_WITH_KNOTS('',3,(#35403,#35404,#35405,#35406,#35407,
#35408,#35409,#35410,#35411,#35412,#35413,#35414,#35415,#35416,#35417,#35418,
#35419,#35420,#35421,#35422,#35423,#35424,#35425,#35426,#35427,#35428,#35429,
#35430,#35431,#35432,#35433,#35434,#35435,#35436,#35437,#35438,#35439,#35440,
#35441,#35442,#35443,#35444,#35445,#35446,#35447,#35448,#35449,#35450,#35451,
#35452,#35453,#35454),.UNSPECIFIED.,.F.,.F.,(4,2,2,2,2,2,2,2,2,2,2,2,2,
2,2,2,2,2,2,2,2,2,2,2,2,4),(0.,0.0553130156040213,0.0625,0.125,0.1875,0.25,
0.3125,0.375,0.40625,0.4375,0.46875,0.484375,0.4921875,0.5,0.5078125,0.515625,
0.53125,0.5625,0.59375,0.625,0.6875,0.75,0.841517211022419,0.875,0.967130863494855,
0.999999278904145),.UNSPECIFIED.);
#399=B_SPLINE_CURVE_WITH_KNOTS('',3,(#35456,#35457,#35458,#35459,#35460,
#35461,#35462,#35463,#35464,#35465,#35466,#35467,#35468,#35469,#35470,#35471,
#35472,#35473,#35474,#35475,#35476,#35477,#35478,#35479,#35480,#35481,#35482,
#35483,#35484,#35485,#35486,#35487,#35488,#35489,#35490,#35491,#35492,#35493,
#35494,#35495,#35496,#35497,#35498,#35499,#35500,#35501,#35502,#35503,#35504),
 .UNSPECIFIED.,.F.,.F.,(4,3,3,3,3,3,3,3,3,3,3,3,3,3,3,3,4),(0.,0.092754553141066,
0.125,0.21604550252371,0.25,0.341382261435592,0.375,0.466365095923449,0.5,
0.591365095923193,0.625,0.716382261435363,0.75,0.841045502523726,0.875,
0.96775455314112,1.),.UNSPECIFIED.);
#400=B_SPLINE_CURVE_WITH_KNOTS('',3,(#35506,#35507,#35508,#35509,#35510,
#35511,#35512,#35513,#35514,#35515,#35516,#35517,#35518,#35519,#35520,#35521,
#35522,#35523,#35524,#35525,#35526,#35527,#35528,#35529,#35530,#35531,#35532,
#35533,#35534,#35535,#35536,#35537,#35538,#35539,#35540,#35541,#35542,#35543,
#35544,#35545,#35546,#35547,#35548,#35549,#35550,#35551,#35552,#35553,#35554),
 .UNSPECIFIED.,.F.,.F.,(4,3,3,3,3,3,3,3,3,3,3,3,3,3,3,3,4),(0.,0.0927714769858617,
0.125,0.216062686304942,0.25,0.341399439696681,0.375,0.466382243798817,
0.5,0.591382243798365,0.625,0.716399439696732,0.75,0.841062686305149,0.875,
0.967771476985755,1.),.UNSPECIFIED.);
#401=B_SPLINE_CURVE_WITH_KNOTS('',3,(#35556,#35557,#35558,#35559,#35560,
#35561,#35562,#35563,#35564,#35565,#35566,#35567,#35568,#35569,#35570,#35571,
#35572,#35573,#35574,#35575,#35576,#35577,#35578,#35579,#35580,#35581,#35582,
#35583,#35584,#35585,#35586,#35587,#35588,#35589,#35590,#35591,#35592,#35593,
#35594,#35595,#35596,#35597,#35598,#35599,#35600,#35601,#35602,#35603,#35604,
#35605,#35606,#35607,#35608,#35609,#35610,#35611,#35612,#35613,#35614,#35615,
#35616,#35617,#35618,#35619,#35620,#35621,#35622,#35623,#35624,#35625,#35626,
#35627,#35628,#35629,#35630,#35631,#35632,#35633,#35634,#35635,#35636,#35637,
#35638,#35639,#35640,#35641,#35642,#35643),.UNSPECIFIED.,.F.,.F.,(4,3,3,
3,3,3,3,3,3,3,3,3,3,3,3,3,3,3,3,3,3,3,3,3,3,3,3,3,3,4),(1.05714741198223E-7,
0.0471016803099375,0.0625,0.114776485281687,0.125,0.183175405287037,0.1875,
0.25,0.3125,0.375,0.40625,0.4375,0.453125,0.46875,0.484375,0.4921875,0.5,
0.5078125,0.515625,0.53125,0.546875,0.5625,0.59375,0.625,0.6875,0.75,0.8125,
0.875,0.968959747574043,0.999999002444466),.UNSPECIFIED.);
#402=B_SPLINE_CURVE_WITH_KNOTS('',3,(#35645,#35646,#35647,#35648,#35649,
#35650,#35651,#35652,#35653,#35654,#35655,#35656,#35657,#35658,#35659,#35660,
#35661,#35662,#35663,#35664,#35665,#35666,#35667,#35668,#35669,#35670,#35671,
#35672,#35673,#35674,#35675,#35676,#35677,#35678,#35679,#35680,#35681,#35682,
#35683,#35684,#35685,#35686,#35687,#35688,#35689,#35690,#35691,#35692,#35693),
 .UNSPECIFIED.,.F.,.F.,(4,3,3,3,3,3,3,3,3,3,3,3,3,3,3,3,4),(0.,0.0927568305050716,
0.125,0.216047814869766,0.25,0.341384573040307,0.375,0.466367403437729,
0.5,0.591367403437667,0.625,0.716384573040161,0.75,0.841047814869804,0.875,
0.967756830505404,1.),.UNSPECIFIED.);
#403=B_SPLINE_CURVE_WITH_KNOTS('',3,(#35695,#35696,#35697,#35698,#35699,
#35700,#35701,#35702,#35703,#35704,#35705,#35706,#35707,#35708,#35709,#35710,
#35711,#35712,#35713,#35714,#35715,#35716,#35717,#35718,#35719,#35720,#35721,
#35722,#35723,#35724,#35725,#35726,#35727,#35728,#35729,#35730,#35731,#35732,
#35733,#35734,#35735,#35736,#35737,#35738,#35739,#35740,#35741,#35742,#35743),
 .UNSPECIFIED.,.F.,.F.,(4,3,3,3,3,3,3,3,3,3,3,3,3,3,3,3,4),(0.,0.0927687785918848,
0.125,0.21605994647008,0.25,0.341396700743647,0.375,0.466379509688856,0.5,
0.591379509688596,0.625,0.716396700743673,0.75,0.841059946470065,0.875,
0.967768778592018,1.),.UNSPECIFIED.);
#404=B_SPLINE_CURVE_WITH_KNOTS('',3,(#35745,#35746,#35747,#35748,#35749,
#35750,#35751,#35752,#35753,#35754,#35755,#35756,#35757,#35758,#35759,#35760,
#35761,#35762,#35763,#35764,#35765,#35766,#35767,#35768,#35769,#35770,#35771,
#35772,#35773,#35774,#35775,#35776,#35777,#35778),.UNSPECIFIED.,.F.,.F.,
(4,2,2,2,2,2,2,2,2,2,2,2,2,2,2,2,4),(6.2904793357381E-7,0.092754167897614,
0.125,0.216044766897767,0.25,0.341379705506234,0.375,0.466367644770845,
0.5,0.591380776467673,0.625,0.716346028360352,0.75,0.841038184239321,0.875,
0.967744550610455,0.999998988396429),.UNSPECIFIED.);
#405=B_SPLINE_CURVE_WITH_KNOTS('',3,(#35780,#35781,#35782,#35783),
 .UNSPECIFIED.,.F.,.F.,(4,4),(0.,0.999999235891784),.UNSPECIFIED.);
#406=B_SPLINE_CURVE_WITH_KNOTS('',3,(#35786,#35787,#35788,#35789,#35790,
#35791,#35792,#35793,#35794,#35795,#35796,#35797,#35798,#35799,#35800,#35801,
#35802,#35803,#35804,#35805,#35806,#35807,#35808,#35809,#35810,#35811,#35812,
#35813,#35814,#35815,#35816,#35817,#35818,#35819,#35820,#35821,#35822,#35823,
#35824,#35825,#35826,#35827,#35828,#35829,#35830,#35831,#35832,#35833,#35834),
 .UNSPECIFIED.,.F.,.F.,(4,3,3,3,3,3,3,3,3,3,3,3,3,3,3,3,4),(5.35367963709457E-13,
0.11846007821872,0.125,0.242079186084241,0.25,0.367390321915038,0.375,0.492346917375386,
0.5,0.617346917375406,0.625,0.742390321915024,0.75,0.86707918608421,0.875,
0.993460078218313,1.),.UNSPECIFIED.);
#407=B_SPLINE_CURVE_WITH_KNOTS('',3,(#35838,#35839,#35840,#35841,#35842,
#35843,#35844,#35845,#35846,#35847,#35848,#35849,#35850,#35851,#35852,#35853,
#35854,#35855,#35856,#35857,#35858,#35859,#35860,#35861,#35862,#35863,#35864,
#35865,#35866,#35867,#35868,#35869,#35870,#35871,#35872,#35873,#35874,#35875,
#35876,#35877,#35878,#35879,#35880,#35881,#35882,#35883,#35884,#35885,#35886),
 .UNSPECIFIED.,.F.,.F.,(4,3,3,3,3,3,3,3,3,3,3,3,3,3,3,3,4),(0.500496609805673,
0.50390625,0.5078125,0.515625,0.53125,0.546875,0.5625,0.591671105840508,
0.59375,0.625,0.6875,0.749287235495431,0.75,0.8125,0.875,0.907000590990823,
0.999998995230263),.UNSPECIFIED.);
#408=B_SPLINE_CURVE_WITH_KNOTS('',3,(#35888,#35889,#35890,#35891,#35892,
#35893,#35894,#35895,#35896,#35897,#35898,#35899,#35900,#35901,#35902,#35903,
#35904,#35905,#35906,#35907,#35908,#35909,#35910,#35911,#35912,#35913,#35914,
#35915,#35916,#35917,#35918,#35919,#35920,#35921,#35922,#35923,#35924,#35925,
#35926,#35927,#35928,#35929,#35930,#35931,#35932,#35933,#35934,#35935,#35936,
#35937,#35938,#35939,#35940,#35941,#35942,#35943,#35944,#35945,#35946,#35947,
#35948,#35949,#35950,#35951,#35952,#35953,#35954,#35955,#35956,#35957,#35958,
#35959,#35960,#35961,#35962,#35963,#35964,#35965,#35966,#35967,#35968,#35969,
#35970,#35971,#35972,#35973,#35974,#35975,#35976,#35977,#35978,#35979,#35980,
#35981,#35982,#35983,#35984,#35985,#35986,#35987,#35988,#35989,#35990,#35991,
#35992,#35993,#35994,#35995,#35996,#35997,#35998,#35999,#36000,#36001,#36002,
#36003,#36004,#36005,#36006,#36007,#36008,#36009,#36010,#36011,#36012,#36013,
#36014,#36015,#36016,#36017,#36018,#36019,#36020,#36021,#36022,#36023,#36024,
#36025,#36026,#36027,#36028,#36029,#36030,#36031,#36032,#36033,#36034,#36035,
#36036,#36037,#36038,#36039,#36040,#36041,#36042,#36043,#36044,#36045,#36046,
#36047,#36048,#36049,#36050,#36051,#36052,#36053,#36054,#36055,#36056,#36057,
#36058,#36059,#36060,#36061,#36062,#36063,#36064,#36065,#36066,#36067,#36068,
#36069,#36070,#36071,#36072,#36073,#36074,#36075,#36076,#36077,#36078,#36079,
#36080,#36081,#36082,#36083,#36084,#36085,#36086,#36087,#36088,#36089,#36090,
#36091,#36092,#36093,#36094,#36095,#36096,#36097,#36098,#36099,#36100,#36101,
#36102,#36103,#36104,#36105,#36106,#36107,#36108,#36109,#36110,#36111,#36112,
#36113,#36114,#36115,#36116,#36117,#36118,#36119,#36120,#36121,#36122,#36123,
#36124,#36125,#36126,#36127,#36128,#36129,#36130,#36131,#36132,#36133,#36134,
#36135,#36136,#36137,#36138,#36139,#36140,#36141,#36142,#36143,#36144,#36145,
#36146,#36147,#36148,#36149,#36150,#36151,#36152,#36153,#36154,#36155,#36156,
#36157,#36158,#36159,#36160,#36161,#36162,#36163,#36164,#36165,#36166,#36167,
#36168,#36169,#36170,#36171,#36172,#36173,#36174,#36175,#36176,#36177,#36178,
#36179,#36180,#36181,#36182,#36183,#36184,#36185,#36186,#36187,#36188,#36189,
#36190,#36191,#36192,#36193,#36194,#36195,#36196,#36197,#36198,#36199,#36200,
#36201,#36202,#36203,#36204,#36205,#36206,#36207,#36208,#36209,#36210,#36211,
#36212,#36213,#36214,#36215,#36216,#36217,#36218,#36219,#36220,#36221,#36222,
#36223,#36224,#36225,#36226,#36227,#36228,#36229,#36230,#36231,#36232,#36233,
#36234,#36235,#36236,#36237,#36238,#36239,#36240,#36241,#36242,#36243,#36244,
#36245,#36246,#36247,#36248,#36249,#36250,#36251,#36252,#36253,#36254,#36255,
#36256,#36257,#36258,#36259,#36260,#36261,#36262,#36263,#36264,#36265,#36266,
#36267,#36268,#36269,#36270,#36271,#36272,#36273,#36274,#36275,#36276,#36277,
#36278,#36279,#36280,#36281,#36282,#36283,#36284,#36285,#36286,#36287,#36288,
#36289,#36290,#36291,#36292,#36293,#36294,#36295,#36296,#36297,#36298,#36299,
#36300,#36301,#36302,#36303,#36304,#36305,#36306,#36307,#36308,#36309,#36310,
#36311,#36312,#36313,#36314,#36315,#36316,#36317,#36318,#36319,#36320,#36321,
#36322,#36323,#36324,#36325,#36326,#36327,#36328,#36329,#36330,#36331,#36332,
#36333,#36334,#36335,#36336,#36337,#36338,#36339,#36340,#36341,#36342,#36343,
#36344,#36345,#36346,#36347,#36348,#36349,#36350,#36351,#36352,#36353,#36354,
#36355,#36356,#36357,#36358,#36359,#36360,#36361,#36362,#36363,#36364,#36365,
#36366,#36367,#36368,#36369,#36370,#36371,#36372,#36373,#36374,#36375,#36376,
#36377,#36378,#36379,#36380,#36381,#36382,#36383,#36384,#36385,#36386,#36387,
#36388,#36389,#36390,#36391,#36392,#36393,#36394,#36395,#36396,#36397,#36398,
#36399,#36400,#36401,#36402,#36403,#36404,#36405,#36406,#36407,#36408,#36409,
#36410,#36411,#36412,#36413,#36414,#36415,#36416,#36417,#36418,#36419,#36420,
#36421,#36422,#36423,#36424,#36425,#36426,#36427,#36428,#36429,#36430,#36431,
#36432,#36433,#36434,#36435,#36436,#36437,#36438,#36439,#36440,#36441,#36442,
#36443,#36444,#36445,#36446,#36447,#36448,#36449,#36450,#36451,#36452,#36453,
#36454,#36455,#36456,#36457,#36458,#36459,#36460,#36461,#36462,#36463,#36464,
#36465,#36466,#36467,#36468,#36469,#36470,#36471,#36472,#36473,#36474,#36475,
#36476,#36477,#36478,#36479,#36480,#36481,#36482,#36483,#36484,#36485,#36486,
#36487,#36488,#36489,#36490,#36491,#36492,#36493,#36494,#36495,#36496,#36497,
#36498,#36499,#36500,#36501,#36502,#36503,#36504,#36505,#36506,#36507,#36508,
#36509,#36510,#36511,#36512,#36513,#36514,#36515,#36516,#36517,#36518,#36519,
#36520,#36521,#36522,#36523,#36524,#36525,#36526,#36527,#36528,#36529,#36530,
#36531,#36532,#36533,#36534,#36535,#36536,#36537,#36538,#36539,#36540,#36541,
#36542,#36543,#36544,#36545,#36546,#36547,#36548,#36549,#36550,#36551,#36552,
#36553,#36554,#36555,#36556,#36557,#36558,#36559,#36560,#36561,#36562,#36563,
#36564,#36565,#36566,#36567,#36568,#36569,#36570,#36571,#36572,#36573,#36574,
#36575,#36576,#36577,#36578,#36579,#36580,#36581,#36582,#36583,#36584,#36585,
#36586,#36587,#36588,#36589,#36590,#36591,#36592,#36593,#36594,#36595,#36596,
#36597,#36598,#36599,#36600,#36601,#36602,#36603,#36604,#36605,#36606,#36607,
#36608,#36609,#36610,#36611,#36612,#36613,#36614,#36615,#36616,#36617,#36618,
#36619,#36620,#36621,#36622,#36623,#36624,#36625,#36626,#36627,#36628,#36629,
#36630,#36631,#36632,#36633,#36634,#36635,#36636,#36637,#36638,#36639,#36640,
#36641,#36642,#36643,#36644,#36645,#36646,#36647,#36648,#36649,#36650,#36651,
#36652,#36653,#36654,#36655,#36656,#36657,#36658,#36659,#36660,#36661,#36662,
#36663,#36664,#36665,#36666,#36667,#36668,#36669,#36670,#36671,#36672,#36673,
#36674,#36675,#36676,#36677,#36678,#36679,#36680,#36681,#36682,#36683,#36684,
#36685,#36686,#36687,#36688,#36689,#36690,#36691,#36692,#36693,#36694,#36695,
#36696,#36697,#36698,#36699,#36700,#36701,#36702,#36703,#36704,#36705,#36706,
#36707,#36708,#36709,#36710,#36711,#36712,#36713,#36714,#36715,#36716,#36717,
#36718,#36719,#36720,#36721,#36722,#36723,#36724,#36725,#36726,#36727,#36728,
#36729,#36730,#36731,#36732,#36733,#36734,#36735,#36736,#36737,#36738,#36739,
#36740,#36741,#36742,#36743,#36744,#36745,#36746,#36747,#36748,#36749,#36750,
#36751,#36752,#36753,#36754,#36755,#36756,#36757,#36758,#36759,#36760,#36761,
#36762,#36763,#36764,#36765,#36766,#36767,#36768,#36769,#36770,#36771,#36772,
#36773,#36774,#36775,#36776,#36777,#36778,#36779,#36780,#36781,#36782,#36783,
#36784,#36785,#36786,#36787,#36788,#36789,#36790,#36791,#36792,#36793,#36794,
#36795,#36796,#36797,#36798,#36799,#36800,#36801,#36802,#36803,#36804,#36805,
#36806,#36807,#36808,#36809,#36810,#36811,#36812,#36813,#36814,#36815,#36816,
#36817,#36818,#36819,#36820,#36821,#36822,#36823,#36824,#36825,#36826,#36827,
#36828,#36829,#36830,#36831,#36832,#36833),.UNSPECIFIED.,.F.,.F.,(4,2,2,
2,2,2,2,2,2,2,2,2,2,2,2,2,2,2,2,2,2,2,2,2,2,2,2,2,2,2,2,2,2,2,2,2,2,2,2,
2,2,2,2,2,2,2,2,2,2,2,2,2,2,2,2,2,2,2,2,2,2,2,2,2,2,2,2,2,2,2,2,2,2,2,2,
2,2,2,2,2,2,2,2,2,2,2,2,2,2,2,2,2,2,2,2,2,2,2,2,2,2,2,2,2,2,2,2,2,2,2,2,
2,2,2,2,2,2,2,2,2,2,2,2,2,2,2,2,2,2,2,2,2,2,2,2,2,2,2,2,2,2,2,2,2,2,2,2,
2,2,2,2,2,2,2,2,2,2,2,2,2,2,2,2,2,2,2,2,2,2,2,2,2,2,2,2,2,2,2,2,2,2,2,2,
2,2,2,2,2,2,2,2,2,2,2,2,2,2,2,2,2,2,2,2,2,2,2,2,2,2,2,2,2,2,2,2,2,2,2,2,
2,2,2,2,2,2,2,2,2,2,2,2,2,2,2,2,2,2,2,2,2,2,2,2,2,2,2,2,2,2,2,2,2,2,2,2,
2,2,2,2,2,2,2,2,2,2,2,2,2,2,2,2,2,2,2,2,2,2,2,2,2,2,2,2,2,2,2,2,2,2,2,2,
2,2,2,2,2,2,2,2,2,2,2,2,2,2,2,2,2,2,2,2,2,2,2,2,2,2,2,2,2,2,2,2,2,2,2,2,
2,2,2,2,2,2,2,2,2,2,2,2,2,2,2,2,2,2,2,2,2,2,2,2,2,2,2,2,2,2,2,2,2,2,2,2,
2,2,2,2,2,2,2,2,2,2,2,2,2,2,2,2,2,2,2,2,2,2,2,2,2,2,2,2,2,2,2,2,2,2,2,2,
2,2,2,2,2,2,2,2,2,2,2,2,2,2,2,2,2,2,2,2,2,2,2,2,2,2,2,2,2,2,2,2,2,2,2,2,
2,2,2,2,2,2,2,2,2,2,2,2,2,2,2,2,2,2,2,2,2,2,2,2,2,2,2,2,2,2,2,2,2,2,2,2,
2,4),(0.000313237606796583,0.0732396125606311,0.107388601669689,0.116229997177897,
0.120739200951735,0.12448068829046,0.12932232799047,0.140221656971463,0.197481902428677,
0.242183482957304,0.258897773384315,0.267128547630496,0.273754482371197,
0.281405825657101,0.294762578788611,0.359832446620594,0.392697716411196,
0.410524918994634,0.416397219067249,0.420282279646255,0.423842780221686,
0.43003701160593,0.449122813102218,0.499312016373005,0.532450329898909,
0.554251024099348,0.563329965988381,0.570055283822999,0.577253748747926,
0.588794905730077,0.63783386640416,0.68555064429509,0.700318391868383,0.71074492774884,
0.715554302770943,0.719289105967843,0.723890692170196,0.733204015963814,
0.775297264573541,0.813397616482522,0.836829411115005,0.854004311242021,
0.862319189947006,0.868890720456341,0.876460021720684,0.889436588905798,
0.958064649980759,0.988901173792772,1.00605964200919,1.01185486548237,1.01572483607133,
1.01981038743091,1.02662506481103,1.05294308186016,1.11603960015384,1.13681639290964,
1.15255038391308,1.16059722623153,1.16657003890367,1.17412248481406,1.18702187013861,
1.26634207907997,1.29860430761864,1.30722407958094,1.31168903283532,1.31543564929409,
1.32033674769295,1.3315838632717,1.38851310549199,1.43301151510683,1.44974680322203,
1.45798167437105,1.46460815319793,1.47225708342722,1.48560161688953,1.5508096408345,
1.58359577756807,1.60139783967576,1.60726747808697,1.61115213976924,1.61471343822002,
1.62091124413417,1.64002901256489,1.69019703923327,1.72332762695399,1.74512535184184,
1.75420411351427,1.76092964789903,1.76812867093258,1.77967145331808,1.82873709616104,
1.87643479990973,1.89120007939844,1.90162546861717,1.906434770132,1.9101697274484,
1.91477176451421,1.92408679796526,1.96636127139429,2.00482306070261,2.02795782992859,
2.0449757045374,2.05326230394008,2.05989243997341,2.06750403665759,2.08067525344837,
2.14761187164537,2.17939332316874,2.19686781230856,2.20270002240954,2.20657731262491,
2.21014682013202,2.21638708153345,2.23591442338624,2.28577745846129,2.33125256327586,
2.3448634669727,2.35249097721753,2.35911945320565,2.36738364623431,2.38048505743541,
2.45126394470639,2.491824698676,2.4990749260843,2.50325459238726,2.50703244418594,
2.51165892580978,2.5230138751059,2.57957652125262,2.62385667981512,2.640608277974,
2.64884637960265,2.65547334481351,2.66312050416494,2.67645581165643,2.74177291493049,
2.77449742393239,2.7922799505251,2.79814754898393,2.80203192776873,2.80559387940277,
2.81179453066218,2.83093749953759,2.88108952277184,2.91421444333614,2.93601008099111,
2.94508878799329,2.95181455092315,2.95901406896798,2.97055820458558,3.01964431923071,
3.06732837603487,3.08209198747141,3.09251664138888,3.09732594073853,3.10106105597637,
3.1056634855733,3.11497990222459,3.15743985639091,3.21906433038732,3.23596923937728,
3.24423525632709,3.25080307478489,3.25840680359813,3.2715414761115,3.33881303289814,
3.37040526765403,3.38781716509415,3.39364215558881,3.39751804612596,3.40108919541907,
3.40733786232631,3.426948013979,3.48278666763428,3.51842522126189,3.53429071536459,
3.54236291286626,3.5483383589686,3.55587295299742,3.56868876036549,3.64839732381433,
3.68047143337749,3.68906884053197,3.6935294641211,3.69727691731241,3.70218474989,
3.71347069177186,3.77036733262433,3.81484680103362,3.83158489220578,3.83982060803806,
3.84644753088318,3.85409671343685,3.86744100221539,3.93266508916591,3.96544623029879,
3.98324714544429,3.98911689971542,3.99300175767898,3.99656333766215,4.0027618249125,
4.02188353105887,4.07205271143324,4.10518460928008,4.12698337883407,4.13606266588215,
4.14278861918699,4.14998811824146,4.16153172542411,4.21060248968077,4.25830151837033,
4.2730674850971,4.28349340724766,4.28830299066872,4.29203818429792,4.29664053409124,
4.30595626291475,4.34934748303688,4.39619782041856,4.41434929080584,4.42857812647288,
4.43633085160234,4.4429505060573,4.45105416420926,4.46359846997177,4.52012220950349,
4.55871685980115,4.57197906541737,4.58161223716024,4.58627531352348,4.5896388918647,
4.59418922081277,4.6032378874983,4.65583263761798,4.69656653463468,4.72135568666745,
4.730856601774,4.73758480567342,4.74462888557875,4.75541960666407,4.79288568239407,
4.82885445160377,4.87344626915557,4.88080474789728,4.88500753632564,4.88881892169032,
4.89429083248362,4.90891007740531,4.93287264334698,5.01162740766663,5.02465998817305,
5.03224150521685,5.03881164645255,5.04710891455437,5.06418654928975,5.08743200694948,
5.12585309495423,5.16790924677788,5.17722081086339,5.18182206712108,5.18555689260041,
5.19036670092958,5.20079548702653,5.21556888747791,5.26331057623244,5.31236987823311,
5.32391216753674,5.33111087790344,5.33783609047363,5.34691438697375,5.36871160436141,
5.40183944885928,5.45201633410622,5.47107788044713,5.47726931209096,5.48082925358337,
5.48471473812841,5.49058942437643,5.50843711943276,5.54136693322142,5.60638140494845,
5.6197470670641,5.62740026155646,5.63402591022171,5.64225388314361,5.65895372302928,
5.70370953468402,5.76105341546906,5.77079415343036,5.77555639304346,5.7793664111699,
5.78347665201096,5.79040604229506,5.82198915488222,5.8857049079595,5.91128857237193,
5.9211610784852,5.92733794405061,5.93417624848413,5.94391888997028,5.97061846915713,
6.01703809091761,6.06096967345059,6.0702767349235,6.07487690866175,6.07861148482227,
6.08342177761782,6.09385448693531,6.10863590921031,6.15643602560443,6.20541939886094,
6.21695774531404,6.22415527180339,6.23088023313038,6.23995951770358,6.261766258068,
6.29491770242867,6.34515755983286,6.36412883642266,6.37031032870974,6.3738681807214,
6.37775507522321,6.38363788156199,6.40156027295113,6.43472527589361,6.49934039243712,
6.51273957205739,6.52039961020333,6.52702412278388,6.53524154289608,6.55188625378585,
6.5967321111915,6.65408992772509,6.66381299538236,6.66857090801069,6.67237964758556,
6.67649143080277,6.68342886648739,6.71518648574016,6.77978011830595,6.80455227971896,
6.81430962319356,6.82108212878374,6.82805754263332,6.83851346682056,6.87195972478911,
6.95215361079866,6.96269806089745,6.96752838705944,6.97126383418314,6.97584690258443,
6.98506573626334,7.02263603588288,7.09433868882286,7.10799292718832,7.11570737876551,
7.12232755374372,7.13047392861467,7.14673772581042,7.20925409112281,7.25175036210626,
7.26106350359465,7.26566474748929,7.26939912698676,7.27420780311051,7.28463214639486,
7.29939754904456,7.34709095519899,7.39619443290078,7.40773763475398,7.4149359919494,
7.42166025661953,7.43073631439035,7.4525229928785,7.48562823741736,7.53575129037795,
7.55487486475011,7.56107238851728,7.56463323392608,7.56851706622811,7.57438498142335,
7.59217665456648,7.62493481732375,7.69022330462129,7.70356180776332,7.71120861885677,
7.71783400362131,7.72606848306152,7.74280685165591,7.78714839928332,7.84382330403291,
7.85529557183305,7.86023376188207,7.8639833645544,7.86842058678017,7.87690577738169,
7.88810374115488,7.91676560401724,7.98957914746058,8.00215087631491,8.00956315584407,
8.01622251652062,8.02482648592442,8.04365816094504,8.07033861727407,8.10460906787267,
8.14806363667771,8.15537705237786,8.15956945765984,8.16338350099015,8.16887609108397,
8.18365337250209,8.20801392577201,8.28573096649293,8.29897840424588,8.30660499365386,
8.31323133193775,8.32149111057444,8.33837102002009,8.38106655106261,8.4352194528517,
8.44928421307062,8.45482389939674,8.45860817415939,8.46276801406585,8.46993053964016,
8.50739522920647,8.56970187884935,8.59163513100119,8.60096217952688,8.60772586212575,
8.61483428769196,8.62594833814482,8.66832213642274,8.68365072489435,8.74111159240067,
8.7496274961707,8.75412329755277,8.75786472642003,8.76280357698595,8.77397110823675,
8.79020879126153,8.84939545791893,8.88566667308928,8.89658894894715,8.90365793660862,
8.91044347639736,8.91989866627855,8.94436484759657,8.98422036065577,9.03835238060195,
9.04708268240285,9.05162363084941,9.05532514558369,9.06018348337513,9.07088942244905,
9.08620626270874,9.13783286586151,9.18237623172095,9.19373048934184,9.20088857749546,
9.20762799411705,9.21680752646988,9.23930234293591,9.27409640251205,9.32864526177467,
9.34224801874259,9.34771243020849,9.35152134447465,9.35572449427036,9.36308997113074,
9.41097147200668,9.44274043488676),.UNSPECIFIED.);
#409=B_SPLINE_CURVE_WITH_KNOTS('',3,(#36835,#36836,#36837,#36838,#36839,
#36840,#36841,#36842,#36843,#36844,#36845,#36846,#36847,#36848,#36849,#36850,
#36851,#36852,#36853,#36854,#36855,#36856,#36857,#36858,#36859,#36860,#36861,
#36862,#36863,#36864,#36865,#36866,#36867,#36868,#36869,#36870,#36871,#36872,
#36873,#36874,#36875,#36876,#36877,#36878,#36879,#36880,#36881,#36882,#36883,
#36884,#36885,#36886,#36887,#36888,#36889,#36890,#36891,#36892,#36893,#36894,
#36895,#36896,#36897,#36898,#36899,#36900,#36901,#36902,#36903,#36904,#36905,
#36906,#36907,#36908,#36909,#36910,#36911,#36912,#36913,#36914,#36915,#36916,
#36917,#36918,#36919,#36920,#36921,#36922,#36923,#36924,#36925,#36926,#36927,
#36928,#36929,#36930,#36931,#36932,#36933,#36934,#36935,#36936,#36937,#36938,
#36939,#36940,#36941,#36942,#36943,#36944,#36945,#36946,#36947,#36948,#36949,
#36950,#36951,#36952,#36953,#36954,#36955,#36956,#36957,#36958,#36959,#36960,
#36961,#36962,#36963,#36964,#36965,#36966,#36967,#36968,#36969,#36970,#36971,
#36972,#36973,#36974,#36975,#36976,#36977,#36978,#36979,#36980,#36981,#36982,
#36983,#36984,#36985,#36986,#36987,#36988,#36989,#36990,#36991,#36992,#36993,
#36994,#36995,#36996,#36997,#36998,#36999,#37000,#37001,#37002,#37003,#37004,
#37005,#37006,#37007,#37008,#37009,#37010,#37011,#37012,#37013,#37014,#37015,
#37016,#37017,#37018,#37019,#37020,#37021,#37022,#37023,#37024,#37025,#37026,
#37027,#37028,#37029,#37030,#37031,#37032,#37033,#37034,#37035,#37036,#37037,
#37038,#37039,#37040,#37041,#37042,#37043,#37044,#37045,#37046,#37047,#37048,
#37049,#37050,#37051,#37052,#37053,#37054,#37055,#37056,#37057,#37058,#37059,
#37060,#37061,#37062,#37063,#37064,#37065,#37066,#37067,#37068,#37069,#37070,
#37071,#37072,#37073,#37074,#37075,#37076,#37077,#37078,#37079,#37080,#37081,
#37082,#37083,#37084,#37085,#37086,#37087,#37088,#37089,#37090,#37091,#37092,
#37093,#37094,#37095,#37096,#37097,#37098,#37099,#37100,#37101,#37102,#37103,
#37104,#37105,#37106,#37107,#37108,#37109,#37110,#37111,#37112,#37113,#37114,
#37115,#37116,#37117,#37118,#37119,#37120,#37121,#37122,#37123,#37124,#37125,
#37126,#37127,#37128,#37129,#37130,#37131,#37132,#37133,#37134,#37135,#37136,
#37137,#37138,#37139,#37140,#37141,#37142,#37143,#37144,#37145,#37146,#37147,
#37148,#37149,#37150,#37151,#37152,#37153,#37154,#37155,#37156,#37157,#37158,
#37159,#37160,#37161,#37162,#37163,#37164,#37165,#37166,#37167,#37168,#37169,
#37170,#37171,#37172,#37173,#37174,#37175,#37176,#37177,#37178,#37179,#37180,
#37181,#37182,#37183,#37184,#37185,#37186,#37187,#37188,#37189,#37190,#37191,
#37192,#37193,#37194,#37195,#37196,#37197,#37198,#37199,#37200,#37201,#37202,
#37203,#37204,#37205,#37206,#37207,#37208,#37209,#37210,#37211,#37212,#37213,
#37214,#37215,#37216,#37217,#37218,#37219,#37220,#37221,#37222,#37223,#37224),
 .UNSPECIFIED.,.F.,.F.,(4,2,2,2,2,2,2,2,2,2,2,2,2,2,2,2,2,2,2,2,2,2,2,2,
2,2,2,2,2,2,2,2,2,2,2,2,2,2,2,2,2,2,2,2,2,2,2,2,2,2,2,2,2,2,2,2,2,2,2,2,
2,2,2,2,2,2,2,2,2,2,2,2,2,2,2,2,2,2,2,2,2,2,2,2,2,2,2,2,2,2,2,2,2,2,2,2,
2,2,2,2,2,2,2,2,2,2,2,2,2,2,2,2,2,2,2,2,2,2,2,2,2,2,2,2,2,2,2,2,2,2,2,2,
2,2,2,2,2,2,2,2,2,2,2,2,2,2,2,2,2,2,2,2,2,2,2,2,2,2,2,2,2,2,2,2,2,2,2,2,
2,2,2,2,2,2,2,2,2,2,2,2,2,2,2,2,2,2,2,2,2,2,2,2,2,2,4),(9.99999999526152E-7,
0.02541508705979,0.0403509785521346,0.0478988957842898,0.0541473169418411,
0.0607715627350446,0.0689794030361682,0.0850231306095784,0.140555435079713,
0.173585934480102,0.188350097916006,0.198774669984789,0.203583572743684,
0.20731820680062,0.211919827642413,0.221233979609255,0.264646346264958,
0.311470042953097,0.329614886335042,0.343839280917871,0.35159037156107,
0.35820904340011,0.366312017366255,0.378856297343035,0.435269542521666,
0.473931972186144,0.49349270960845,0.499550744538113,0.503473421030138,
0.506997351234623,0.512999204789748,0.53040898313939,0.581879644126399,
0.623712128187474,0.640123710024594,0.648298060722711,0.654920127170653,
0.662613387749988,0.67616713643093,0.738608872800642,0.773101424473421,
0.791440449153294,0.797369422545081,0.80126564039814,0.804814062124252,
0.810945956436549,0.829461537871561,0.886330892904588,0.921781420161633,
0.937943429823994,0.946071029843745,0.952690622809616,0.960421006174729,
0.97414880871105,1.03185979384175,1.06958924070581,1.08268946443784,1.09223470828921,
1.09688056522918,1.10024265388201,1.1048070309001,1.11393025772448,1.1799559966417,
1.21189033405176,1.2331676438347,1.24216632496867,1.24887863916426,1.25610686702012,
1.26779453972329,1.31837403481817,1.35636457635536,1.38506419660503,1.39183807772474,
1.39591435594572,1.39974303726536,1.40552566248542,1.42124676978749,1.47406019861245,
1.50820862862716,1.53043596827541,1.5395775531375,1.54631192021341,1.55348559060862,
1.56491065125921,1.60926620515102,1.66090596941392,1.67622375644931,1.68693143540261,
1.69179065888691,1.69549305560627,1.70003539947624,1.70876887097193,1.76293424303464,
1.80280979026846,1.82728429692332,1.83674210724431,1.84352928172483,1.84976015883669,
1.8599462518553,1.88823141575172,1.94179659623945,1.97943655892693,1.98669149214734,
1.99087159173205,1.99469084996073,2.00021440726323,2.01522176968697,2.04016382138305,
2.1164765391538,2.13002112034464,2.13771127091191,2.14433177541148,2.15250559103361,
2.16892119780121,2.21093710449602,2.26274000132455,2.27967966095738,2.28562176463385,
2.28913403699085,2.29306869599499,2.29918716107689,2.31935976452665,2.36028657690867,
2.41367472917936,2.42626028226952,2.43437464521228,2.44099296215536,2.44873263999628,
2.46290364477065,2.48095745045831,2.52734101885416,2.57129836700053,2.58060409495587,
2.58520405916938,2.58893983523734,2.59375359411506,2.6041978076728,2.6190006463112,
2.66695430111742,2.71567951130462,2.72720795203295,2.73440477612739,2.7411329213571,
2.75022265791473,2.77208905832678,2.80537678018994,2.85596265538789,2.87447221987865,
2.88060315926801,2.88415128178029,2.88804330123993,2.89396506363409,2.91227355281239,
2.94667645633749,3.00935373112116,3.02289418062897,3.03057962783057,3.03719446225264,
3.04535893359252,3.06174596062229,3.10327548774194,3.15420939777526,3.17226518965298,
3.17834083402444,3.18187622467,3.18577996015993,3.19175249373992,3.21050493335888,
3.24635311542894,3.30691938175137,3.32057951640045,3.3282967358863,3.33491892847784,
3.34306739813751,3.35933488529976,3.42197603469795,3.46418131911456,3.47353803357934,
3.47815099013026,3.48189654725739,3.48672299886183,3.49718158689922,3.51200355480281,
3.56010114755446,3.60825547711487,3.6197700369559,3.62697430206707,3.63372116635705,
3.64285552699046,3.66494112643857,3.69871103664215,3.76234943713865,3.77115339485521,
3.77402045671866,3.77647229296193),.UNSPECIFIED.);
#410=B_SPLINE_CURVE_WITH_KNOTS('',3,(#37226,#37227,#37228,#37229,#37230,
#37231,#37232,#37233,#37234,#37235,#37236,#37237,#37238,#37239,#37240,#37241,
#37242,#37243,#37244,#37245,#37246,#37247,#37248,#37249,#37250,#37251,#37252,
#37253,#37254,#37255,#37256,#37257,#37258,#37259,#37260,#37261,#37262,#37263,
#37264,#37265,#37266,#37267,#37268,#37269,#37270,#37271,#37272,#37273,#37274,
#37275,#37276,#37277,#37278,#37279,#37280,#37281,#37282,#37283,#37284,#37285,
#37286,#37287,#37288,#37289,#37290,#37291,#37292,#37293,#37294,#37295,#37296,
#37297,#37298,#37299,#37300,#37301,#37302,#37303,#37304,#37305,#37306,#37307,
#37308,#37309,#37310,#37311,#37312,#37313,#37314,#37315,#37316,#37317,#37318,
#37319,#37320,#37321,#37322,#37323,#37324,#37325,#37326,#37327),
 .UNSPECIFIED.,.F.,.F.,(4,2,2,2,2,2,2,2,2,2,2,2,2,2,2,2,2,2,2,2,2,2,2,2,
2,2,2,2,2,2,2,2,2,2,2,2,2,2,2,2,2,2,2,2,2,2,2,2,2,2,4),(0.000274590634593237,
0.0025082762786118,0.00535069727310344,0.0116844857126863,0.0342991856608529,
0.0843016193333742,0.115297757508164,0.136139369508367,0.145022650646858,
0.151667283405926,0.158837468056138,0.170458820756428,0.221014938736121,
0.267413615605875,0.281958972332198,0.292254398082525,0.297016468905675,
0.300730962418017,0.305324808844561,0.314619905230995,0.357647295962238,
0.419422814912621,0.436370390294811,0.444655812784192,0.451299173082329,
0.458941834237123,0.472211170200764,0.516280100710487,0.546464638149321,
0.58483144266112,0.59212456635804,0.596333234407501,0.600256784222936,0.605985302348148,
0.621931521037642,0.649320403068425,0.720955334511645,0.733274317749864,
0.740699761065403,0.747479592700835,0.756403816803348,0.776727475649347,
0.804043104311228,0.856916121248536,0.88117922472343,0.887847382211191,
0.891895834338558,0.895605417154939,0.899318875233909,0.904616105327427,
0.944316620293279),.UNSPECIFIED.);
#411=B_SPLINE_CURVE_WITH_KNOTS('',3,(#37331,#37332,#37333,#37334,#37335,
#37336,#37337),.UNSPECIFIED.,.F.,.F.,(4,1,1,1,4),(0.,0.25,0.5,0.75,1.),
 .UNSPECIFIED.);
#412=B_SPLINE_CURVE_WITH_KNOTS('',3,(#37339,#37340,#37341,#37342,#37343,
#37344,#37345,#37346,#37347,#37348,#37349,#37350,#37351,#37352,#37353,#37354,
#37355,#37356,#37357,#37358,#37359,#37360,#37361,#37362,#37363,#37364,#37365,
#37366,#37367,#37368,#37369,#37370,#37371,#37372,#37373,#37374,#37375,#37376,
#37377,#37378,#37379,#37380,#37381,#37382,#37383,#37384,#37385,#37386,#37387,
#37388,#37389,#37390,#37391,#37392,#37393,#37394,#37395,#37396,#37397,#37398,
#37399,#37400,#37401,#37402,#37403,#37404,#37405,#37406,#37407,#37408,#37409,
#37410,#37411,#37412,#37413,#37414,#37415,#37416,#37417,#37418,#37419,#37420,
#37421,#37422,#37423,#37424,#37425,#37426,#37427,#37428,#37429),
 .UNSPECIFIED.,.F.,.F.,(4,3,3,3,3,3,3,3,3,3,3,3,3,3,3,3,3,3,3,3,3,3,3,3,
3,3,3,3,3,3,4),(1.01781475985858E-6,0.0978279187980743,0.125,0.1875,0.25,
0.255532112875372,0.3125,0.375,0.40625,0.413169433494558,0.4375,0.46875,
0.484375,0.4921875,0.5,0.5078125,0.515625,0.53125,0.5625,0.59375,0.625,
0.627666778982696,0.6875,0.75,0.800182159962401,0.8125,0.875,0.924421520907667,
0.9375,0.992828832419945,0.999999605898017),.UNSPECIFIED.);
#413=B_SPLINE_CURVE_WITH_KNOTS('',3,(#37431,#37432,#37433,#37434,#37435,
#37436,#37437,#37438,#37439,#37440,#37441,#37442,#37443,#37444,#37445,#37446,
#37447,#37448,#37449,#37450,#37451,#37452,#37453,#37454,#37455,#37456,#37457,
#37458,#37459,#37460,#37461,#37462,#37463,#37464,#37465,#37466,#37467,#37468,
#37469,#37470,#37471,#37472,#37473,#37474,#37475,#37476,#37477,#37478,#37479),
 .UNSPECIFIED.,.F.,.F.,(4,3,3,3,3,3,3,3,3,3,3,3,3,3,3,3,4),(0.,0.0886352608471135,
0.125,0.212002569513292,0.25,0.33732431895677,0.375,0.462307893887243,0.5,
0.587307893887231,0.625,0.712324318956778,0.75,0.837002569513291,0.875,
0.963635260847104,1.),.UNSPECIFIED.);
#414=B_SPLINE_CURVE_WITH_KNOTS('',3,(#37481,#37482,#37483,#37484,#37485,
#37486,#37487,#37488,#37489,#37490,#37491,#37492,#37493,#37494,#37495,#37496,
#37497,#37498,#37499,#37500,#37501,#37502,#37503,#37504,#37505,#37506,#37507,
#37508,#37509,#37510,#37511,#37512,#37513,#37514,#37515,#37516,#37517,#37518,
#37519,#37520,#37521,#37522,#37523,#37524,#37525,#37526,#37527,#37528,#37529),
 .UNSPECIFIED.,.F.,.F.,(4,3,3,3,3,3,3,3,3,3,3,3,3,3,3,3,4),(0.,0.0886238521664878,
0.125,0.211990985604023,0.25,0.337312738768364,0.375,0.462296334182994,
0.5,0.587296334182989,0.625,0.71231273876836,0.75,0.836990985604029,0.875,
0.96362385216648,1.),.UNSPECIFIED.);
#415=B_SPLINE_CURVE_WITH_KNOTS('',3,(#37531,#37532,#37533,#37534,#37535,
#37536,#37537,#37538,#37539,#37540,#37541,#37542,#37543,#37544,#37545,#37546,
#37547,#37548,#37549,#37550,#37551,#37552,#37553,#37554,#37555,#37556,#37557,
#37558,#37559,#37560,#37561,#37562,#37563,#37564,#37565,#37566,#37567,#37568,
#37569,#37570,#37571,#37572,#37573,#37574,#37575,#37576,#37577,#37578,#37579),
 .UNSPECIFIED.,.F.,.F.,(4,3,3,3,3,3,3,3,3,3,3,3,3,3,3,3,4),(1.00099247898549E-6,
0.0886113417660512,0.125,0.211978963112827,0.25,0.337305507603416,0.375,
0.462245106775286,0.5,0.587333725456046,0.625,0.712305984259491,0.75,0.836989030990787,
0.875,0.963623492160247,0.999999791341556),.UNSPECIFIED.);
#416=B_SPLINE_CURVE_WITH_KNOTS('',3,(#37581,#37582,#37583,#37584,#37585,
#37586,#37587,#37588,#37589,#37590,#37591,#37592,#37593,#37594,#37595,#37596,
#37597,#37598,#37599,#37600,#37601,#37602,#37603,#37604,#37605,#37606,#37607,
#37608,#37609,#37610,#37611,#37612,#37613,#37614,#37615,#37616,#37617,#37618,
#37619,#37620,#37621,#37622,#37623,#37624,#37625,#37626,#37627,#37628,#37629),
 .UNSPECIFIED.,.F.,.F.,(4,3,3,3,3,3,3,3,3,3,3,3,3,3,3,3,4),(0.,0.0886378390083851,
0.125,0.212005187268809,0.25,0.337326935869751,0.375,0.462310506172766,
0.5,0.587310506172741,0.625,0.712326935869763,0.75,0.837005187268801,0.875,
0.963637839008402,1.),.UNSPECIFIED.);
#417=B_SPLINE_CURVE_WITH_KNOTS('',3,(#37631,#37632,#37633,#37634,#37635,
#37636,#37637,#37638,#37639,#37640,#37641,#37642,#37643,#37644,#37645,#37646,
#37647,#37648,#37649,#37650,#37651,#37652,#37653,#37654,#37655,#37656,#37657,
#37658,#37659,#37660,#37661,#37662,#37663,#37664,#37665,#37666,#37667,#37668,
#37669,#37670,#37671,#37672,#37673,#37674,#37675,#37676,#37677,#37678,#37679),
 .UNSPECIFIED.,.F.,.F.,(4,3,3,3,3,3,3,3,3,3,3,3,3,3,3,3,4),(0.,0.0886216790948839,
0.125,0.211988779152122,0.25,0.337310533023806,0.375,0.462294132341469,
0.5,0.58729413234147,0.625,0.712310533023803,0.75,0.836988779152123,0.875,
0.963621679094858,1.),.UNSPECIFIED.);
#418=B_SPLINE_CURVE_WITH_KNOTS('',3,(#37681,#37682,#37683,#37684,#37685,
#37686,#37687,#37688,#37689,#37690,#37691,#37692,#37693,#37694,#37695,#37696,
#37697,#37698,#37699,#37700,#37701,#37702,#37703,#37704,#37705,#37706,#37707,
#37708,#37709,#37710,#37711,#37712,#37713,#37714,#37715,#37716,#37717,#37718,
#37719,#37720,#37721,#37722,#37723,#37724,#37725,#37726,#37727,#37728,#37729),
 .UNSPECIFIED.,.F.,.F.,(4,3,3,3,3,3,3,3,3,3,3,3,3,3,3,3,4),(7.23012916031714E-7,
0.0886177045235499,0.125,0.211984073096313,0.25,0.337305828475216,0.375,
0.462289436118893,0.5,0.5872894361189,0.625,0.712305828475213,0.75,0.836984073096328,
0.875,0.963617044238319,1.),.UNSPECIFIED.);
#419=B_SPLINE_CURVE_WITH_KNOTS('',3,(#37731,#37732,#37733,#37734,#37735,
#37736,#37737,#37738,#37739,#37740,#37741,#37742,#37743,#37744,#37745,#37746,
#37747,#37748,#37749,#37750,#37751,#37752,#37753,#37754,#37755,#37756,#37757,
#37758,#37759,#37760,#37761,#37762,#37763,#37764,#37765,#37766,#37767,#37768,
#37769,#37770,#37771,#37772,#37773,#37774,#37775,#37776,#37777,#37778,#37779),
 .UNSPECIFIED.,.F.,.F.,(4,3,3,3,3,3,3,3,3,3,3,3,3,3,3,3,4),(0.,0.0886395817675682,
0.125,0.212006956791507,0.25,0.337328704822608,0.375,0.462312271997881,
0.5,0.587312271997905,0.625,0.712328704822597,0.75,0.837006956791513,0.875,
0.963639581767539,1.),.UNSPECIFIED.);
#420=B_SPLINE_CURVE_WITH_KNOTS('',3,(#37781,#37782,#37783,#37784,#37785,
#37786,#37787,#37788,#37789,#37790,#37791,#37792,#37793,#37794,#37795,#37796,
#37797,#37798,#37799,#37800,#37801,#37802,#37803,#37804,#37805,#37806,#37807,
#37808,#37809,#37810,#37811,#37812,#37813,#37814,#37815,#37816,#37817,#37818,
#37819,#37820,#37821,#37822,#37823,#37824,#37825,#37826,#37827,#37828,#37829),
 .UNSPECIFIED.,.F.,.F.,(4,3,3,3,3,3,3,3,3,3,3,3,3,3,3,3,4),(0.,0.0886188875000415,
0.125,0.211985944674266,0.25,0.337307699454002,0.375,0.462291303786219,
0.5,0.587291303786234,0.625,0.712307699453993,0.75,0.836985944674267,0.875,
0.963618887500054,1.),.UNSPECIFIED.);
#421=B_SPLINE_CURVE_WITH_KNOTS('',3,(#37831,#37832,#37833,#37834,#37835,
#37836,#37837,#37838,#37839,#37840,#37841,#37842,#37843,#37844,#37845,#37846,
#37847,#37848,#37849,#37850,#37851,#37852),.UNSPECIFIED.,.F.,.F.,(4,3,3,
3,3,3,3,4),(8.83577889380245E-7,0.195536634947496,0.25,0.5,0.566780896033298,
0.75,0.937584669068563,1.),.UNSPECIFIED.);
#422=B_SPLINE_CURVE_WITH_KNOTS('',3,(#37856,#37857,#37858,#37859,#37860,
#37861,#37862,#37863,#37864,#37865,#37866,#37867,#37868,#37869,#37870,#37871,
#37872,#37873,#37874,#37875,#37876,#37877,#37878,#37879,#37880,#37881,#37882,
#37883,#37884,#37885,#37886,#37887,#37888,#37889,#37890,#37891,#37892,#37893,
#37894,#37895,#37896,#37897,#37898,#37899,#37900,#37901,#37902,#37903,#37904,
#37905,#37906,#37907,#37908,#37909,#37910,#37911,#37912,#37913,#37914,#37915,
#37916,#37917,#37918,#37919,#37920,#37921,#37922,#37923,#37924,#37925,#37926,
#37927,#37928,#37929,#37930,#37931,#37932,#37933,#37934,#37935,#37936,#37937,
#37938,#37939,#37940,#37941,#37942,#37943,#37944,#37945,#37946,#37947,#37948,
#37949,#37950,#37951,#37952,#37953,#37954,#37955,#37956,#37957,#37958,#37959,
#37960,#37961,#37962,#37963,#37964,#37965,#37966,#37967,#37968,#37969,#37970,
#37971,#37972,#37973,#37974,#37975,#37976,#37977,#37978,#37979,#37980,#37981,
#37982,#37983,#37984,#37985,#37986,#37987,#37988,#37989,#37990,#37991,#37992,
#37993,#37994,#37995,#37996,#37997,#37998,#37999,#38000,#38001,#38002,#38003,
#38004,#38005,#38006,#38007,#38008,#38009,#38010,#38011,#38012,#38013,#38014,
#38015,#38016,#38017,#38018,#38019,#38020,#38021,#38022,#38023,#38024,#38025,
#38026,#38027,#38028,#38029,#38030,#38031,#38032,#38033,#38034,#38035,#38036,
#38037,#38038,#38039,#38040,#38041,#38042,#38043,#38044,#38045,#38046,#38047,
#38048,#38049,#38050,#38051,#38052,#38053,#38054,#38055,#38056,#38057,#38058,
#38059,#38060,#38061,#38062,#38063,#38064,#38065,#38066,#38067,#38068,#38069,
#38070,#38071,#38072,#38073,#38074,#38075,#38076,#38077,#38078,#38079,#38080,
#38081,#38082,#38083,#38084,#38085,#38086,#38087,#38088,#38089,#38090,#38091,
#38092,#38093,#38094,#38095,#38096,#38097,#38098,#38099,#38100,#38101,#38102,
#38103,#38104,#38105,#38106,#38107,#38108,#38109,#38110,#38111,#38112,#38113,
#38114,#38115,#38116,#38117,#38118,#38119,#38120,#38121,#38122,#38123,#38124,
#38125,#38126,#38127,#38128,#38129,#38130,#38131,#38132,#38133,#38134,#38135,
#38136,#38137,#38138,#38139,#38140,#38141,#38142,#38143,#38144,#38145,#38146,
#38147,#38148,#38149,#38150,#38151,#38152,#38153,#38154,#38155,#38156,#38157,
#38158,#38159,#38160,#38161,#38162,#38163,#38164,#38165,#38166,#38167,#38168,
#38169,#38170,#38171,#38172,#38173,#38174,#38175,#38176,#38177,#38178,#38179,
#38180,#38181,#38182,#38183,#38184,#38185,#38186,#38187,#38188,#38189,#38190,
#38191,#38192,#38193,#38194,#38195,#38196,#38197),.UNSPECIFIED.,.F.,.F.,
(4,2,2,2,2,2,2,2,2,2,2,2,2,2,2,2,2,2,2,2,2,2,2,2,2,2,2,2,2,2,2,2,2,2,2,
2,2,2,2,2,2,2,2,2,2,2,2,2,2,2,2,2,2,2,2,2,2,2,2,2,2,2,2,2,2,2,2,2,2,2,2,
2,2,2,2,2,2,2,2,2,2,2,2,2,2,2,2,2,2,2,2,2,2,2,2,2,2,2,2,2,2,2,2,2,2,2,2,
2,2,2,2,2,2,2,2,2,2,2,2,2,2,2,2,2,2,2,2,2,2,2,2,2,2,2,2,2,2,2,2,2,2,2,2,
2,2,2,2,2,2,2,2,2,2,2,2,2,2,2,2,2,2,2,2,2,2,2,2,2,2,2,4),(1.00000000230168E-6,
0.00270686683477302,0.00578013839413656,0.0146631673706884,0.0546195079158328,
0.0956849417342354,0.118927518992973,0.128775936846263,0.136252617995142,
0.144478190542676,0.15828221299073,0.235046296377132,0.268196766064285,
0.286394477892574,0.292358443255677,0.296284179023899,0.300167040939504,
0.306427742313422,0.327922114008251,0.382123323164708,0.422311158381288,
0.434910252745757,0.44208371144609,0.448366899237495,0.456249172852546,
0.468792601527292,0.518955441473817,0.565719787146273,0.587278799532253,
0.593306598296846,0.597114659355356,0.600569798001007,0.606200418528769,
0.620832369761187,0.681981858298264,0.727563855778881,0.738978699544188,
0.74623072370966,0.753102243049817,0.762541754626802,0.784632816535728,
0.854402797787406,0.872707911890411,0.884903098454377,0.890096691313338,
0.893939824049587,0.898434112826663,0.906811756910079,0.965737406041129,
1.01356858983867,1.02932012397361,1.03739325442462,1.04339391787124,1.05099379254819,
1.06400661622428,1.14359015573781,1.16749357497808,1.18210231392832,1.18757632047122,
1.19138593847589,1.19556216209836,1.20286773363048,1.2466503732369,1.28143691110029,
1.30769572225958,1.32629495305924,1.3348254503737,1.34143774786581,1.34880564804806,
1.36131579902078,1.43480064613803,1.46340841333038,1.47457962120612,1.48303969140981,
1.4874513914218,1.49119059442889,1.49611282537706,1.50747844961977,1.56433476114742,
1.5999989598884,1.6228690473338,1.63211938844692,1.63888586197319,1.64605080500312,
1.65737090731572,1.69875233824027,1.71627196787867,1.77144690675703,1.78010852447289,
1.78464710306606,1.78836201207362,1.79326289410475,1.80418399198311,1.81992038509624,
1.87477223330872,1.91547880593922,1.92675713612992,1.93390293673173,1.9406553847883,
1.94989187936498,1.97274951265969,2.00840714107598,2.06528199524312,2.07552357683295,
2.08093377673006,2.08473347450726,2.08895721789922,2.09642566664508,2.10589791876019,
2.1277654222735,2.19494631184431,2.21746004485472,2.2268522049097,2.23355637160797,
2.24062130216056,2.25153928621326,2.29086867062449,2.32564080626157,2.36938832195415,
2.37670926188997,2.38090107982992,2.3847139624554,2.3901998970205,2.40492153443202,
2.42913968770142,2.50724404223848,2.52041822514432,2.52803163635923,2.53466351050005,
2.54295266287335,2.55997873443911,2.58312787154005,2.6215354819646,2.66369352930304,
2.67300467983656,2.67760717712282,2.68134300104556,2.68615471963433,2.69659405653731,
2.7113881985145,2.75927686564514,2.80813803034489,2.81967068926964,2.82686675018931,
2.83359174147683,2.84267322490722,2.86449650877761,2.89768572387087,2.94801408370866,
2.9668763350307,2.97304553205218,2.97660063326439,2.98048876321959,2.98638034958086,
3.00438735807661,3.03782125689201,3.10198182120185,3.11542156423178,3.1230894359458,
3.12971193330523,3.13791546624242,3.15449005265703,3.19892062263756,3.25528526333678,
3.26680140627161,3.27145400415412,3.27523692698049,3.2794004830943,3.28657865243074,
3.32452173193262,3.39737921865892),.UNSPECIFIED.);
#423=B_SPLINE_CURVE_WITH_KNOTS('',3,(#38198,#38199,#38200,#38201),
 .UNSPECIFIED.,.F.,.F.,(4,4),(0.5,0.500496609805673),.UNSPECIFIED.);
#424=B_SPLINE_CURVE_WITH_KNOTS('',3,(#38203,#38204,#38205,#38206,#38207,
#38208),.UNSPECIFIED.,.F.,.F.,(4,2,4),(-0.00141044735461021,-0.000756989983528312,
-0.000100211350264882),.UNSPECIFIED.);
#425=B_SPLINE_CURVE_WITH_KNOTS('',3,(#38212,#38213,#38214,#38215,#38216,
#38217,#38218,#38219,#38220,#38221,#38222,#38223,#38224,#38225,#38226,#38227,
#38228,#38229,#38230,#38231,#38232,#38233,#38234,#38235,#38236,#38237,#38238,
#38239,#38240,#38241,#38242,#38243,#38244,#38245,#38246,#38247,#38248,#38249,
#38250,#38251,#38252,#38253,#38254,#38255,#38256,#38257,#38258,#38259,#38260),
 .UNSPECIFIED.,.F.,.F.,(4,3,3,3,3,3,3,3,3,3,3,3,3,3,3,3,4),(0.,0.0927679075208042,
0.125,0.216059062020963,0.25,0.341395816579201,0.375,0.466378627087965,
0.5,0.591378627088015,0.625,0.716395816579185,0.75,0.841059062020798,0.875,
0.967767907520689,1.),.UNSPECIFIED.);
#426=B_SPLINE_CURVE_WITH_KNOTS('',3,(#38262,#38263,#38264,#38265,#38266,
#38267,#38268,#38269,#38270,#38271,#38272,#38273,#38274,#38275,#38276,#38277,
#38278,#38279,#38280,#38281,#38282,#38283,#38284,#38285,#38286,#38287,#38288,
#38289,#38290,#38291,#38292,#38293,#38294,#38295,#38296,#38297,#38298,#38299,
#38300,#38301,#38302,#38303,#38304,#38305,#38306,#38307,#38308,#38309,#38310,
#38311,#38312,#38313,#38314,#38315,#38316,#38317,#38318,#38319,#38320,#38321,
#38322,#38323,#38324,#38325,#38326,#38327,#38328,#38329,#38330,#38331,#38332,
#38333,#38334,#38335,#38336,#38337,#38338,#38339,#38340,#38341,#38342,#38343,
#38344,#38345,#38346,#38347,#38348,#38349,#38350,#38351,#38352,#38353,#38354,
#38355,#38356,#38357,#38358,#38359,#38360,#38361,#38362,#38363,#38364,#38365,
#38366,#38367,#38368,#38369,#38370),.UNSPECIFIED.,.F.,.F.,(4,3,3,3,3,3,
3,3,3,3,3,3,3,3,3,3,3,3,3,3,3,3,3,3,3,3,3,3,3,3,3,3,3,3,3,3,4),(1.46787644835882E-7,
0.0459840424349436,0.0625,0.0640257524258921,0.117713071409535,0.125,0.167674721829891,
0.1875,0.25,0.3125,0.324179685500434,0.375,0.40625,0.4375,0.46875,0.484375,
0.5,0.515625,0.53125,0.5625,0.625,0.634598942174335,0.65625,0.6875,0.71875,
0.734375,0.742632729388345,0.750148009590237,0.757120179138782,0.769674509629174,
0.78125,0.8125,0.84375,0.875,0.926573451013963,0.9375,0.999999590615941),
 .UNSPECIFIED.);
#427=B_SPLINE_CURVE_WITH_KNOTS('',3,(#38372,#38373,#38374,#38375,#38376,
#38377,#38378,#38379,#38380,#38381,#38382,#38383,#38384,#38385,#38386,#38387,
#38388,#38389,#38390,#38391,#38392,#38393,#38394,#38395,#38396,#38397,#38398,
#38399,#38400,#38401,#38402,#38403,#38404,#38405,#38406,#38407,#38408,#38409,
#38410,#38411,#38412,#38413,#38414,#38415,#38416,#38417,#38418,#38419,#38420),
 .UNSPECIFIED.,.F.,.F.,(4,3,3,3,3,3,3,3,3,3,3,3,3,3,3,3,4),(0.,0.0927529117207158,
0.125,0.216043835888795,0.25,0.341380595334184,0.375,0.466363432770545,
0.5,0.591363432771095,0.625,0.716380595334513,0.75,0.841043835888631,0.875,
0.967752911720961,1.),.UNSPECIFIED.);
#428=B_SPLINE_CURVE_WITH_KNOTS('',3,(#38422,#38423,#38424,#38425,#38426,
#38427,#38428,#38429,#38430,#38431,#38432,#38433,#38434,#38435,#38436,#38437,
#38438,#38439,#38440,#38441,#38442,#38443,#38444,#38445,#38446,#38447,#38448,
#38449,#38450,#38451,#38452,#38453,#38454,#38455),.UNSPECIFIED.,.F.,.F.,
(4,2,2,2,2,2,2,2,2,2,2,2,2,2,2,2,4),(0.,0.0927729654601161,0.125,0.216064197637713,
0.25,0.341400950542809,0.375,0.466383751973243,0.5,0.591383751973228,0.625,
0.716400950542821,0.75,0.841064197637697,0.875,0.967772965460199,1.),
 .UNSPECIFIED.);
#429=B_SPLINE_CURVE_WITH_KNOTS('',3,(#38461,#38462,#38463,#38464,#38465,
#38466,#38467,#38468,#38469,#38470,#38471,#38472,#38473,#38474,#38475,#38476,
#38477,#38478,#38479,#38480,#38481,#38482,#38483,#38484,#38485),
 .UNSPECIFIED.,.F.,.F.,(4,3,3,3,3,3,3,3,4),(0.,0.125,0.25,0.375,0.5,0.625,
0.75,0.875,1.),.UNSPECIFIED.);
#430=B_SPLINE_CURVE_WITH_KNOTS('',3,(#38487,#38488,#38489,#38490,#38491,
#38492,#38493,#38494,#38495,#38496,#38497,#38498,#38499,#38500,#38501,#38502,
#38503,#38504,#38505,#38506,#38507,#38508,#38509,#38510,#38511,#38512,#38513,
#38514,#38515,#38516,#38517,#38518,#38519,#38520,#38521,#38522,#38523,#38524,
#38525,#38526,#38527,#38528,#38529,#38530,#38531,#38532,#38533,#38534,#38535),
 .UNSPECIFIED.,.F.,.F.,(4,3,3,3,3,3,3,3,3,3,3,3,3,3,3,3,4),(1.61418366015071E-7,
0.0927499019073366,0.125,0.216040617119944,0.25,0.341377377596209,0.375,
0.466360220727834,0.5,0.591360220727629,0.625,0.716377377596198,0.75,0.841040617119855,
0.875,0.967749741650065,1.),.UNSPECIFIED.);
#431=B_SPLINE_CURVE_WITH_KNOTS('',3,(#38537,#38538,#38539,#38540,#38541,
#38542,#38543,#38544,#38545,#38546,#38547,#38548,#38549,#38550,#38551,#38552,
#38553,#38554,#38555,#38556,#38557,#38558,#38559,#38560,#38561,#38562,#38563,
#38564,#38565,#38566,#38567,#38568,#38569,#38570,#38571,#38572,#38573,#38574,
#38575,#38576,#38577,#38578,#38579,#38580,#38581,#38582,#38583,#38584,#38585),
 .UNSPECIFIED.,.F.,.F.,(4,3,3,3,3,3,3,3,3,3,3,3,3,3,3,3,4),(0.,0.092769801779297,
0.125,0.216060985371345,0.25,0.341397739310444,0.375,0.466380546419268,
0.5,0.591380546419013,0.625,0.716397739310629,0.75,0.841060985371185,0.875,
0.967769801779509,1.),.UNSPECIFIED.);
#432=B_SPLINE_CURVE_WITH_KNOTS('',3,(#38587,#38588,#38589,#38590,#38591,
#38592,#38593,#38594,#38595,#38596,#38597,#38598,#38599,#38600,#38601,#38602,
#38603,#38604,#38605,#38606,#38607,#38608,#38609,#38610,#38611,#38612,#38613,
#38614,#38615,#38616,#38617,#38618,#38619,#38620,#38621,#38622,#38623,#38624,
#38625,#38626,#38627,#38628,#38629,#38630,#38631,#38632,#38633,#38634,#38635),
 .UNSPECIFIED.,.F.,.F.,(4,3,3,3,3,3,3,3,3,3,3,3,3,3,3,3,4),(0.,0.092760818757206,
0.125,0.216051864381934,0.25,0.341388621253046,0.375,0.466371444488478,
0.5,0.59137144448888,0.625,0.716388621253012,0.75,0.841051864382076,0.875,
0.967760818757123,1.),.UNSPECIFIED.);
#433=B_SPLINE_CURVE_WITH_KNOTS('',3,(#38637,#38638,#38639,#38640,#38641,
#38642,#38643,#38644,#38645,#38646,#38647,#38648,#38649,#38650,#38651,#38652,
#38653,#38654,#38655,#38656,#38657,#38658,#38659,#38660,#38661,#38662,#38663,
#38664,#38665,#38666,#38667,#38668,#38669,#38670,#38671,#38672,#38673,#38674,
#38675,#38676,#38677,#38678,#38679,#38680,#38681,#38682,#38683,#38684,#38685),
 .UNSPECIFIED.,.F.,.F.,(4,3,3,3,3,3,3,3,3,3,3,3,3,3,3,3,4),(1.25095121062788E-6,
0.0928811417084261,0.125,0.215904919700791,0.25,0.340703649733594,0.375,
0.472752790800904,0.5,0.58379655566272,0.625,0.717023923539693,0.75,0.841676781252664,
0.875,0.969038482526097,0.999998918721821),.UNSPECIFIED.);
#434=B_SPLINE_CURVE_WITH_KNOTS('',3,(#38687,#38688,#38689,#38690),
 .UNSPECIFIED.,.F.,.F.,(4,4),(0.,0.999999406830264),.UNSPECIFIED.);
#435=B_SPLINE_CURVE_WITH_KNOTS('',3,(#38693,#38694,#38695,#38696,#38697,
#38698,#38699,#38700,#38701,#38702,#38703,#38704,#38705,#38706,#38707,#38708,
#38709,#38710,#38711,#38712,#38713,#38714,#38715,#38716,#38717,#38718,#38719,
#38720,#38721,#38722,#38723,#38724,#38725,#38726,#38727,#38728,#38729,#38730,
#38731,#38732,#38733,#38734,#38735,#38736,#38737,#38738,#38739,#38740,#38741),
 .UNSPECIFIED.,.F.,.F.,(4,3,3,3,3,3,3,3,3,3,3,3,3,3,3,3,4),(5.35569051418317E-13,
0.118460071640814,0.125,0.24207917943708,0.25,0.367390315276668,0.375,0.492346910740242,
0.5,0.617346910740273,0.625,0.742390315276672,0.75,0.867079179437042,0.875,
0.993460071640304,1.),.UNSPECIFIED.);
#436=B_SPLINE_CURVE_WITH_KNOTS('',3,(#38745,#38746,#38747,#38748,#38749,
#38750,#38751,#38752,#38753,#38754,#38755,#38756,#38757,#38758,#38759,#38760,
#38761,#38762,#38763,#38764,#38765,#38766,#38767,#38768,#38769,#38770,#38771,
#38772,#38773,#38774,#38775,#38776,#38777,#38778,#38779,#38780,#38781,#38782,
#38783,#38784,#38785,#38786,#38787,#38788,#38789,#38790,#38791,#38792,#38793),
 .UNSPECIFIED.,.F.,.F.,(4,3,3,3,3,3,3,3,3,3,3,3,3,3,3,3,4),(0.,0.0886362384441663,
0.125,0.212003562124013,0.25,0.337325311248101,0.375,0.462308884423835,
0.5,0.587308884423828,0.625,0.712325311248107,0.75,0.837003562124003,0.875,
0.963636238444181,1.),.UNSPECIFIED.);
#437=B_SPLINE_CURVE_WITH_KNOTS('',3,(#38795,#38796,#38797,#38798,#38799,
#38800,#38801,#38802,#38803,#38804,#38805,#38806,#38807,#38808,#38809,#38810,
#38811,#38812,#38813,#38814,#38815,#38816,#38817,#38818,#38819,#38820,#38821,
#38822,#38823,#38824,#38825,#38826,#38827,#38828,#38829,#38830,#38831,#38832,
#38833,#38834,#38835,#38836,#38837,#38838,#38839,#38840,#38841,#38842,#38843),
 .UNSPECIFIED.,.F.,.F.,(4,3,3,3,3,3,3,3,3,3,3,3,3,3,3,3,4),(0.,0.0886170904948371,
0.125,0.211984120063404,0.25,0.337305875427266,0.375,0.462289482987845,
0.5,0.58728948298785,0.625,0.712305875427259,0.75,0.836984120063407,0.875,
0.963617076466439,0.999999838308052),.UNSPECIFIED.);
#438=B_SPLINE_CURVE_WITH_KNOTS('',3,(#38845,#38846,#38847,#38848,#38849,
#38850,#38851,#38852,#38853,#38854,#38855,#38856,#38857,#38858,#38859,#38860,
#38861,#38862,#38863,#38864,#38865,#38866,#38867,#38868,#38869),
 .UNSPECIFIED.,.F.,.F.,(4,3,3,3,3,3,3,3,4),(0.,0.209718158421766,0.25,0.456937946730344,
0.5,0.70693794673032,0.75,0.959718158421781,1.),.UNSPECIFIED.);
#439=B_SPLINE_CURVE_WITH_KNOTS('',3,(#38873,#38874,#38875,#38876,#38877,
#38878,#38879,#38880,#38881,#38882),.UNSPECIFIED.,.F.,.F.,(4,2,2,2,4),(1.2249654638409E-12,
0.291982900699211,0.5,0.791982900697973,1.),.UNSPECIFIED.);
#440=B_SPLINE_CURVE_WITH_KNOTS('',3,(#38884,#38885,#38886,#38887,#38888,
#38889,#38890,#38891,#38892,#38893,#38894,#38895,#38896,#38897,#38898,#38899,
#38900,#38901,#38902,#38903,#38904,#38905,#38906,#38907,#38908,#38909,#38910,
#38911,#38912,#38913,#38914,#38915,#38916,#38917,#38918,#38919,#38920,#38921,
#38922,#38923,#38924,#38925,#38926,#38927,#38928,#38929,#38930,#38931,#38932),
 .UNSPECIFIED.,.F.,.F.,(4,3,3,3,3,3,3,3,3,3,3,3,3,3,3,3,4),(0.,0.0886392611603209,
0.125,0.212006631260798,0.25,0.337328379396744,0.375,0.462311947147395,
0.5,0.587311947147404,0.625,0.712328379396739,0.75,0.837006631260799,0.875,
0.963639261160282,1.),.UNSPECIFIED.);
#441=B_SPLINE_CURVE_WITH_KNOTS('',3,(#38934,#38935,#38936,#38937,#38938,
#38939,#38940,#38941,#38942,#38943,#38944,#38945,#38946,#38947,#38948,#38949,
#38950,#38951,#38952,#38953,#38954,#38955,#38956,#38957,#38958,#38959,#38960,
#38961,#38962,#38963,#38964,#38965,#38966,#38967,#38968,#38969,#38970,#38971,
#38972,#38973,#38974,#38975,#38976,#38977,#38978,#38979,#38980,#38981,#38982),
 .UNSPECIFIED.,.F.,.F.,(4,3,3,3,3,3,3,3,3,3,3,3,3,3,3,3,4),(0.,0.0886201162472742,
0.125,0.211987192297148,0.25,0.337308946677277,0.375,0.462292548802212,
0.5,0.587292548802218,0.625,0.712308946677277,0.75,0.836987192297145,0.875,
0.963620116247306,1.),.UNSPECIFIED.);
#442=B_SPLINE_CURVE_WITH_KNOTS('',3,(#38984,#38985,#38986,#38987,#38988,
#38989,#38990,#38991,#38992,#38993,#38994,#38995,#38996,#38997,#38998,#38999,
#39000,#39001,#39002,#39003,#39004,#39005,#39006,#39007,#39008,#39009,#39010,
#39011,#39012,#39013,#39014,#39015,#39016,#39017,#39018,#39019,#39020,#39021,
#39022,#39023,#39024,#39025,#39026,#39027,#39028,#39029,#39030,#39031,#39032),
 .UNSPECIFIED.,.F.,.F.,(4,3,3,3,3,3,3,3,3,3,3,3,3,3,3,3,4),(5.05515188767001E-7,
0.0886110104715978,0.125,0.211979068662331,0.25,0.337305561024299,0.375,
0.462245638602086,0.5,0.587333292602463,0.625,0.712306032467428,0.75,0.836989026938191,
0.875,0.963623466963222,0.99999974561912),.UNSPECIFIED.);
#443=B_SPLINE_CURVE_WITH_KNOTS('',3,(#39034,#39035,#39036,#39037,#39038,
#39039,#39040,#39041,#39042,#39043,#39044,#39045,#39046,#39047,#39048,#39049,
#39050,#39051,#39052,#39053,#39054,#39055,#39056,#39057,#39058,#39059,#39060,
#39061,#39062,#39063,#39064,#39065,#39066,#39067,#39068,#39069,#39070,#39071,
#39072,#39073,#39074,#39075,#39076,#39077,#39078,#39079,#39080,#39081,#39082),
 .UNSPECIFIED.,.F.,.F.,(4,3,3,3,3,3,3,3,3,3,3,3,3,3,3,3,4),(0.,0.0886344285884905,
0.125,0.212001724472824,0.25,0.337323474188171,0.375,0.462307050612556,
0.5,0.587307050612541,0.625,0.712323474188171,0.75,0.837001724472838,0.875,
0.963634428588436,1.),.UNSPECIFIED.);
#444=B_SPLINE_CURVE_WITH_KNOTS('',3,(#39084,#39085,#39086,#39087,#39088,
#39089,#39090,#39091,#39092,#39093,#39094,#39095,#39096,#39097,#39098,#39099,
#39100,#39101,#39102,#39103,#39104,#39105,#39106,#39107,#39108),
 .UNSPECIFIED.,.F.,.F.,(4,3,3,3,3,3,3,3,4),(0.,0.177329485747707,0.25,0.424060419200447,
0.5,0.674060419200489,0.75,0.927329485747577,1.),.UNSPECIFIED.);
#445=B_SPLINE_CURVE_WITH_KNOTS('',3,(#39112,#39113,#39114,#39115,#39116,
#39117,#39118),.UNSPECIFIED.,.F.,.F.,(4,1,1,1,4),(0.,0.25,0.5,0.75,1.),
 .UNSPECIFIED.);
#446=B_SPLINE_CURVE_WITH_KNOTS('',3,(#39120,#39121,#39122,#39123,#39124,
#39125,#39126,#39127,#39128,#39129,#39130,#39131,#39132,#39133,#39134,#39135,
#39136,#39137,#39138,#39139,#39140,#39141,#39142,#39143,#39144,#39145,#39146,
#39147,#39148,#39149,#39150,#39151,#39152,#39153,#39154,#39155,#39156,#39157,
#39158,#39159,#39160,#39161,#39162,#39163,#39164,#39165,#39166,#39167,#39168,
#39169,#39170,#39171,#39172,#39173,#39174,#39175,#39176,#39177,#39178,#39179,
#39180,#39181,#39182,#39183,#39184,#39185,#39186),.UNSPECIFIED.,.F.,.F.,
(4,3,3,3,3,3,3,3,3,3,3,3,3,3,3,3,3,3,3,3,3,3,4),(1.06075131901111E-6,0.0884946396841923,
0.102026634743488,0.125,0.212110420183879,0.25,0.261096997261559,0.337989428361259,
0.375,0.420019583798184,0.457713536375547,0.5,0.580296494461757,0.599118987891557,
0.625,0.711607136294009,0.740646741453979,0.75,0.836347955298163,0.875,
0.898862893862905,0.962328567718677,0.999998772366922),.UNSPECIFIED.);
#447=B_SPLINE_CURVE_WITH_KNOTS('',3,(#39187,#39188,#39189,#39190,#39191,
#39192,#39193,#39194,#39195,#39196,#39197,#39198,#39199,#39200,#39201,#39202,
#39203,#39204,#39205,#39206,#39207,#39208,#39209,#39210,#39211,#39212,#39213,
#39214,#39215,#39216,#39217,#39218,#39219,#39220,#39221,#39222,#39223,#39224,
#39225,#39226,#39227,#39228,#39229,#39230,#39231,#39232,#39233,#39234,#39235),
 .UNSPECIFIED.,.F.,.F.,(4,3,3,3,3,3,3,3,3,3,3,3,3,3,3,3,4),(0.,0.0886276628941314,
0.125,0.211994854865046,0.25,0.337316606787889,0.375,0.462300195359125,
0.5,0.587300195359111,0.625,0.712316606787894,0.75,0.836994854865049,0.875,
0.963627662894127,1.),.UNSPECIFIED.);
#448=B_SPLINE_CURVE_WITH_KNOTS('',3,(#39276,#39277,#39278,#39279,#39280,
#39281,#39282,#39283,#39284,#39285,#39286,#39287,#39288,#39289,#39290,#39291,
#39292,#39293,#39294,#39295,#39296,#39297,#39298,#39299,#39300,#39301,#39302,
#39303,#39304,#39305,#39306,#39307,#39308,#39309,#39310,#39311,#39312,#39313,
#39314,#39315),.UNSPECIFIED.,.F.,.F.,(4,3,3,3,3,3,3,3,3,3,3,3,3,4),(-0.499777858153212,
-0.47181324986483,-0.404411035114472,-0.399568579211665,-0.370348404118398,
-0.312287096243119,-0.306423970531928,-0.263103928856152,-0.205372645614112,
-0.199340068239674,-0.11676936673232,-0.101385295104661,-0.096217945588105,
0.),.UNSPECIFIED.);
#449=B_SPLINE_CURVE_WITH_KNOTS('',3,(#39316,#39317,#39318,#39319,#39320,
#39321,#39322,#39323,#39324,#39325,#39326,#39327,#39328,#39329,#39330,#39331,
#39332,#39333,#39334,#39335,#39336,#39337,#39338,#39339,#39340,#39341,#39342,
#39343,#39344,#39345,#39346,#39347,#39348,#39349,#39350,#39351,#39352,#39353,
#39354,#39355,#39356,#39357,#39358),.UNSPECIFIED.,.F.,.F.,(4,3,3,3,3,3,
3,3,3,3,3,3,3,3,4),(-0.503648702838967,-0.430770877953045,-0.423912464156221,
-0.414886975050139,-0.331929750071717,-0.32764763640537,-0.286137866472306,
-0.230749364089863,-0.225605706863336,-0.22120879272055,-0.117677069982424,
-0.111686767538004,-0.0817616813229237,-0.0223522743546254,0.),
 .UNSPECIFIED.);
#450=B_SPLINE_CURVE_WITH_KNOTS('',3,(#39628,#39629,#39630,#39631,#39632,
#39633),.UNSPECIFIED.,.F.,.F.,(4,2,4),(7.69181997283135E-5,0.00104275533486278,
0.00201241795641651),.UNSPECIFIED.);
#451=B_SPLINE_CURVE_WITH_KNOTS('',3,(#39634,#39635,#39636,#39637,#39638,
#39639,#39640,#39641,#39642,#39643,#39644,#39645,#39646,#39647,#39648,#39649,
#39650,#39651,#39652,#39653,#39654,#39655,#39656,#39657,#39658,#39659,#39660,
#39661,#39662,#39663,#39664,#39665,#39666,#39667,#39668,#39669,#39670,#39671,
#39672,#39673),.UNSPECIFIED.,.F.,.F.,(4,3,3,3,3,3,3,3,3,3,3,3,3,4),(0.,
0.0959833697741033,0.101972206699614,0.195587298215562,0.206341771970019,
0.216827129531729,0.271561541990413,0.3003318498953,0.306853038549853,0.312555564896745,
0.399722509461884,0.404649475313381,0.493811083623272,0.501724005229504),
 .UNSPECIFIED.);
#452=B_SPLINE_CURVE_WITH_KNOTS('',3,(#39942,#39943,#39944,#39945,#39946,
#39947,#39948,#39949,#39950,#39951,#39952,#39953,#39954,#39955,#39956,#39957,
#39958,#39959,#39960,#39961,#39962,#39963,#39964,#39965,#39966,#39967,#39968,
#39969,#39970,#39971,#39972,#39973,#39974,#39975,#39976,#39977,#39978,#39979,
#39980,#39981,#39982,#39983,#39984,#39985,#39986,#39987,#39988,#39989,#39990,
#39991,#39992,#39993,#39994,#39995,#39996,#39997,#39998,#39999),
 .UNSPECIFIED.,.F.,.F.,(4,3,3,3,3,3,3,3,3,3,3,3,3,3,3,3,3,3,3,4),(0.000189315453215585,
0.0299594922632419,0.108460134023621,0.114084312282721,0.118341445248336,
0.223026221099152,0.228346490943163,0.239675938105935,0.322886901748949,
0.329558994731095,0.33493041280197,0.389982815414618,0.404828322990172,
0.413165778692639,0.418170476314411,0.422544813989412,0.449072712381233,
0.476360707610091,0.50168871402095,0.503648702838949),.UNSPECIFIED.);
#453=B_SPLINE_CURVE_WITH_KNOTS('',3,(#40145,#40146,#40147,#40148,#40149,
#40150,#40151,#40152,#40153,#40154,#40155,#40156,#40157,#40158,#40159,#40160,
#40161,#40162,#40163,#40164,#40165,#40166,#40167,#40168,#40169,#40170,#40171,
#40172,#40173,#40174,#40175,#40176,#40177,#40178,#40179,#40180,#40181,#40182,
#40183,#40184,#40185,#40186,#40187,#40188,#40189,#40190),.UNSPECIFIED.,
 .F.,.F.,(4,3,3,3,3,3,3,3,3,3,3,3,3,3,3,4),(9.88255891804216E-5,0.0299029135328962,
0.117771907894534,0.147638843125062,0.220655384964364,0.224985986036839,
0.229406390499783,0.237239648816644,0.328742913474894,0.334897242635998,
0.404790741220614,0.413084719440826,0.418385494722407,0.42240987867637,
0.501611305817306,0.503648702838969),.UNSPECIFIED.);
#454=B_SPLINE_CURVE_WITH_KNOTS('',3,(#40191,#40192,#40193,#40194,#40195,
#40196,#40197,#40198,#40199,#40200,#40201,#40202,#40203,#40204,#40205,#40206,
#40207,#40208,#40209,#40210,#40211,#40212,#40213,#40214,#40215,#40216,#40217,
#40218,#40219,#40220,#40221,#40222,#40223,#40224,#40225,#40226,#40227,#40228,
#40229,#40230,#40231,#40232,#40233),.UNSPECIFIED.,.F.,.F.,(4,3,3,3,3,3,
3,3,3,3,3,3,3,3,4),(-0.503648702838958,-0.429930161153392,-0.422397062002223,
-0.416091587548294,-0.333112845076983,-0.328793934021496,-0.300414695296256,
-0.288538996878268,-0.233218025246608,-0.227649042762086,-0.222314267218344,
-0.11882824439468,-0.11430518334793,-0.0249444678531058,0.),
 .UNSPECIFIED.);
#455=B_SPLINE_CURVE_WITH_KNOTS('',3,(#40237,#40238,#40239,#40240,#40241,
#40242,#40243,#40244,#40245,#40246,#40247,#40248,#40249,#40250,#40251,#40252,
#40253,#40254,#40255,#40256,#40257,#40258,#40259,#40260,#40261,#40262,#40263,
#40264,#40265,#40266,#40267,#40268,#40269,#40270,#40271,#40272,#40273,#40274,
#40275,#40276,#40277,#40278,#40279,#40280,#40281,#40282),.UNSPECIFIED.,
 .F.,.F.,(4,3,3,3,3,3,3,3,3,3,3,3,3,3,3,4),(-0.500212455550078,-0.471794247742062,
-0.409627241063031,-0.404584739756394,-0.39961108596175,-0.322820829274765,
-0.311856171421863,-0.26553693014911,-0.207517702253279,-0.202680435589951,
-0.198239983473561,-0.107350009536642,-0.100409420181077,-0.0696937723003933,
-0.0181002222704456,0.),.UNSPECIFIED.);
#456=B_SPLINE_CURVE_WITH_KNOTS('',3,(#40424,#40425,#40426,#40427,#40428,
#40429,#40430,#40431,#40432,#40433,#40434,#40435,#40436,#40437,#40438,#40439,
#40440,#40441,#40442,#40443,#40444,#40445,#40446,#40447,#40448,#40449,#40450,
#40451,#40452,#40453,#40454,#40455,#40456,#40457,#40458,#40459,#40460,#40461,
#40462,#40463),.UNSPECIFIED.,.F.,.F.,(4,3,3,3,3,3,3,3,3,3,3,3,3,4),(0.,
0.0979252393519714,0.101981016086327,0.186131114719788,0.194303776652966,
0.201330780004315,0.205068643612296,0.214441627415338,0.396886032890214,
0.402513654010981,0.407314608904017,0.437254927315218,0.49643612517153,
0.501724005229503),.UNSPECIFIED.);
#457=B_SPLINE_CURVE_WITH_KNOTS('',3,(#40497,#40498,#40499,#40500,#40501,
#40502,#40503,#40504,#40505,#40506,#40507,#40508,#40509,#40510,#40511,#40512,
#40513,#40514,#40515,#40516,#40517,#40518,#40519,#40520,#40521,#40522,#40523,
#40524,#40525,#40526,#40527,#40528,#40529,#40530,#40531,#40532,#40533,#40534,
#40535,#40536,#40537,#40538,#40539,#40540,#40541,#40542,#40543,#40544,#40545,
#40546),.UNSPECIFIED.,.F.,.F.,(4,2,2,2,2,2,2,2,2,2,2,2,2,2,2,2,2,2,2,2,
2,2,2,2,4),(0.000209493712794322,0.0422872913938982,0.0542226665498989,
0.0656299001912059,0.0761984914852202,0.0887188350368748,0.144055532882821,
0.166979316880622,0.181775163552867,0.188803136528792,0.194952964302586,
0.204776397594916,0.236321457818492,0.28877412063129,0.301515346905665,
0.312233055563606,0.323797735338658,0.344187219178032,0.372232761612485,
0.42043174817154,0.429529383616972,0.435416861196921,0.440637222272047,
0.447327481728966,0.472483010091814),.UNSPECIFIED.);
#458=B_SPLINE_CURVE_WITH_KNOTS('',3,(#40549,#40550,#40551,#40552,#40553,
#40554,#40555,#40556,#40557,#40558,#40559,#40560,#40561,#40562,#40563,#40564,
#40565,#40566,#40567,#40568,#40569,#40570,#40571,#40572,#40573,#40574,#40575,
#40576,#40577,#40578),.UNSPECIFIED.,.F.,.F.,(4,2,2,2,2,2,2,2,2,2,2,2,2,
2,4),(9.99999999571378E-7,0.00565775487530941,0.0129173728394934,0.0519474282669346,
0.0924692038786361,0.106536967386471,0.118140574424233,0.132780272231367,
0.172415521622109,0.222944405297024,0.236545301367104,0.243410862645757,
0.249272230574711,0.258478354896224,0.275556593261106),.UNSPECIFIED.);
#459=B_SPLINE_CURVE_WITH_KNOTS('',3,(#40584,#40585,#40586,#40587,#40588,
#40589,#40590,#40591,#40592,#40593,#40594,#40595,#40596,#40597,#40598,#40599,
#40600,#40601,#40602,#40603,#40604,#40605,#40606,#40607,#40608,#40609,#40610,
#40611,#40612,#40613,#40614,#40615,#40616,#40617,#40618,#40619,#40620,#40621,
#40622,#40623,#40624,#40625,#40626,#40627,#40628,#40629,#40630,#40631,#40632,
#40633,#40634,#40635,#40636,#40637,#40638,#40639,#40640,#40641,#40642,#40643,
#40644,#40645,#40646,#40647,#40648,#40649,#40650,#40651,#40652,#40653,#40654,
#40655,#40656,#40657,#40658,#40659,#40660,#40661,#40662,#40663,#40664,#40665,
#40666,#40667,#40668,#40669,#40670,#40671,#40672,#40673,#40674,#40675,#40676,
#40677,#40678,#40679,#40680,#40681,#40682,#40683,#40684,#40685,#40686,#40687,
#40688,#40689,#40690,#40691,#40692,#40693,#40694,#40695,#40696,#40697,#40698,
#40699,#40700,#40701,#40702,#40703,#40704,#40705,#40706,#40707,#40708,#40709,
#40710,#40711,#40712,#40713,#40714,#40715,#40716,#40717,#40718,#40719,#40720,
#40721,#40722,#40723,#40724,#40725,#40726,#40727,#40728,#40729,#40730,#40731,
#40732,#40733,#40734,#40735,#40736,#40737,#40738,#40739,#40740,#40741),
 .UNSPECIFIED.,.F.,.F.,(4,2,2,2,2,2,2,2,2,2,2,2,2,2,2,2,2,2,2,2,2,2,2,2,
2,2,2,2,2,2,2,2,2,2,2,2,2,2,2,2,2,2,2,2,2,2,2,2,2,2,2,2,2,2,2,2,2,2,2,2,
2,2,2,2,2,2,2,2,2,2,2,2,2,2,2,2,2,2,4),(6.30435270860889,6.33486878320123,
6.34366974614675,6.34966324284323,6.35703713755435,6.37420620250057,6.40375264025194,
6.4470390695231,6.46203191150256,6.47264308026978,6.48406809681009,6.50407751685343,
6.53144912706435,6.58091498964814,6.58971900104101,6.59571521178631,6.60309649351356,
6.62029862705322,6.64995101906424,6.693024043224,6.708012300807,6.71862649719076,
6.73006138331729,6.75011057786636,6.7775645954391,6.82685633546438,6.83568099086117,
6.84167591283988,6.8490295334854,6.8660798204813,6.89526589896446,6.93907381839847,
6.9540616271593,6.96466389709236,6.97607323881813,6.99603127669263,7.02329568207772,
7.07302291161279,7.08179288524694,7.087779399277,7.09516137744094,7.11239908891738,
7.14215363461921,7.18521725183071,7.20021562855414,7.21082892841909,7.22225457039669,
7.24226256268532,7.26963720002217,7.31902650273789,7.3278387071296,7.3338469765065,
7.34126629547086,7.35864634523377,7.3888709987462,7.43087825960643,7.44583940029455,
7.45646854729715,7.46795493496144,7.48821541141176,7.51611323660128,7.56446287865684,
7.57339841015601,7.57939406940583,7.586623356302,7.60299394716167,7.63017917440611,
7.67742899532298,7.69229453732945,7.70282865451226,7.71416963637204,7.73398882738903,
7.76099878006726,7.81118536759106,7.81992573892269,7.82589410585711,7.83325762804537,
7.84165606901659,7.87995889022397),.UNSPECIFIED.);
#460=B_SPLINE_CURVE_WITH_KNOTS('',3,(#40742,#40743,#40744,#40745),
 .UNSPECIFIED.,.F.,.F.,(4,4),(1.01357413598985E-6,0.000209493712794322),
 .UNSPECIFIED.);
#461=B_SPLINE_CURVE_WITH_KNOTS('',3,(#40746,#40747,#40748,#40749,#40750,
#40751,#40752,#40753,#40754,#40755,#40756,#40757,#40758,#40759,#40760,#40761,
#40762,#40763,#40764,#40765,#40766,#40767,#40768,#40769,#40770,#40771,#40772,
#40773,#40774,#40775,#40776,#40777,#40778,#40779,#40780,#40781,#40782,#40783,
#40784,#40785,#40786,#40787,#40788,#40789,#40790,#40791,#40792,#40793,#40794,
#40795,#40796,#40797,#40798,#40799,#40800,#40801,#40802,#40803,#40804,#40805,
#40806,#40807,#40808,#40809,#40810,#40811,#40812,#40813,#40814,#40815,#40816,
#40817,#40818,#40819,#40820,#40821,#40822,#40823,#40824,#40825,#40826,#40827,
#40828,#40829,#40830,#40831,#40832,#40833,#40834,#40835,#40836,#40837,#40838,
#40839,#40840,#40841,#40842,#40843,#40844,#40845,#40846,#40847,#40848,#40849,
#40850,#40851,#40852,#40853,#40854,#40855,#40856,#40857,#40858,#40859,#40860,
#40861,#40862,#40863,#40864,#40865,#40866,#40867,#40868,#40869,#40870,#40871,
#40872,#40873,#40874,#40875,#40876,#40877,#40878,#40879,#40880,#40881,#40882,
#40883,#40884,#40885,#40886,#40887,#40888,#40889,#40890,#40891,#40892,#40893,
#40894,#40895,#40896,#40897,#40898,#40899,#40900,#40901),.UNSPECIFIED.,
 .F.,.F.,(4,2,2,2,2,2,2,2,2,2,2,2,2,2,2,2,2,2,2,2,2,2,2,2,2,2,2,2,2,2,2,
2,2,2,2,2,2,2,2,2,2,2,2,2,2,2,2,2,2,2,2,2,2,2,2,2,2,2,2,2,2,2,2,2,2,2,2,
2,2,2,2,2,2,2,2,2,2,4),(0.275556593261106,0.302257716093375,0.332145449002062,
0.353019638320446,0.364182811346166,0.374094054396295,0.387016365935024,
0.424468399690209,0.474784838723073,0.486382245753939,0.49262015904604,
0.498086515168979,0.507668815230086,0.549849706736197,0.580898810950735,
0.602581422114444,0.614391844510637,0.625103828088379,0.639873751023731,
0.68612813271093,0.712253967143993,0.728243775062982,0.73554602991629,0.741707481959803,
0.751244469819963,0.794030213469046,0.824223859030593,0.845430043251126,
0.857061734857099,0.867632782348189,0.882182911159433,0.941047537998989,
0.96150213928913,0.97527996369794,0.982123309918813,0.98815353536044,0.997879223181914,
1.04633441080135,1.07317249406427,1.09290377583721,1.10421640948278,1.11473376705714,
1.12958982902173,1.17659174660286,1.20386064199112,1.22025213524982,1.22747630986562,
1.23345821413433,1.24235725539788,1.29095061193003,1.3187384153877,1.33893993740818,
1.35040225813014,1.36101160205548,1.37594642745454,1.41769551255673,1.4480412350592,
1.46544943938522,1.47286386661574,1.47885850768789,1.4876337927126,1.5372593554286,
1.56452795041183,1.58447799162328,1.59587951676874,1.60647281319572,1.62144445402929,
1.66411223318268,1.69407854731155,1.7113737724098,1.7187549102345,1.72472703980151,
1.73345363173632,1.78346592748571,1.81060244195952,1.83049217765482,1.84187542645257,
1.85022063120531),.UNSPECIFIED.);
#462=B_SPLINE_CURVE_WITH_KNOTS('',3,(#40906,#40907,#40908,#40909,#40910,
#40911,#40912,#40913,#40914,#40915,#40916,#40917,#40918,#40919,#40920,#40921,
#40922,#40923,#40924,#40925,#40926,#40927,#40928,#40929,#40930,#40931,#40932,
#40933,#40934,#40935,#40936,#40937,#40938,#40939,#40940,#40941,#40942,#40943,
#40944,#40945,#40946,#40947,#40948,#40949,#40950,#40951,#40952,#40953,#40954,
#40955,#40956,#40957,#40958,#40959,#40960,#40961,#40962,#40963,#40964,#40965,
#40966,#40967,#40968,#40969,#40970,#40971,#40972,#40973,#40974,#40975,#40976,
#40977,#40978,#40979,#40980,#40981,#40982,#40983,#40984,#40985,#40986,#40987,
#40988,#40989,#40990,#40991,#40992,#40993,#40994,#40995,#40996,#40997,#40998,
#40999,#41000,#41001,#41002,#41003,#41004,#41005,#41006,#41007,#41008,#41009,
#41010,#41011,#41012,#41013,#41014,#41015,#41016,#41017,#41018,#41019,#41020,
#41021,#41022,#41023,#41024,#41025,#41026,#41027,#41028,#41029,#41030,#41031,
#41032,#41033,#41034,#41035,#41036,#41037,#41038,#41039,#41040,#41041,#41042,
#41043,#41044,#41045,#41046,#41047,#41048,#41049,#41050,#41051,#41052,#41053,
#41054,#41055,#41056,#41057,#41058,#41059,#41060,#41061,#41062,#41063),
 .UNSPECIFIED.,.F.,.F.,(4,2,2,2,2,2,2,2,2,2,2,2,2,2,2,2,2,2,2,2,2,2,2,2,
2,2,2,2,2,2,2,2,2,2,2,2,2,2,2,2,2,2,2,2,2,2,2,2,2,2,2,2,2,2,2,2,2,2,2,2,
2,2,2,2,2,2,2,2,2,2,2,2,2,2,2,2,2,2,4),(4.72819048267577,4.73950795185586,
4.75012210979889,4.76155086895958,4.78156836809081,4.80895190741352,4.85843117911358,
4.86723766046422,4.87323362414742,4.88060942980026,4.89778064245953,4.92732947790588,
4.97061576111725,4.98561061430102,4.99622420623809,5.00765283970181,5.02767158171161,
5.05505859474814,5.10452501033381,5.11333238041157,5.119328288513,5.12670325752487,
5.14386935222794,5.17340318557322,5.21670622262401,5.23170062699955,5.24231393095466,
5.25374230849599,5.27376083811829,5.30114790257251,5.35061005460223,5.35941738370218,
5.3654130554825,5.37278737207586,5.38995088389089,5.41947774454824,5.46278794072297,
5.47778169663862,5.4883943710803,5.49982188080286,5.51983816805462,5.54722109224304,
5.59668877283127,5.6054948237148,5.61149004333747,5.61886426512492,5.63602890233187,
5.6655599240848,5.70886382307828,5.72385725358769,5.73446957571265,5.74589658496825,
5.76591167794044,5.79329281107251,5.84275834566241,5.85156409224043,5.85755945109383,
5.86493479128113,5.88210548756745,5.91165646761162,5.95492013716683,5.9699124918867,
5.98052501497582,5.99195326255171,6.0119740552566,6.03936750252539,6.08880259339068,
6.09761148824992,6.10360662335611,6.11097785502081,6.1281262103999,6.15760933171281,
6.20097342104773,6.21596522841018,6.22657577246508,6.23800016613919,6.25800788400909,
6.28537444195454,6.30435270860889),.UNSPECIFIED.);
#463=B_SPLINE_CURVE_WITH_KNOTS('',3,(#41064,#41065,#41066,#41067,#41068,
#41069,#41070,#41071,#41072,#41073,#41074,#41075,#41076,#41077,#41078,#41079,
#41080,#41081,#41082,#41083,#41084,#41085,#41086,#41087,#41088,#41089,#41090,
#41091,#41092,#41093,#41094,#41095,#41096,#41097,#41098,#41099,#41100,#41101,
#41102,#41103,#41104,#41105,#41106,#41107,#41108,#41109,#41110,#41111,#41112,
#41113,#41114,#41115,#41116,#41117,#41118,#41119,#41120,#41121,#41122,#41123,
#41124,#41125,#41126,#41127,#41128,#41129,#41130,#41131,#41132,#41133,#41134,
#41135,#41136,#41137,#41138,#41139,#41140,#41141,#41142,#41143,#41144,#41145,
#41146,#41147,#41148,#41149,#41150,#41151,#41152,#41153,#41154,#41155,#41156,
#41157,#41158,#41159,#41160,#41161,#41162,#41163,#41164,#41165,#41166,#41167,
#41168,#41169,#41170,#41171,#41172,#41173,#41174,#41175,#41176,#41177,#41178,
#41179,#41180,#41181,#41182,#41183,#41184,#41185,#41186,#41187,#41188,#41189,
#41190,#41191,#41192,#41193,#41194,#41195,#41196,#41197,#41198,#41199,#41200,
#41201,#41202,#41203,#41204,#41205,#41206,#41207,#41208,#41209,#41210,#41211,
#41212,#41213,#41214,#41215,#41216,#41217,#41218,#41219),.UNSPECIFIED.,
 .F.,.F.,(4,2,2,2,2,2,2,2,2,2,2,2,2,2,2,2,2,2,2,2,2,2,2,2,2,2,2,2,2,2,2,
2,2,2,2,2,2,2,2,2,2,2,2,2,2,2,2,2,2,2,2,2,2,2,2,2,2,2,2,2,2,2,2,2,2,2,2,
2,2,2,2,2,2,2,2,2,2,4),(1.85022063120531,1.85245803545648,1.86742343567781,
1.91092677999263,1.94025068089833,1.95733584714856,1.9646854274236,1.97066601700574,
1.97945105943726,2.02899469267185,2.05633207510499,2.07631803047564,2.08772733025059,
2.09832096608194,2.11328308319158,2.15603372225511,2.18584052738125,2.20308163037672,
2.21045914351855,2.21644079802621,2.22520415870899,2.27492501537538,2.30217744978419,
2.32212212808228,2.33352104296743,2.34411139064825,2.35907813354066,2.40202494263366,
2.43173414326021,2.448944807865,2.45631516411609,2.46229382809607,2.47105314309451,
2.5208064963315,2.54805044763132,2.56799158078089,2.57938927809238,2.58997869927616,
2.60494442056477,2.64798095380983,2.67761542931793,2.69480159722625,2.70216859579123,
2.7081487224768,2.71691624692997,2.76660392905713,2.79387563535955,2.81382999658193,
2.82523127782325,2.83582222281463,2.85078748140468,2.89371885123636,2.92342331327636,
2.94063208540719,2.94800303400513,2.95398316784399,2.96274709136088,3.0124644483609,
3.03972253770116,3.05967032655013,3.07106994252096,3.08166033426212,3.09662625340397,
3.13959336916278,3.1692785866773,3.18648130065975,3.19385096254273,3.19983073143358,
3.20859451245861,3.2583134518259,3.28557185055764,3.3055198931902,3.31691956705066,
3.32750995083086,3.34247577477007,3.38545424338359,3.41512952594777,3.42490669701472),
 .UNSPECIFIED.);
#464=B_SPLINE_CURVE_WITH_KNOTS('',3,(#41224,#41225,#41226,#41227,#41228,
#41229,#41230,#41231,#41232,#41233,#41234,#41235,#41236,#41237,#41238,#41239,
#41240,#41241,#41242,#41243,#41244,#41245,#41246,#41247,#41248,#41249,#41250,
#41251,#41252,#41253,#41254,#41255,#41256,#41257,#41258,#41259,#41260,#41261,
#41262,#41263,#41264,#41265,#41266,#41267,#41268,#41269,#41270,#41271,#41272,
#41273,#41274,#41275,#41276,#41277,#41278,#41279,#41280,#41281,#41282,#41283,
#41284,#41285,#41286,#41287,#41288,#41289,#41290,#41291,#41292,#41293,#41294,
#41295,#41296,#41297,#41298,#41299,#41300,#41301,#41302,#41303,#41304,#41305,
#41306,#41307,#41308,#41309,#41310,#41311,#41312,#41313,#41314,#41315,#41316,
#41317,#41318,#41319,#41320,#41321,#41322,#41323,#41324,#41325,#41326,#41327,
#41328,#41329,#41330,#41331,#41332,#41333,#41334,#41335,#41336,#41337,#41338,
#41339,#41340,#41341,#41342,#41343,#41344,#41345,#41346,#41347,#41348,#41349,
#41350,#41351,#41352,#41353,#41354,#41355,#41356,#41357,#41358,#41359,#41360,
#41361,#41362,#41363,#41364,#41365,#41366,#41367,#41368,#41369,#41370,#41371,
#41372,#41373,#41374,#41375,#41376,#41377,#41378,#41379),.UNSPECIFIED.,
 .F.,.F.,(4,2,2,2,2,2,2,2,2,2,2,2,2,2,2,2,2,2,2,2,2,2,2,2,2,2,2,2,2,2,2,
2,2,2,2,2,2,2,2,2,2,2,2,2,2,2,2,2,2,2,2,2,2,2,2,2,2,2,2,2,2,2,2,2,2,2,2,
2,2,2,2,2,2,2,2,2,2,4),(3.15163477931716,3.15298897800685,3.16238915291939,
3.20652316777823,3.23631453510694,3.25737596078581,3.26897275867627,3.27952566483782,
3.29407041532064,3.35235036865309,3.3728309815977,3.3866151299212,3.39346659347139,
3.39954852935888,3.40941344026376,3.44468995601634,3.47940486850441,3.5023744208504,
3.51426586598204,3.52474840048023,3.53842769924747,3.59544554110014,3.61777418371048,
3.6323332685606,3.63931464019944,3.64534505137541,3.65487513183864,3.69766251601296,
3.72811334463534,3.74944920047817,3.76109086059298,3.77163275342468,3.78607775600029,
3.8449932390036,3.86524842884655,3.87893564142306,3.88577126146191,3.8918620139421,
3.90177670873891,3.93886568365411,3.98643481968158,4.00130483072224,4.01190269193801,
4.02337820046101,4.04367536038818,4.07168373699399,4.11973819691762,4.12870546523491,
4.13471998074014,4.14200401683087,4.15852421519058,4.18610554687911,4.23240953690924,
4.24734931712728,4.25795632477907,4.26940615582526,4.28954829302094,4.31720844817241,
4.3660547580922,4.37493356713054,4.3809377544045,4.38827163283667,4.4051410940172,
4.43376174987304,4.47841465989933,4.49340541599483,4.50401914264897,4.5154505679836,
4.53548223967792,4.56289658186719,4.61230833309369,4.62112304563995,4.6271200943582,
4.6344914860604,4.65162945556555,4.68107395400867,4.7245115038362,4.72819048267577),
 .UNSPECIFIED.);
#465=B_SPLINE_CURVE_WITH_KNOTS('',3,(#41380,#41381,#41382,#41383,#41384,
#41385,#41386,#41387,#41388,#41389,#41390,#41391,#41392,#41393,#41394,#41395,
#41396,#41397,#41398,#41399,#41400,#41401,#41402,#41403,#41404,#41405,#41406,
#41407,#41408,#41409,#41410,#41411,#41412,#41413,#41414,#41415,#41416,#41417,
#41418,#41419,#41420,#41421,#41422,#41423,#41424,#41425,#41426,#41427,#41428,
#41429,#41430,#41431,#41432,#41433,#41434,#41435,#41436,#41437,#41438,#41439,
#41440,#41441,#41442,#41443,#41444,#41445,#41446,#41447,#41448,#41449,#41450,
#41451,#41452,#41453,#41454,#41455,#41456,#41457,#41458,#41459,#41460,#41461,
#41462,#41463,#41464,#41465,#41466,#41467,#41468,#41469,#41470,#41471,#41472,
#41473,#41474,#41475,#41476,#41477,#41478,#41479,#41480,#41481,#41482,#41483,
#41484,#41485,#41486,#41487,#41488,#41489,#41490,#41491,#41492,#41493,#41494,
#41495,#41496,#41497,#41498,#41499,#41500,#41501,#41502,#41503,#41504,#41505,
#41506,#41507,#41508,#41509,#41510,#41511,#41512,#41513,#41514,#41515,#41516,
#41517,#41518,#41519,#41520,#41521,#41522,#41523,#41524,#41525,#41526,#41527,
#41528,#41529,#41530,#41531,#41532,#41533,#41534,#41535,#41536,#41537,#41538,
#41539),.UNSPECIFIED.,.F.,.F.,(4,2,2,2,2,2,2,2,2,2,2,2,2,2,2,2,2,2,2,2,
2,2,2,2,2,2,2,2,2,2,2,2,2,2,2,2,2,2,2,2,2,2,2,2,2,2,2,2,2,2,2,2,2,2,2,2,
2,2,2,2,2,2,2,2,2,2,2,2,2,2,2,2,2,2,2,2,2,2,2,4),(3.42490669701472,3.43232900937426,
3.43969829801849,3.44567833743907,3.45444340772131,3.50415231677713,3.53141504241583,
3.55136514504334,3.56276536765941,3.5733559672353,3.58832164819124,3.63127353358472,
3.66096759078479,3.6781731340077,3.68554337761954,3.69152334799716,3.70028723094562,
3.75000664143778,3.77726495614238,3.79721303103668,3.80861285460821,3.81920347093602,
3.83416980904366,3.87717038552534,3.90683077511809,3.92402561123087,3.9313943222146,
3.9373744942306,3.94614063170833,3.9958408787074,4.02310765778037,4.04305960357326,
4.05446010444556,4.06505052396108,4.08001514446103,4.1228808607337,4.15263751223124,
4.16986304230536,4.17723603423089,4.18321554998337,4.19197490861075,4.24173491283261,
4.26897644454247,4.28891702452145,4.30031571146024,4.31090697332087,4.32587722245906,
4.36937895902415,4.39868650088571,4.41576813047898,4.4231211723634,4.42910412598506,
4.43646726570338,4.45971562472414,4.50520763102599,4.53139557445127,4.54371433568145,
4.5541180054599,4.56730274768906,4.60218149192356,4.65148806356465,4.66391775308509,
4.67052045405102,4.67679960714132,4.68750057680989,4.7015915514247,4.74262703357355,
4.77468881107418,4.78787526656112,4.79827946517432,4.81059788314442,4.83678448185971,
4.88228453828832,4.90548434936197,4.91284436066545,4.91882714926359,4.92618309784467,
4.94328338218393,4.97264560048608,4.99969446742076),.UNSPECIFIED.);
#466=B_SPLINE_CURVE_WITH_KNOTS('',3,(#41544,#41545,#41546,#41547,#41548,
#41549,#41550,#41551,#41552,#41553,#41554,#41555,#41556,#41557,#41558,#41559,
#41560,#41561,#41562,#41563,#41564,#41565,#41566,#41567,#41568,#41569,#41570,
#41571,#41572,#41573,#41574,#41575,#41576,#41577,#41578,#41579,#41580,#41581,
#41582,#41583,#41584,#41585,#41586,#41587,#41588,#41589,#41590,#41591,#41592,
#41593,#41594,#41595,#41596,#41597,#41598,#41599,#41600,#41601,#41602,#41603,
#41604,#41605,#41606,#41607,#41608,#41609,#41610,#41611,#41612,#41613,#41614,
#41615,#41616,#41617,#41618,#41619,#41620,#41621,#41622,#41623,#41624,#41625,
#41626,#41627,#41628,#41629,#41630,#41631,#41632,#41633,#41634,#41635,#41636,
#41637,#41638,#41639,#41640,#41641,#41642,#41643,#41644,#41645,#41646,#41647,
#41648,#41649,#41650,#41651,#41652,#41653,#41654,#41655,#41656,#41657,#41658,
#41659,#41660,#41661,#41662,#41663,#41664,#41665,#41666,#41667,#41668,#41669,
#41670,#41671,#41672,#41673,#41674,#41675,#41676,#41677,#41678,#41679,#41680,
#41681,#41682,#41683,#41684,#41685,#41686,#41687,#41688,#41689,#41690,#41691,
#41692,#41693,#41694,#41695,#41696,#41697,#41698,#41699),.UNSPECIFIED.,
 .F.,.F.,(4,2,2,2,2,2,2,2,2,2,2,2,2,2,2,2,2,2,2,2,2,2,2,2,2,2,2,2,2,2,2,
2,2,2,2,2,2,2,2,2,2,2,2,2,2,2,2,2,2,2,2,2,2,2,2,2,2,2,2,2,2,2,2,2,2,2,2,
2,2,2,2,2,2,2,2,2,2,4),(1.57573377077494,1.62765792826645,1.64959536187562,
1.66399107840287,1.67094216055766,1.67697668986032,1.68655851418989,1.72842730949596,
1.75932678332557,1.78083900036542,1.79250216644476,1.80302743167571,1.81739114789624,
1.87670562810885,1.89678969429371,1.91039884999513,1.91721772124075,1.92331003450725,
1.93325191685743,1.97089147230866,2.00397410831103,2.0263397248044,2.03813683621378,
2.04863311602486,2.06272342571438,2.1176522354464,2.14083124951818,2.15572836792034,
2.16276251929583,2.16877142344457,2.17816783765395,2.22229373429271,2.25207163880422,
2.27312448195018,2.28471713128469,2.29526654080658,2.30980688182928,2.36806871883366,
2.38854354444909,2.40232357767318,2.4091727629334,2.41525246645886,2.42511327097463,
2.4584377159878,2.49440636690439,2.5178117205551,2.52976442851919,2.54023191880453,
2.55379343767083,2.6116463098907,2.63362193023033,2.6480349291388,2.65499078921074,
2.66102769979372,2.67061121068673,2.7125346838191,2.74342068747608,2.76493078745306,
2.77659726502315,2.78712790206586,2.80150309322966,2.86079835467284,2.88090211573173,
2.89452170521694,2.90134430867959,2.90743827759055,2.91738134281159,2.95499587952527,
2.98811449016284,3.01049649694549,3.02229829801593,3.03279684452293,3.04688704308136,
3.10187416891229,3.12504668052472,3.13994304117261,3.14697820988748,3.15163477931716),
 .UNSPECIFIED.);
#467=B_SPLINE_CURVE_WITH_KNOTS('',3,(#41700,#41701,#41702,#41703,#41704,
#41705,#41706,#41707,#41708,#41709,#41710,#41711,#41712,#41713,#41714,#41715,
#41716,#41717,#41718,#41719,#41720,#41721,#41722,#41723,#41724,#41725,#41726,
#41727,#41728,#41729,#41730,#41731,#41732,#41733,#41734,#41735,#41736,#41737,
#41738,#41739,#41740,#41741,#41742,#41743,#41744,#41745,#41746,#41747,#41748,
#41749,#41750,#41751,#41752,#41753,#41754,#41755,#41756,#41757,#41758,#41759,
#41760,#41761,#41762,#41763,#41764,#41765,#41766,#41767,#41768,#41769,#41770,
#41771,#41772,#41773,#41774,#41775,#41776,#41777,#41778,#41779,#41780,#41781,
#41782,#41783,#41784,#41785,#41786,#41787,#41788,#41789,#41790,#41791,#41792,
#41793,#41794,#41795,#41796,#41797,#41798,#41799,#41800,#41801,#41802,#41803,
#41804,#41805,#41806,#41807,#41808,#41809,#41810,#41811,#41812,#41813,#41814,
#41815,#41816,#41817,#41818,#41819,#41820,#41821,#41822,#41823,#41824,#41825,
#41826,#41827,#41828,#41829,#41830,#41831,#41832,#41833,#41834,#41835,#41836,
#41837,#41838,#41839,#41840,#41841,#41842,#41843,#41844,#41845,#41846,#41847,
#41848,#41849,#41850,#41851,#41852,#41853,#41854,#41855,#41856,#41857),
 .UNSPECIFIED.,.F.,.F.,(4,2,2,2,2,2,2,2,2,2,2,2,2,2,2,2,2,2,2,2,2,2,2,2,
2,2,2,2,2,2,2,2,2,2,2,2,2,2,2,2,2,2,2,2,2,2,2,2,2,2,2,2,2,2,2,2,2,2,2,2,
2,2,2,2,2,2,2,2,2,2,2,2,2,2,2,2,2,2,4),(4.99969446742076,5.01612222627699,
5.03109516348412,5.04168706966171,5.05308518898519,5.07302229762032,5.1002546627482,
5.14997692512985,5.15873609088758,5.1647157027327,5.17208878556789,5.1893137796041,
5.2190661229799,5.26198773137693,5.27695508294564,5.28754590343637,5.29894534460231,
5.31889228788194,5.34614704355636,5.3958124203372,5.40457756099,5.41055759285015,
5.41792650755612,5.43512281958154,5.46478613974075,5.50782924203427,5.52279756377833,
5.53338817485161,5.5447866086011,5.56472941162079,5.59197565421998,5.64165680760733,
5.65041958749698,5.65639916459359,5.66376897940814,5.68097325410772,5.71066239908315,
5.75366657805781,5.76863392821428,5.77922407496883,5.79062219761345,5.81056502390953,
5.83781199515832,5.88748687860816,5.89624982930673,5.90222928343406,5.90959871406835,
5.92680106382864,5.95648509297602,5.99949210260467,6.01445893700445,6.02504880009767,
6.03644671594783,6.05638954826976,6.08363702364114,6.13330675622669,6.14206979428491,
6.14804903332223,6.1554177543789,6.17261703184667,6.20229247583851,6.24530894913595,
6.26027522555275,6.27086448881313,6.28226153981436,6.30220205280319,6.32944519668532,
6.37912113982749,6.38788283983767,6.39386163221232,6.40123032730111,6.41843116490278,
6.44811212107449,6.49112058930372,6.50608651709517,6.51667543994895,6.52807202836461,
6.54801148982236,6.57429106571742),.UNSPECIFIED.);
#468=B_SPLINE_CURVE_WITH_KNOTS('',3,(#41860,#41861,#41862,#41863,#41864,
#41865,#41866,#41867,#41868,#41869,#41870,#41871,#41872,#41873,#41874,#41875,
#41876,#41877,#41878,#41879,#41880,#41881,#41882,#41883,#41884,#41885,#41886,
#41887,#41888,#41889),.UNSPECIFIED.,.T.,.F.,(4,2,2,2,2,2,2,2,2,2,2,2,2,
2,4),(0.,0.125,0.14292295086177,0.25,0.285800104977707,0.375,0.42861930011293,
0.5,0.571377117830905,0.625,0.714197774307772,0.75,0.857087735980742,0.875,
1.),.UNSPECIFIED.);
#469=B_SPLINE_CURVE_WITH_KNOTS('',3,(#41895,#41896,#41897,#41898,#41899,
#41900,#41901,#41902,#41903,#41904,#41905,#41906,#41907,#41908,#41909,#41910,
#41911,#41912,#41913,#41914,#41915,#41916,#41917,#41918,#41919),
 .UNSPECIFIED.,.F.,.F.,(4,3,3,3,3,3,3,3,4),(8.08098624460284E-14,0.185589856128629,
0.25,0.432168172320759,0.5,0.682168172320751,0.75,0.935589856128578,1.),
 .UNSPECIFIED.);
#470=B_SPLINE_CURVE_WITH_KNOTS('',3,(#41923,#41924,#41925,#41926,#41927,
#41928,#41929,#41930,#41931,#41932,#41933,#41934,#41935,#41936,#41937,#41938,
#41939,#41940,#41941,#41942,#41943,#41944,#41945,#41946,#41947,#41948,#41949,
#41950,#41951,#41952,#41953,#41954,#41955,#41956,#41957,#41958,#41959,#41960,
#41961,#41962,#41963,#41964,#41965,#41966,#41967,#41968,#41969,#41970,#41971,
#41972,#41973,#41974,#41975,#41976,#41977,#41978,#41979,#41980,#41981,#41982,
#41983,#41984,#41985,#41986,#41987,#41988,#41989,#41990,#41991,#41992,#41993,
#41994,#41995,#41996,#41997,#41998,#41999,#42000,#42001,#42002,#42003,#42004,
#42005,#42006,#42007,#42008,#42009,#42010,#42011,#42012,#42013,#42014,#42015,
#42016,#42017,#42018,#42019,#42020,#42021,#42022),.UNSPECIFIED.,.F.,.F.,
(4,2,2,2,2,2,2,2,2,2,2,2,2,2,2,2,2,2,2,2,2,2,2,2,2,2,2,2,2,2,2,2,2,2,2,
2,2,2,2,2,2,2,2,2,2,2,2,2,2,4),(8.14853860778369,8.16952826439388,8.21130376441472,
8.22623517802908,8.2368405400259,8.2482970281195,8.26848496361379,8.29624866877044,
8.34478884818763,8.35368295116283,8.35966224525979,8.36688375521984,8.38327081527719,
8.41053459302116,8.45755714724689,8.47240884484075,8.48292186841738,8.49422859899152,
8.51394716165414,8.54076356003648,8.58918975381341,8.59889384251938,8.60491862652603,
8.61176490778234,8.62557233139796,8.64610175919149,8.70476844526811,8.71934725585207,
8.72991779791933,8.74152915216654,8.76263341682554,8.79259020149926,8.83575324613513,
8.84524474377202,8.85139811770872,8.85871560890523,8.87482363784368,8.90129418975491,
8.94695055904045,8.96175119473661,8.97246257761506,8.98425125307571,9.00582359482735,
9.03661281625652,9.079277716991,9.08877611000028,9.09422577303682,9.10048321199873,
9.10729564609716,9.13371097451824),.UNSPECIFIED.);
#471=B_SPLINE_CURVE_WITH_KNOTS('',3,(#42096,#42097,#42098,#42099,#42100,
#42101,#42102),.UNSPECIFIED.,.F.,.F.,(4,1,1,1,4),(-1.00000000003634,-0.785714285714286,
-0.5,-0.285714285714286,0.),.UNSPECIFIED.);
#472=B_SPLINE_CURVE_WITH_KNOTS('',3,(#42106,#42107,#42108,#42109,#42110,
#42111,#42112,#42113,#42114,#42115,#42116,#42117,#42118),.UNSPECIFIED.,
 .F.,.F.,(4,3,3,3,4),(-1.00728892207246,-0.785714285714271,-0.499999999999975,
-0.285714285714254,-0.00388490843767506),.UNSPECIFIED.);
#473=B_SPLINE_CURVE_WITH_KNOTS('',3,(#42119,#42120,#42121,#42122,#42123,
#42124,#42125,#42126,#42127,#42128,#42129,#42130,#42131,#42132,#42133,#42134),
 .UNSPECIFIED.,.F.,.F.,(4,2,2,2,2,2,2,4),(0.,0.125,0.142930238992666,0.25,
0.285797996648243,0.375,0.428625070295843,0.5),.UNSPECIFIED.);
#474=B_SPLINE_CURVE_WITH_KNOTS('',3,(#42136,#42137,#42138,#42139,#42140,
#42141,#42142,#42143,#42144,#42145,#42146,#42147,#42148,#42149,#42150,#42151,
#42152,#42153,#42154,#42155,#42156,#42157,#42158,#42159,#42160,#42161,#42162,
#42163,#42164,#42165,#42166,#42167,#42168,#42169,#42170,#42171,#42172,#42173,
#42174,#42175,#42176,#42177,#42178,#42179,#42180,#42181,#42182,#42183,#42184,
#42185,#42186,#42187,#42188,#42189,#42190,#42191,#42192,#42193,#42194,#42195,
#42196,#42197,#42198,#42199,#42200,#42201,#42202,#42203,#42204,#42205,#42206,
#42207,#42208,#42209,#42210,#42211,#42212,#42213,#42214,#42215,#42216,#42217,
#42218,#42219,#42220,#42221,#42222,#42223,#42224,#42225,#42226,#42227,#42228,
#42229,#42230,#42231,#42232,#42233,#42234,#42235,#42236,#42237,#42238,#42239,
#42240,#42241,#42242,#42243,#42244,#42245,#42246,#42247,#42248,#42249,#42250,
#42251,#42252,#42253,#42254,#42255,#42256,#42257,#42258,#42259,#42260,#42261,
#42262,#42263,#42264,#42265,#42266,#42267,#42268,#42269,#42270,#42271,#42272,
#42273,#42274,#42275,#42276,#42277,#42278,#42279,#42280,#42281,#42282,#42283,
#42284,#42285,#42286,#42287,#42288,#42289,#42290,#42291,#42292,#42293),
 .UNSPECIFIED.,.F.,.F.,(4,2,2,2,2,2,2,2,2,2,2,2,2,2,2,2,2,2,2,2,2,2,2,2,
2,2,2,2,2,2,2,2,2,2,2,2,2,2,2,2,2,2,2,2,2,2,2,2,2,2,2,2,2,2,2,2,2,2,2,2,
2,2,2,2,2,2,2,2,2,2,2,2,2,2,2,2,2,2,4),(0.000492563516689082,0.0341773825702078,
0.0575679327368054,0.0695405979140284,0.080049251897907,0.0937029164043512,
0.151407163606198,0.173705220541313,0.188260994861637,0.195239466532897,
0.201229835610513,0.210651604612185,0.254192847398101,0.284228886612211,
0.305357526206893,0.316905967924253,0.327360354313765,0.341661949166553,
0.401357262672953,0.421409295931973,0.434990789447019,0.441773538848331,
0.447845020942935,0.457705587063812,0.491936437561936,0.527323937432171,
0.550541172588345,0.562482488398015,0.572980379233105,0.586646844990631,
0.643384374021231,0.665625338642604,0.680145545196282,0.687132637128509,
0.693179422881149,0.702781210952997,0.744025731518034,0.77522830088162,
0.796856261903557,0.808537183417919,0.819058257864295,0.833383886246761,
0.893022300843321,0.913019973709865,0.92659117754553,0.933400964082066,
0.939487126547021,0.949422006253815,0.9876332057857,1.02034457517022,1.0425628713401,
1.05432752661319,1.06481341692,1.0789159362931,1.13367863289971,1.15693108349076,
1.17185362339831,1.17888626616877,1.1848894220167,1.19426317033574,1.23857413766376,
1.26825527692179,1.28926748143279,1.30085452805911,1.31140795327241,1.32597043241504,
1.3840113167314,1.40453338966003,1.4183327500512,1.42518637685489,1.43126538812174,
1.4411230076461,1.47423916106134,1.51032084223349,1.53376037562423,1.54571514203592,
1.55617812384814,1.56972476147254,1.57573377077494),.UNSPECIFIED.);
#475=B_SPLINE_CURVE_WITH_KNOTS('',3,(#42294,#42295,#42296,#42297,#42298,
#42299,#42300,#42301,#42302,#42303,#42304,#42305,#42306,#42307,#42308,#42309,
#42310,#42311,#42312,#42313,#42314,#42315,#42316,#42317,#42318,#42319,#42320,
#42321,#42322,#42323,#42324,#42325,#42326,#42327,#42328,#42329,#42330,#42331,
#42332,#42333,#42334,#42335,#42336,#42337,#42338,#42339,#42340,#42341,#42342,
#42343,#42344,#42345,#42346,#42347,#42348,#42349,#42350,#42351,#42352,#42353,
#42354,#42355,#42356,#42357,#42358,#42359,#42360,#42361,#42362,#42363,#42364,
#42365,#42366,#42367,#42368,#42369,#42370,#42371,#42372,#42373,#42374,#42375,
#42376,#42377,#42378,#42379,#42380,#42381,#42382,#42383,#42384,#42385,#42386,
#42387,#42388,#42389,#42390,#42391,#42392,#42393,#42394,#42395,#42396,#42397,
#42398,#42399,#42400,#42401,#42402,#42403,#42404,#42405,#42406,#42407,#42408,
#42409,#42410,#42411,#42412,#42413,#42414,#42415,#42416,#42417,#42418,#42419,
#42420,#42421,#42422,#42423,#42424,#42425,#42426,#42427,#42428,#42429,#42430,
#42431,#42432,#42433,#42434,#42435,#42436,#42437,#42438,#42439,#42440,#42441,
#42442,#42443,#42444,#42445,#42446,#42447,#42448,#42449,#42450,#42451,#42452,
#42453),.UNSPECIFIED.,.F.,.F.,(4,2,2,2,2,2,2,2,2,2,2,2,2,2,2,2,2,2,2,2,
2,2,2,2,2,2,2,2,2,2,2,2,2,2,2,2,2,2,2,2,2,2,2,2,2,2,2,2,2,2,2,2,2,2,2,2,
2,2,2,2,2,2,2,2,2,2,2,2,2,2,2,2,2,2,2,2,2,2,2,4),(6.57429106571742,6.57525312780825,
6.62492647305338,6.63368794510889,6.63966689284873,6.64703667225612,6.664243319311,
6.69394354699268,6.73691334989607,6.75187810133236,6.76246721858811,6.7738650909055,
6.79381047113821,6.82106484856978,6.8707067458127,6.87947153249801,6.88545027371608,
6.89281584938557,6.90999927630054,6.93962843610894,6.98270214150769,6.99766683268721,
7.00825406798716,7.01964798195614,7.03957951401267,7.0668053321817,7.11651096144781,
7.12526727912624,7.13124435902373,7.13861302368273,7.15582021492245,7.18552258815762,
7.2285057924792,7.24347103047062,7.25405883896717,7.26545357522281,7.2853879155563,
7.31262115632881,7.36229296993982,7.37105299601105,7.37703285822145,7.38440845393583,
7.40164566696,7.43144510282038,7.47422987238597,7.48919000344632,7.49978074330808,
7.51118546323947,7.53116031983854,7.55847739348733,7.60797073119219,7.61675207961588,
7.62273067714667,7.63007813321545,7.64715914178237,7.67647586609909,7.72001071707904,
7.73497347848119,7.74555282386888,7.7569311847097,7.77680955932541,7.80392574551293,
7.85388397829139,7.86260685946152,7.86857681560139,7.87595541755871,7.89324468633585,
7.92319870849767,7.96590180693535,7.98087055981519,7.99146026296552,8.00285641024184,
8.02279382133068,8.05003986018625,8.09961288982266,8.10838377760247,8.1143759906819,
8.12178784521217,8.13919108703434,8.14853860778369),.UNSPECIFIED.);
#476=B_SPLINE_CURVE_WITH_KNOTS('',3,(#42457,#42458,#42459,#42460,#42461,
#42462,#42463,#42464,#42465,#42466,#42467,#42468,#42469,#42470,#42471,#42472,
#42473,#42474,#42475,#42476,#42477,#42478,#42479,#42480,#42481,#42482,#42483,
#42484,#42485,#42486,#42487,#42488,#42489,#42490,#42491,#42492,#42493,#42494,
#42495,#42496,#42497,#42498,#42499,#42500,#42501,#42502,#42503,#42504,#42505,
#42506,#42507,#42508,#42509,#42510,#42511,#42512,#42513,#42514,#42515,#42516,
#42517,#42518,#42519,#42520,#42521,#42522,#42523,#42524,#42525,#42526,#42527,
#42528,#42529,#42530,#42531,#42532,#42533,#42534,#42535,#42536,#42537,#42538,
#42539,#42540,#42541,#42542,#42543,#42544,#42545,#42546,#42547,#42548,#42549,
#42550,#42551,#42552,#42553,#42554,#42555,#42556,#42557,#42558,#42559,#42560,
#42561,#42562,#42563,#42564,#42565,#42566,#42567,#42568,#42569,#42570,#42571,
#42572,#42573,#42574,#42575,#42576,#42577,#42578,#42579,#42580,#42581,#42582,
#42583,#42584,#42585,#42586,#42587,#42588,#42589,#42590,#42591,#42592,#42593,
#42594,#42595,#42596,#42597,#42598,#42599,#42600,#42601,#42602,#42603,#42604,
#42605,#42606,#42607,#42608,#42609,#42610,#42611,#42612,#42613,#42614,#42615,
#42616,#42617,#42618,#42619,#42620,#42621,#42622,#42623,#42624,#42625,#42626,
#42627,#42628,#42629,#42630,#42631,#42632,#42633,#42634,#42635,#42636,#42637,
#42638,#42639,#42640,#42641,#42642,#42643,#42644,#42645,#42646,#42647,#42648,
#42649,#42650,#42651,#42652,#42653,#42654,#42655,#42656,#42657,#42658,#42659,
#42660,#42661,#42662,#42663,#42664,#42665,#42666,#42667,#42668,#42669,#42670,
#42671,#42672,#42673,#42674,#42675,#42676,#42677,#42678,#42679,#42680,#42681,
#42682,#42683,#42684,#42685,#42686,#42687,#42688,#42689,#42690,#42691,#42692,
#42693,#42694,#42695,#42696,#42697,#42698,#42699,#42700,#42701,#42702,#42703,
#42704,#42705,#42706,#42707,#42708,#42709,#42710,#42711,#42712,#42713,#42714,
#42715,#42716,#42717,#42718,#42719,#42720,#42721,#42722,#42723,#42724,#42725,
#42726,#42727,#42728,#42729,#42730,#42731,#42732,#42733,#42734,#42735,#42736,
#42737,#42738,#42739,#42740,#42741,#42742,#42743,#42744,#42745,#42746,#42747,
#42748,#42749,#42750,#42751,#42752,#42753,#42754,#42755,#42756,#42757,#42758,
#42759,#42760,#42761,#42762,#42763,#42764,#42765,#42766,#42767,#42768,#42769,
#42770,#42771,#42772,#42773,#42774,#42775,#42776,#42777,#42778,#42779,#42780,
#42781,#42782,#42783,#42784,#42785,#42786,#42787,#42788,#42789,#42790,#42791,
#42792,#42793,#42794,#42795,#42796,#42797,#42798,#42799,#42800,#42801,#42802,
#42803,#42804,#42805,#42806,#42807,#42808,#42809,#42810,#42811,#42812,#42813,
#42814,#42815,#42816,#42817,#42818,#42819,#42820,#42821,#42822,#42823,#42824,
#42825,#42826,#42827,#42828,#42829,#42830,#42831,#42832,#42833,#42834,#42835,
#42836,#42837,#42838,#42839,#42840,#42841,#42842,#42843,#42844,#42845,#42846,
#42847,#42848,#42849,#42850,#42851,#42852,#42853,#42854,#42855,#42856,#42857,
#42858,#42859,#42860,#42861,#42862,#42863,#42864,#42865,#42866,#42867,#42868,
#42869,#42870,#42871,#42872,#42873,#42874,#42875,#42876,#42877,#42878,#42879,
#42880,#42881,#42882,#42883,#42884,#42885,#42886,#42887,#42888,#42889,#42890,
#42891,#42892,#42893,#42894,#42895,#42896,#42897,#42898,#42899,#42900,#42901,
#42902,#42903,#42904,#42905,#42906,#42907,#42908,#42909,#42910,#42911,#42912,
#42913,#42914,#42915,#42916,#42917,#42918,#42919,#42920,#42921,#42922,#42923,
#42924,#42925,#42926,#42927,#42928,#42929,#42930,#42931,#42932,#42933,#42934,
#42935,#42936,#42937,#42938,#42939,#42940,#42941,#42942,#42943,#42944,#42945,
#42946,#42947,#42948,#42949,#42950,#42951,#42952,#42953,#42954,#42955,#42956,
#42957,#42958,#42959,#42960,#42961,#42962,#42963,#42964,#42965,#42966,#42967,
#42968,#42969,#42970,#42971,#42972,#42973,#42974,#42975,#42976,#42977,#42978,
#42979,#42980,#42981,#42982,#42983,#42984,#42985,#42986,#42987,#42988,#42989,
#42990,#42991,#42992,#42993,#42994,#42995,#42996,#42997,#42998,#42999,#43000,
#43001,#43002,#43003,#43004,#43005,#43006,#43007,#43008,#43009,#43010,#43011,
#43012),.UNSPECIFIED.,.F.,.F.,(4,2,2,2,2,2,2,2,2,2,2,2,2,2,2,2,2,2,2,2,
2,2,2,2,2,2,2,2,2,2,2,2,2,2,2,2,2,2,2,2,2,2,2,2,2,2,2,2,2,2,2,2,2,2,2,2,
2,2,2,2,2,2,2,2,2,2,2,2,2,2,2,2,2,2,2,2,2,2,2,2,2,2,2,2,2,2,2,2,2,2,2,2,
2,2,2,2,2,2,2,2,2,2,2,2,2,2,2,2,2,2,2,2,2,2,2,2,2,2,2,2,2,2,2,2,2,2,2,2,
2,2,2,2,2,2,2,2,2,2,2,2,2,2,2,2,2,2,2,2,2,2,2,2,2,2,2,2,2,2,2,2,2,2,2,2,
2,2,2,2,2,2,2,2,2,2,2,2,2,2,2,2,2,2,2,2,2,2,2,2,2,2,2,2,2,2,2,2,2,2,2,2,
2,2,2,2,2,2,2,2,2,2,2,2,2,2,2,2,2,2,2,2,2,2,2,2,2,2,2,2,2,2,2,2,2,2,2,2,
2,2,2,2,2,2,2,2,2,2,2,2,2,2,2,2,2,2,2,2,2,2,2,2,2,2,2,2,2,2,2,2,2,2,2,2,
2,2,2,2,2,4),(-5.04396562385481,-4.9980997399527,-4.98517304167195,-4.97475139559582,
-4.96166371518258,-4.921775707794,-4.89290076511485,-4.88456488860594,-4.8785680730564,
-4.87008445784522,-4.83672939119426,-4.80028885219112,-4.78769996080878,
-4.77726507703883,-4.76400838452873,-4.73054630709276,-4.70650394910092,
-4.69619601034013,-4.68780851051061,-4.68181156156318,-4.67337915758532,
-4.63945495070001,-4.60358755870111,-4.59096148088791,-4.58052971024975,
-4.56732186964725,-4.53109971760608,-4.50881566590829,-4.49888645340053,
-4.49071720534244,-4.48471608964361,-4.47604780804978,-4.449005747584,-4.42070634761022,
-4.40666120058398,-4.39407596545333,-4.38364158980256,-4.37038253566392,
-4.33664883357748,-4.31279127262899,-4.30252191157765,-4.29415656481433,
-4.28815973320411,-4.27970570955559,-4.24601432125875,-4.20997688873402,
-4.19734388266647,-4.18691194094929,-4.17371104356827,-4.1373312314936,
-4.11513893028465,-4.10523004910812,-4.09707249032982,-4.09107049916221,
-4.08238714555653,-4.05800788480088,-4.02801990766354,-4.01362476225451,
-4.00083425924956,-3.99040814439592,-3.97716614184849,-3.93912396593494,
-3.90886908488587,-3.90050508873323,-3.89450792470256,-3.88605161859358,
-3.85237892225237,-3.8161886131112,-3.80360056947496,-3.79316571460693,
-3.77990845723896,-3.74538679304435,-3.7220542950279,-3.71189576584705,
-3.70359387915126,-3.69759597423091,-3.6890744283436,-3.6561820560895,-3.62025958972076,
-3.60735638871829,-3.59693228420076,-3.58381383094242,-3.54424147308057,
-3.51462519149695,-3.5065095921122,-3.5005051263756,-3.49177010707168,-3.45349842000022,
-3.42710425054575,-3.41273120962491,-3.40223261938362,-3.39019823640823,
-3.36569740343653,-3.36147034427012,-3.3312092116069,-3.31975449511956,
-3.3107256902233,-3.3047578718194,-3.29704216671289,-3.27225427536476,-3.24121717728329,
-3.22661595293402,-3.21370516322041,-3.20328097974073,-3.19017015830589,
-3.15050920248891,-3.12150449765795,-3.11314613088155,-3.10714867910601,
-3.09868585411656,-3.06508118920166,-3.02882775500764,-3.01624126270455,
-3.00580589278111,-2.99254559742156,-2.95879977160056,-2.93494661651809,
-2.9246777145481,-2.91631240787225,-2.91031506206288,-2.90185953622638,
-2.86817471840147,-2.8319924711787,-2.81940412294166,-2.80896896003358,
-2.79571122867243,-2.76225320730671,-2.73820079857532,-2.72789038512483,
-2.71950135489018,-2.71350420950499,-2.70507313391826,-2.67112288763767,
-2.63526778873467,-2.62264100548169,-2.61220811636895,-2.59899810347981,
-2.56279740603495,-2.54049800602625,-2.53056489713006,-2.5223931372204,
-2.51639138478821,-2.50772378236512,-2.48256899715478,-2.43843788980511,
-2.42580407415773,-2.41547151391196,-2.40210417538893,-2.37329609545325,
-2.33491239210544,-2.32618692988061,-2.32018294755467,-2.31205947587147,
-2.28219692540875,-2.24302609734378,-2.22987849102719,-2.21945384116751,
-2.20657735072229,-2.17223538648604,-2.13721553536805,-2.12888216918187,
-2.12288452532769,-2.11439581859475,-2.10391216418375,-2.07900238538826,
-2.0467674883918,-2.03354220280478,-2.0231084357258,-2.01049363347507,-1.97501370751928,
-1.94048055212601,-1.93209907102176,-1.92610170015708,-1.91766255644763,
-1.88821372113992,-1.84940963752081,-1.83623016330586,-1.82580453163593,
-1.81295620316917,-1.77753687330015,-1.74377447611805,-1.7353200520767,
-1.72932199350505,-1.72095323761138,-1.71068045451249,-1.68680241944228,
-1.6531429601866,-1.63988492492727,-1.62944829646414,-1.61685643626237,
-1.58091333839126,-1.54687011339687,-1.53844096501795,-1.53244338339867,
-1.52405137812602,-1.51373760576268,-1.4896619176958,-1.45627914048263,
-1.44302413175325,-1.432589131087,-1.41999897114718,-1.40594419482603,-1.3776177180808,
-1.35055266625314,-1.34188042274638,-1.33587876477466,-1.32771234378527,
-1.31779034355513,-1.29553657129119,-1.25928909807849,-1.24608278548942,
-1.23564916667892,-1.22301736637024,-1.18711148810971,-1.15317872555741,
-1.14473908814109,-1.13873846837883,-1.13034569787102,-1.10070203595733,
-1.0620413769319,-1.04885022177276,-1.03841875808444,-1.02556551691472,
-0.988322305896801,-0.956665726743883,-0.948072596609712,-0.942074562471509,
-0.933844274676115,-0.904768749791148,-0.864856542057289,-0.851776633085321,
-0.841361068612671,-0.828444460549937,-0.813826751526624,-0.782708281311359,
-0.757983219586049,-0.750266579081623,-0.744303167463873,-0.735295079569443,
-0.723880916128707,-0.693868839046441,-0.665207196242956,-0.653033399552585,
-0.642552720577251,-0.62842387841274,-0.611669104989387,-0.565617573062991,
-0.55561770717174,-0.549543765701532,-0.542170263894716,-0.522951951329844,
-0.476594372838271,-0.461268813403962,-0.450642607100512,-0.438951849204563,
-0.415321945435501,-0.370261879634943,-0.359532031488147,-0.353921591201462,
-0.347213117971576,-0.333193810459605,-0.3102448063465,-0.274955635025903,
-0.261740926979313,-0.251374343263263,-0.238931025985625,-0.202432263450545,
-0.168717182801042,-0.160282113829637,-0.154303257202801,-0.1459900731177,
-0.135821813315604,-0.112500651658126,-0.077610350198274,-0.0642890983207978,
-0.053806453088995,-0.0411553443408391,-0.000209718449385024),
 .UNSPECIFIED.);
#477=B_SPLINE_CURVE_WITH_KNOTS('',3,(#43014,#43015,#43016,#43017,#43018,
#43019,#43020,#43021,#43022,#43023,#43024,#43025,#43026),.UNSPECIFIED.,
 .F.,.F.,(4,3,3,3,4),(0.,0.465944417146252,0.5,0.965944417145535,0.99999951939385),
 .UNSPECIFIED.);
#478=B_SPLINE_CURVE_WITH_KNOTS('',3,(#43030,#43031,#43032,#43033,#43034,
#43035,#43036,#43037,#43038,#43039,#43040,#43041,#43042,#43043,#43044,#43045,
#43046,#43047,#43048,#43049,#43050,#43051,#43052,#43053,#43054,#43055,#43056,
#43057,#43058,#43059,#43060,#43061,#43062,#43063,#43064,#43065,#43066,#43067,
#43068,#43069,#43070,#43071,#43072,#43073,#43074,#43075,#43076,#43077,#43078,
#43079,#43080,#43081,#43082,#43083,#43084,#43085,#43086,#43087,#43088,#43089,
#43090,#43091,#43092,#43093),.UNSPECIFIED.,.F.,.F.,(4,3,3,3,3,3,3,3,3,3,
3,3,3,3,3,3,3,3,3,3,3,4),(0.,0.107672209678887,0.125,0.170875355635446,
0.231002904544599,0.25,0.341726464788695,0.356352682078381,0.375,0.481320543933706,
0.5,0.512656877147315,0.606320543933732,0.625,0.683466200655585,0.731352682078384,
0.75,0.854340962716065,0.856002904544577,0.875,0.98267220967895,1.),
 .UNSPECIFIED.);
#479=B_SPLINE_CURVE_WITH_KNOTS('',3,(#43095,#43096,#43097,#43098,#43099,
#43100,#43101,#43102,#43103,#43104,#43105,#43106,#43107,#43108,#43109,#43110,
#43111,#43112,#43113,#43114,#43115,#43116,#43117,#43118,#43119,#43120,#43121,
#43122,#43123,#43124,#43125,#43126,#43127,#43128,#43129,#43130,#43131,#43132,
#43133,#43134,#43135,#43136,#43137,#43138,#43139,#43140,#43141,#43142,#43143),
 .UNSPECIFIED.,.F.,.F.,(4,3,3,3,3,3,3,3,3,3,3,3,3,3,3,3,4),(0.,0.0980957321441499,
0.125,0.221288934213747,0.25,0.346645006971691,0.375,0.471626821224367,
0.5,0.596626821224286,0.625,0.721645006972078,0.75,0.846288934213863,0.875,
0.973095732143744,1.),.UNSPECIFIED.);
#480=B_SPLINE_CURVE_WITH_KNOTS('',3,(#43145,#43146,#43147,#43148,#43149,
#43150,#43151,#43152,#43153,#43154,#43155,#43156,#43157,#43158,#43159,#43160,
#43161,#43162,#43163,#43164,#43165,#43166,#43167,#43168,#43169,#43170,#43171,
#43172,#43173,#43174,#43175,#43176,#43177,#43178,#43179,#43180,#43181,#43182,
#43183,#43184,#43185,#43186,#43187,#43188,#43189,#43190,#43191,#43192,#43193),
 .UNSPECIFIED.,.F.,.F.,(4,3,3,3,3,3,3,3,3,3,3,3,3,3,3,3,4),(3.47866587965213E-7,
0.0980732301818695,0.125,0.221270685953323,0.25,0.346629928815369,0.375,
0.471532576649637,0.5,0.596793963593996,0.625,0.721485590978993,0.75,0.846265350404548,
0.875,0.973064073364032,0.999998966090638),.UNSPECIFIED.);
#481=B_SPLINE_CURVE_WITH_KNOTS('',3,(#43195,#43196,#43197,#43198,#43199,
#43200,#43201,#43202,#43203,#43204,#43205,#43206,#43207,#43208,#43209,#43210,
#43211,#43212,#43213,#43214,#43215,#43216,#43217,#43218,#43219,#43220,#43221,
#43222,#43223,#43224,#43225,#43226,#43227,#43228,#43229,#43230,#43231,#43232,
#43233,#43234,#43235,#43236,#43237,#43238,#43239,#43240,#43241,#43242,#43243),
 .UNSPECIFIED.,.F.,.F.,(4,3,3,3,3,3,3,3,3,3,3,3,3,3,3,3,4),(0.,0.0980882716237501,
0.125,0.221281359117661,0.25,0.346637434313584,0.375,0.471619261957286,
0.5,0.596619261956614,0.625,0.721637434313737,0.75,0.84628135911775,0.875,
0.973088271625478,1.),.UNSPECIFIED.);
#482=B_SPLINE_CURVE_WITH_KNOTS('',3,(#43245,#43246,#43247,#43248,#43249,
#43250,#43251,#43252,#43253,#43254,#43255,#43256,#43257,#43258,#43259,#43260,
#43261,#43262,#43263,#43264,#43265,#43266,#43267,#43268,#43269,#43270,#43271,
#43272,#43273,#43274,#43275,#43276,#43277,#43278,#43279,#43280,#43281,#43282,
#43283,#43284,#43285,#43286,#43287,#43288,#43289,#43290,#43291,#43292,#43293),
 .UNSPECIFIED.,.F.,.F.,(4,3,3,3,3,3,3,3,3,3,3,3,3,3,3,3,4),(0.,0.0980731050085886,
0.125,0.221265959541012,0.25,0.346622039677989,0.375,0.471603894557442,
0.5,0.596603894557873,0.625,0.721622039678259,0.75,0.846265959541324,0.875,
0.973073105008618,1.),.UNSPECIFIED.);
#483=B_SPLINE_CURVE_WITH_KNOTS('',3,(#43295,#43296,#43297,#43298,#43299,
#43300,#43301,#43302,#43303,#43304,#43305,#43306,#43307,#43308,#43309,#43310,
#43311,#43312,#43313,#43314,#43315,#43316,#43317,#43318,#43319,#43320,#43321,
#43322,#43323,#43324,#43325,#43326,#43327,#43328,#43329,#43330,#43331,#43332,
#43333,#43334,#43335,#43336,#43337,#43338,#43339,#43340,#43341,#43342,#43343),
 .UNSPECIFIED.,.F.,.F.,(4,3,3,3,3,3,3,3,3,3,3,3,3,3,3,3,4),(3.58622363903863E-7,
0.111115124155117,0.125,0.234490512890156,0.25,0.359836869680777,0.375,
0.484801042762829,0.5,0.609801042765287,0.625,0.734836869676075,0.75,0.859490512890428,
0.875,0.986114767852758,0.999999885501399),.UNSPECIFIED.);
#484=B_SPLINE_CURVE_WITH_KNOTS('',3,(#43347,#43348,#43349,#43350,#43351,
#43352,#43353,#43354,#43355,#43356,#43357,#43358,#43359,#43360,#43361,#43362,
#43363,#43364,#43365,#43366,#43367,#43368,#43369,#43370,#43371,#43372,#43373,
#43374,#43375,#43376,#43377,#43378,#43379,#43380),.UNSPECIFIED.,.F.,.F.,
(4,3,3,3,3,3,3,3,3,3,3,4),(3.20858793336893E-13,0.16551266710415,0.25,0.265228163927209,
0.411286989585918,0.5,0.530572838575572,0.661286989585927,0.75,0.795852056859227,
0.915512667103842,1.),.UNSPECIFIED.);
#485=B_SPLINE_CURVE_WITH_KNOTS('',3,(#43381,#43382,#43383,#43384,#43385,
#43386,#43387,#43388,#43389,#43390,#43391,#43392,#43393,#43394,#43395,#43396,
#43397,#43398,#43399,#43400,#43401,#43402,#43403,#43404,#43405,#43406,#43407,
#43408,#43409,#43410,#43411,#43412,#43413,#43414,#43415,#43416,#43417,#43418,
#43419,#43420,#43421,#43422,#43423,#43424,#43425,#43426,#43427,#43428,#43429,
#43430,#43431,#43432,#43433,#43434,#43435,#43436,#43437,#43438,#43439,#43440,
#43441,#43442,#43443,#43444,#43445,#43446,#43447,#43448,#43449,#43450,#43451,
#43452,#43453,#43454,#43455,#43456,#43457,#43458,#43459,#43460,#43461,#43462,
#43463,#43464,#43465,#43466,#43467,#43468,#43469,#43470,#43471,#43472,#43473,
#43474,#43475,#43476,#43477,#43478,#43479,#43480,#43481,#43482,#43483,#43484,
#43485,#43486,#43487,#43488,#43489,#43490,#43491,#43492,#43493,#43494,#43495,
#43496,#43497,#43498,#43499,#43500,#43501,#43502,#43503,#43504,#43505,#43506,
#43507,#43508,#43509,#43510,#43511,#43512,#43513,#43514,#43515,#43516,#43517,
#43518,#43519,#43520,#43521,#43522),.UNSPECIFIED.,.F.,.F.,(4,2,2,2,2,2,
2,2,2,2,2,2,2,2,2,2,2,2,2,2,2,2,2,2,2,2,2,2,2,2,2,2,2,2,2,2,2,2,2,2,2,2,
2,2,2,2,2,2,2,2,2,2,2,2,2,2,2,2,2,2,2,2,2,2,2,2,2,2,2,2,4),(-1.26096989666227,
-1.22707058127239,-1.21883665098304,-1.21289954999642,-1.20452617599143,
-1.17050362623785,-1.13505788761883,-1.12240658005665,-1.11212247487635,
-1.09914117067393,-1.05877205797667,-1.03006717083556,-1.02178707012923,
-1.01585312011901,-1.00753612548882,-0.972574059078231,-0.937995783116275,
-0.925203432258212,-0.914816294073501,-0.901684245354329,-0.86289631062092,
-0.83290071502599,-0.82478680774899,-0.818805855652598,-0.810142260707499,
-0.786096075401545,-0.755904654055759,-0.73597095185452,-0.724797129082856,
-0.714207929993758,-0.697763307221352,-0.65614157148257,-0.641239193444398,
-0.630465011268126,-0.62487137855747,-0.618203007845375,-0.604447950817056,
-0.582238896381285,-0.545920399853265,-0.532768230208396,-0.522410230839679,
-0.509928389110634,-0.472994950077797,-0.439951546199994,-0.431462167963196,
-0.425506067265656,-0.417314381788017,-0.388017161369834,-0.348366600927986,
-0.335298804060168,-0.324936578735646,-0.312152912192802,-0.297732041447513,
-0.267499207795241,-0.243457877537951,-0.234795503786561,-0.22882907817729,
-0.220770488928708,-0.19100223684165,-0.151594040354065,-0.138510634584796,
-0.128153541750447,-0.115399159575225,-0.101026582114009,-0.0710352414085446,
-0.0446772738205007,-0.0369488222373959,-0.0309729674374409,-0.0248730602270775,
-0.0160319166381245,-2.50941038643732E-5),.UNSPECIFIED.);
#486=B_SPLINE_CURVE_WITH_KNOTS('',3,(#43593,#43594,#43595,#43596,#43597,
#43598,#43599,#43600,#43601,#43602,#43603,#43604,#43605,#43606,#43607,#43608),
 .UNSPECIFIED.,.F.,.F.,(4,2,2,2,2,2,2,4),(0.500000149075164,0.571383311424569,
0.625,0.714192063098084,0.75,0.857080176928947,0.875,1.),.UNSPECIFIED.);
#487=B_SPLINE_CURVE_WITH_KNOTS('',3,(#43838,#43839,#43840,#43841,#43842,
#43843,#43844),.UNSPECIFIED.,.F.,.F.,(4,1,1,1,4),(-1.,-0.785714285714286,
-0.571428571428571,-0.285714285714286,3.18349790973116E-11),
 .UNSPECIFIED.);
#488=B_SPLINE_CURVE_WITH_KNOTS('',3,(#43883,#43884,#43885,#43886,#43887,
#43888),.UNSPECIFIED.,.F.,.F.,(4,2,4),(0.000117088579411485,0.000909402471215065,
0.00174490984546788),.UNSPECIFIED.);
#489=B_SPLINE_CURVE_WITH_KNOTS('',3,(#43890,#43891,#43892,#43893,#43894,
#43895,#43896,#43897,#43898,#43899,#43900,#43901,#43902,#43903,#43904,#43905,
#43906,#43907,#43908,#43909,#43910,#43911,#43912,#43913,#43914,#43915,#43916,
#43917,#43918,#43919,#43920,#43921,#43922,#43923,#43924,#43925,#43926,#43927,
#43928,#43929,#43930,#43931,#43932,#43933,#43934,#43935),.UNSPECIFIED.,
 .F.,.F.,(4,3,3,3,3,3,3,3,3,3,3,3,3,3,3,4),(-0.409631076264667,-0.385380122364829,
-0.3409735646143,-0.331279738066214,-0.326505129564108,-0.260525143680311,
-0.251715173498639,-0.247659301762696,-0.223884696358354,-0.211563155315766,
-0.163804628915719,-0.160094298147174,-0.0805484267240998,-0.0768764939308757,
-0.0110461773969077,0.),.UNSPECIFIED.);
#490=B_SPLINE_CURVE_WITH_KNOTS('',3,(#43936,#43937,#43938,#43939,#43940,
#43941,#43942,#43943,#43944,#43945,#43946,#43947,#43948,#43949,#43950,#43951,
#43952,#43953,#43954,#43955,#43956,#43957,#43958,#43959,#43960,#43961,#43962,
#43963,#43964,#43965,#43966,#43967,#43968,#43969,#43970,#43971,#43972,#43973,
#43974,#43975,#43976,#43977,#43978,#43979,#43980,#43981,#43982,#43983,#43984,
#43985,#43986,#43987,#43988,#43989,#43990),.UNSPECIFIED.,.F.,.F.,(4,3,3,
3,3,3,3,3,3,3,3,3,3,3,3,3,3,3,4),(-0.413257902153422,-0.390922947181097,
-0.368527860933955,-0.351784161114064,-0.345070111406328,-0.3408068417481,
-0.279278028382547,-0.273184383320329,-0.269298985732011,-0.245026600124572,
-0.234578262374825,-0.197920862117467,-0.187270004319717,-0.183437118834528,
-0.0991669299111112,-0.0951172833893305,-0.0912706016525077,-0.0138375730600328,
0.),.UNSPECIFIED.);
#491=B_SPLINE_CURVE_WITH_KNOTS('',3,(#44159,#44160,#44161,#44162,#44163,
#44164,#44165,#44166,#44167,#44168,#44169,#44170,#44171,#44172,#44173,#44174,
#44175,#44176,#44177,#44178,#44179,#44180,#44181,#44182,#44183,#44184,#44185,
#44186,#44187,#44188,#44189,#44190,#44191,#44192,#44193,#44194,#44195,#44196,
#44197,#44198,#44199,#44200,#44201,#44202,#44203,#44204,#44205,#44206,#44207),
 .UNSPECIFIED.,.F.,.F.,(4,3,3,3,3,3,3,3,3,3,3,3,3,3,3,3,4),(-0.41325790215343,
-0.351784145825427,-0.345070539488157,-0.340806885032473,-0.279278049754355,
-0.273184457928296,-0.269298995380588,-0.245026610762357,-0.234578262374832,
-0.187269997389303,-0.183437116025571,-0.109052973926965,-0.0991668215785101,
-0.0951172236224628,-0.0912705901101731,-0.0138375948482117,0.),
 .UNSPECIFIED.);
#492=B_SPLINE_CURVE_WITH_KNOTS('',3,(#44209,#44210,#44211,#44212,#44213,
#44214,#44215,#44216,#44217,#44218,#44219,#44220,#44221,#44222,#44223,#44224,
#44225,#44226,#44227,#44228,#44229,#44230,#44231,#44232,#44233,#44234,#44235,
#44236,#44237,#44238,#44239,#44240,#44241,#44242,#44243,#44244,#44245,#44246,
#44247,#44248,#44249,#44250,#44251,#44252,#44253,#44254,#44255,#44256,#44257),
 .UNSPECIFIED.,.F.,.F.,(4,3,3,3,3,3,3,3,3,3,3,3,3,3,3,3,4),(-0.409631140621061,
-0.385380121304351,-0.340973570999351,-0.326505126071581,-0.260525176777292,
-0.251715206634708,-0.247659319036372,-0.223884748477094,-0.211563155315756,
-0.163804641724133,-0.160094308683559,-0.136551760510434,-0.113090562557914,
-0.0805484427544219,-0.0768765013185619,-0.0110460447264667,0.),
 .UNSPECIFIED.);
#493=B_SPLINE_CURVE_WITH_KNOTS('',3,(#44466,#44467,#44468,#44469,#44470,
#44471),.UNSPECIFIED.,.F.,.F.,(4,1,1,4),(0.,0.333333333333333,0.666666666666667,
1.),.UNSPECIFIED.);
#494=B_SPLINE_CURVE_WITH_KNOTS('',3,(#44473,#44474,#44475,#44476,#44477,
#44478),.UNSPECIFIED.,.F.,.F.,(4,1,1,4),(0.,0.333333333333333,0.666666666666667,
1.),.UNSPECIFIED.);
#495=B_SPLINE_CURVE_WITH_KNOTS('',3,(#44519,#44520,#44521,#44522,#44523,
#44524),.UNSPECIFIED.,.F.,.F.,(4,1,1,4),(0.,0.333333333333333,0.666666666666667,
1.),.UNSPECIFIED.);
#496=B_SPLINE_CURVE_WITH_KNOTS('',3,(#44565,#44566,#44567,#44568,#44569,
#44570),.UNSPECIFIED.,.F.,.F.,(4,1,1,4),(0.,0.333333333333333,0.666666666666667,
1.),.UNSPECIFIED.);
#497=B_SPLINE_CURVE_WITH_KNOTS('',3,(#44611,#44612,#44613,#44614,#44615,
#44616),.UNSPECIFIED.,.F.,.F.,(4,1,1,4),(0.,0.333333333333333,0.666666666666667,
1.),.UNSPECIFIED.);
#498=B_SPLINE_CURVE_WITH_KNOTS('',3,(#44657,#44658,#44659,#44660,#44661,
#44662),.UNSPECIFIED.,.F.,.F.,(4,1,1,4),(0.,0.333333333333333,0.666666666666667,
1.),.UNSPECIFIED.);
#499=B_SPLINE_CURVE_WITH_KNOTS('',3,(#44704,#44705,#44706,#44707,#44708,
#44709),.UNSPECIFIED.,.F.,.F.,(4,1,1,4),(0.,0.333333333333333,0.666666666666667,
1.),.UNSPECIFIED.);
#500=B_SPLINE_CURVE_WITH_KNOTS('',3,(#44711,#44712,#44713,#44714,#44715,
#44716),.UNSPECIFIED.,.F.,.F.,(4,1,1,4),(0.,0.333333333333333,0.666666666666667,
1.),.UNSPECIFIED.);
#501=B_SPLINE_CURVE_WITH_KNOTS('',3,(#44757,#44758,#44759,#44760,#44761,
#44762),.UNSPECIFIED.,.F.,.F.,(4,1,1,4),(0.,0.333333333333333,0.666666666666667,
1.),.UNSPECIFIED.);
#502=B_SPLINE_CURVE_WITH_KNOTS('',3,(#44803,#44804,#44805,#44806,#44807,
#44808),.UNSPECIFIED.,.F.,.F.,(4,1,1,4),(0.,0.333333333333333,0.666666666666667,
1.),.UNSPECIFIED.);
#503=B_SPLINE_CURVE_WITH_KNOTS('',3,(#44849,#44850,#44851,#44852,#44853,
#44854),.UNSPECIFIED.,.F.,.F.,(4,1,1,4),(0.,0.333333333333333,0.666666666666667,
1.),.UNSPECIFIED.);
#504=B_SPLINE_CURVE_WITH_KNOTS('',3,(#44895,#44896,#44897,#44898,#44899,
#44900),.UNSPECIFIED.,.F.,.F.,(4,1,1,4),(0.,0.333333333333333,0.666666666666667,
1.),.UNSPECIFIED.);
#505=B_SPLINE_CURVE_WITH_KNOTS('',3,(#44942,#44943,#44944,#44945,#44946,
#44947),.UNSPECIFIED.,.F.,.F.,(4,1,1,4),(0.,0.333333333333333,0.666666666666667,
1.),.UNSPECIFIED.);
#506=B_SPLINE_CURVE_WITH_KNOTS('',3,(#44949,#44950,#44951,#44952,#44953,
#44954),.UNSPECIFIED.,.F.,.F.,(4,1,1,4),(0.,0.333333333333333,0.666666666666667,
1.),.UNSPECIFIED.);
#507=B_SPLINE_CURVE_WITH_KNOTS('',3,(#44995,#44996,#44997,#44998,#44999,
#45000),.UNSPECIFIED.,.F.,.F.,(4,1,1,4),(0.,0.333333333333333,0.666666666666667,
1.),.UNSPECIFIED.);
#508=B_SPLINE_CURVE_WITH_KNOTS('',3,(#45041,#45042,#45043,#45044,#45045,
#45046),.UNSPECIFIED.,.F.,.F.,(4,1,1,4),(0.,0.333333333333333,0.666666666666667,
1.),.UNSPECIFIED.);
#509=B_SPLINE_CURVE_WITH_KNOTS('',3,(#45087,#45088,#45089,#45090,#45091,
#45092),.UNSPECIFIED.,.F.,.F.,(4,1,1,4),(0.,0.333333333333333,0.666666666666667,
1.),.UNSPECIFIED.);
#510=B_SPLINE_CURVE_WITH_KNOTS('',3,(#45133,#45134,#45135,#45136,#45137,
#45138),.UNSPECIFIED.,.F.,.F.,(4,1,1,4),(0.,0.333333333333333,0.666666666666667,
1.),.UNSPECIFIED.);
#511=B_SPLINE_CURVE_WITH_KNOTS('',3,(#45180,#45181,#45182,#45183,#45184,
#45185),.UNSPECIFIED.,.F.,.F.,(4,1,1,4),(0.,0.333333333333333,0.666666666666667,
1.),.UNSPECIFIED.);
#512=B_SPLINE_CURVE_WITH_KNOTS('',3,(#45187,#45188,#45189,#45190,#45191,
#45192),.UNSPECIFIED.,.F.,.F.,(4,1,1,4),(0.,0.333333333333333,0.666666666666667,
1.),.UNSPECIFIED.);
#513=B_SPLINE_CURVE_WITH_KNOTS('',3,(#45233,#45234,#45235,#45236,#45237,
#45238),.UNSPECIFIED.,.F.,.F.,(4,1,1,4),(0.,0.333333333333333,0.666666666666667,
1.),.UNSPECIFIED.);
#514=B_SPLINE_CURVE_WITH_KNOTS('',3,(#45279,#45280,#45281,#45282,#45283,
#45284),.UNSPECIFIED.,.F.,.F.,(4,1,1,4),(0.,0.333333333333333,0.666666666666667,
1.),.UNSPECIFIED.);
#515=B_SPLINE_CURVE_WITH_KNOTS('',3,(#45325,#45326,#45327,#45328,#45329,
#45330),.UNSPECIFIED.,.F.,.F.,(4,1,1,4),(0.,0.333333333333333,0.666666666666667,
1.),.UNSPECIFIED.);
#516=B_SPLINE_CURVE_WITH_KNOTS('',3,(#45371,#45372,#45373,#45374,#45375,
#45376),.UNSPECIFIED.,.F.,.F.,(4,1,1,4),(0.,0.333333333333333,0.666666666666667,
1.),.UNSPECIFIED.);
#517=B_SPLINE_CURVE_WITH_KNOTS('',3,(#45891,#45892,#45893,#45894,#45895,
#45896,#45897,#45898,#45899,#45900,#45901,#45902,#45903,#45904,#45905,#45906,
#45907,#45908,#45909,#45910),.UNSPECIFIED.,.F.,.F.,(4,2,2,2,2,2,2,2,2,4),
(-0.472680489487021,-0.421857921558036,-0.362870895179553,-0.305901838025028,
-0.246237725257386,-0.187898332264809,-0.130441066174416,-0.0704976060355538,
-0.0346474857024549,-9.9999999542133E-7),.UNSPECIFIED.);
#518=B_SPLINE_CURVE_WITH_KNOTS('',3,(#45913,#45914,#45915,#45916,#45917,
#45918,#45919,#45920,#45921,#45922,#45923,#45924,#45925,#45926,#45927,#45928),
 .UNSPECIFIED.,.F.,.F.,(4,2,2,2,2,2,2,4),(-14.4370592734888,-14.4037012578129,
-14.3709495751806,-14.3127127045736,-14.2529421093177,-14.1958485449995,
-14.1369603965429,-14.0806259388301),.UNSPECIFIED.);
#519=B_SPLINE_CURVE_WITH_KNOTS('',3,(#45933,#45934,#45935,#45936,#45937,
#45938,#45939,#45940,#45941,#45942,#45943,#45944,#45945,#45946,#45947,#45948,
#45949,#45950,#45951,#45952,#45953,#45954,#45955,#45956,#45957,#45958,#45959,
#45960,#45961,#45962,#45963,#45964,#45965,#45966,#45967,#45968,#45969,#45970),
 .UNSPECIFIED.,.F.,.F.,(4,2,2,2,2,2,2,2,2,2,2,2,2,2,2,2,2,2,4),(-1.41859832691229,
-1.41822527997428,-1.35855760366901,-1.29985891312466,-1.24273727568412,
-1.18301408218039,-1.12496822443588,-1.06682478961775,-1.00721544324156,
-0.949844979558046,-0.89017629567726,-0.831344294177192,-0.77434923288016,
-0.714670672924963,-0.656488509400857,-0.598748590473465,-0.538981330577316,
-0.481470031543986,-0.472680489487021),.UNSPECIFIED.);
#520=B_SPLINE_CURVE_WITH_KNOTS('',3,(#45971,#45972,#45973,#45974,#45975,
#45976,#45977,#45978,#45979,#45980,#45981,#45982,#45983,#45984,#45985,#45986,
#45987,#45988,#45989,#45990,#45991,#45992,#45993,#45994,#45995,#45996,#45997,
#45998,#45999,#46000,#46001,#46002,#46003,#46004,#46005,#46006,#46007,#46008),
 .UNSPECIFIED.,.F.,.F.,(4,2,2,2,2,2,2,2,2,2,2,2,2,2,2,2,2,2,4),(-14.0806259388301,
-14.0772027728482,-14.0197752809982,-13.9601089034145,-13.9017860811062,
-13.843680755693,-13.7832574713262,-13.7260330550825,-13.6672514254089,
-13.6074849557429,-13.5502487242808,-13.4908237302309,-13.432144117751,
-13.3742545460729,-13.3140698205319,-13.2567467237662,-13.198184782689,
-13.1384608998608,-13.133357359287),.UNSPECIFIED.);
#521=B_SPLINE_CURVE_WITH_KNOTS('',3,(#46013,#46014,#46015,#46016,#46017,
#46018,#46019,#46020,#46021,#46022,#46023,#46024,#46025,#46026,#46027,#46028,
#46029,#46030,#46031,#46032,#46033,#46034,#46035,#46036,#46037,#46038,#46039,
#46040,#46041,#46042,#46043,#46044,#46045,#46046,#46047,#46048),
 .UNSPECIFIED.,.F.,.F.,(4,2,2,2,2,2,2,2,2,2,2,2,2,2,2,2,2,4),(-2.36357121621961,
-2.35439216466225,-2.29478381910495,-2.23649866694068,-2.17909549669189,
-2.11920774560853,-2.06159204897073,-2.00258816172034,-1.94346622679962,
-1.8864802795193,-1.82685774819307,-1.76838058281947,-1.71116885123677,
-1.65107017816501,-1.59326446777019,-1.53472012633121,-1.47537944090739,
-1.41859832691229),.UNSPECIFIED.);
#522=B_SPLINE_CURVE_WITH_KNOTS('',3,(#46049,#46050,#46051,#46052,#46053,
#46054,#46055,#46056,#46057,#46058,#46059,#46060,#46061,#46062,#46063,#46064,
#46065,#46066,#46067,#46068,#46069,#46070,#46071,#46072,#46073,#46074,#46075,
#46076,#46077,#46078,#46079,#46080,#46081,#46082,#46083,#46084),
 .UNSPECIFIED.,.F.,.F.,(4,2,2,2,2,2,2,2,2,2,2,2,2,2,2,2,2,4),(-13.133357359287,
-13.081385357797,-13.0221773281264,-12.9630288925176,-12.905327227556,-12.8453511553982,
-12.7878283622088,-12.729456125551,-12.6697440428986,-12.6127306500945,
-12.5537100886643,-12.4940029413133,-12.4364567758814,-12.3766541658974,
-12.3188421358561,-12.2606243760745,-12.2008957709647,-12.1870122249769),
 .UNSPECIFIED.);
#523=B_SPLINE_CURVE_WITH_KNOTS('',3,(#46089,#46090,#46091,#46092,#46093,
#46094,#46095,#46096,#46097,#46098,#46099,#46100,#46101,#46102,#46103,#46104,
#46105,#46106,#46107,#46108,#46109,#46110,#46111,#46112,#46113,#46114,#46115,
#46116,#46117,#46118,#46119,#46120,#46121,#46122,#46123,#46124),
 .UNSPECIFIED.,.F.,.F.,(4,2,2,2,2,2,2,2,2,2,2,2,2,2,2,2,2,4),(-3.30848554402564,
-3.29034972008339,-3.23068257001005,-3.1726908982952,-3.11460265690008,
-3.05504892530917,-2.99773200432777,-2.93811923868514,-2.8793421277137,
-2.82240057354888,-2.76277796537348,-2.70465007979412,-2.64696477699234,
-2.58725324895101,-2.52979559565241,-2.47024018500225,-2.41130800830289,
-2.36357121621961),.UNSPECIFIED.);
#524=B_SPLINE_CURVE_WITH_KNOTS('',3,(#46125,#46126,#46127,#46128,#46129,
#46130,#46131,#46132,#46133,#46134,#46135,#46136,#46137,#46138,#46139,#46140,
#46141,#46142,#46143,#46144,#46145,#46146,#46147,#46148,#46149,#46150,#46151,
#46152,#46153,#46154,#46155,#46156,#46157,#46158,#46159,#46160),
 .UNSPECIFIED.,.F.,.F.,(4,2,2,2,2,2,2,2,2,2,2,2,2,2,2,2,2,4),(-12.1870122249769,
-12.1438492432235,-12.0849809374751,-12.0246571711172,-11.9672296348607,
-11.9075603623266,-11.8493922713876,-11.7912891282832,-11.731517449561,
-11.6743561420471,-11.6155998003076,-11.5558844962949,-11.4986749070985,
-11.4392762960987,-11.3807140133877,-11.3228531755694,-11.2626963209889,
-11.2404440616607),.UNSPECIFIED.);
#525=B_SPLINE_CURVE_WITH_KNOTS('',3,(#46165,#46166,#46167,#46168,#46169,
#46170,#46171,#46172,#46173,#46174,#46175,#46176,#46177,#46178,#46179,#46180,
#46181,#46182,#46183,#46184,#46185,#46186,#46187,#46188,#46189,#46190,#46191,
#46192,#46193,#46194,#46195,#46196,#46197,#46198,#46199,#46200),
 .UNSPECIFIED.,.F.,.F.,(4,2,2,2,2,2,2,2,2,2,2,2,2,2,2,2,2,4),(-4.2528209750252,
-4.2258289954172,-4.16599723540487,-4.10843542684453,-4.04948791774649,
-3.99042123507979,-3.93348867864914,-3.87392217476687,-3.81549965097264,
-3.75834197483301,-3.69829943582703,-3.64054774097401,-3.58205916445528,
-3.52277389154611,-3.46567311490864,-3.4060614524971,-3.34741756521746,
-3.30848554402564),.UNSPECIFIED.);
#526=B_SPLINE_CURVE_WITH_KNOTS('',3,(#46201,#46202,#46203,#46204,#46205,
#46206,#46207,#46208,#46209,#46210,#46211,#46212,#46213,#46214,#46215,#46216,
#46217,#46218,#46219,#46220,#46221,#46222,#46223,#46224,#46225,#46226,#46227,
#46228,#46229,#46230,#46231,#46232,#46233,#46234,#46235,#46236),
 .UNSPECIFIED.,.F.,.F.,(4,2,2,2,2,2,2,2,2,2,2,2,2,2,2,2,2,4),(-11.2404440616607,
-11.2054512613555,-11.1469182749413,-11.0872501668356,-11.0302148159706,
-10.9710367406564,-10.9120211179477,-10.854352265994,-10.7944084679723,
-10.7369779084177,-10.6786390615402,-10.6189869936286,-10.5620279497738,
-10.5030417379351,-10.4434790671637,-10.3859704970566,-10.3262053607749,
-10.2949578972094),.UNSPECIFIED.);
#527=B_SPLINE_CURVE_WITH_KNOTS('',3,(#46241,#46242,#46243,#46244,#46245,
#46246,#46247,#46248,#46249,#46250,#46251,#46252,#46253,#46254,#46255,#46256,
#46257,#46258,#46259,#46260,#46261,#46262,#46263,#46264,#46265,#46266,#46267,
#46268,#46269,#46270,#46271,#46272,#46273,#46274,#46275,#46276),
 .UNSPECIFIED.,.F.,.F.,(4,2,2,2,2,2,2,2,2,2,2,2,2,2,2,2,2,4),(-5.19675137828244,
-5.16045616765585,-5.10095821008514,-5.04369498598246,-4.98413831157424,
-4.92541624835806,-4.86852837157201,-4.80896188953764,-4.75088843704952,
-4.6932579452808,-4.63360230711379,-4.57619845256742,-4.5167000729659,-4.4578230250715,
-4.40096067746688,-4.34140839720388,-4.28317776156472,-4.2528209750252),
 .UNSPECIFIED.);
#528=B_SPLINE_CURVE_WITH_KNOTS('',3,(#46277,#46278,#46279,#46280,#46281,
#46282,#46283,#46284,#46285,#46286,#46287,#46288,#46289,#46290,#46291,#46292,
#46293,#46294,#46295,#46296,#46297,#46298,#46299,#46300,#46301,#46302,#46303,
#46304,#46305,#46306,#46307,#46308,#46309,#46310,#46311,#46312),
 .UNSPECIFIED.,.F.,.F.,(4,2,2,2,2,2,2,2,2,2,2,2,2,2,2,2,2,4),(-10.2949578972094,
-10.2684975889558,-10.2103184315637,-10.1506537980798,-10.0936746957517,
-10.0348459812853,-9.97467345304288,-9.91728892738338,-9.85766301371066,
-9.79960748007447,-9.74154877508422,-9.68184483516709,-9.62476165993561,
-9.56605083144069,-9.50636878850725,-9.44910648683061,-9.38961853093635,
-9.34899662094938),.UNSPECIFIED.);
#529=B_SPLINE_CURVE_WITH_KNOTS('',3,(#46317,#46318,#46319,#46320,#46321,
#46322,#46323,#46324,#46325,#46326,#46327,#46328,#46329,#46330,#46331,#46332,
#46333,#46334,#46335,#46336,#46337,#46338,#46339,#46340,#46341,#46342,#46343,
#46344,#46345,#46346,#46347,#46348,#46349,#46350,#46351,#46352),
 .UNSPECIFIED.,.F.,.F.,(4,2,2,2,2,2,2,2,2,2,2,2,2,2,2,2,2,4),(-6.14044228887836,
-6.09446054161853,-6.03544927417801,-5.97857027285831,-5.91905997766185,
-5.86069225619341,-5.80358882530382,-5.74360258432422,-5.68590506399478,
-5.62747247135089,-5.56824277211902,-5.51119553553071,-5.4516400653047,
-5.39305114016943,-5.33603726706465,-5.27642633763462,-5.21848900864112,
-5.19675137828244),.UNSPECIFIED.);
#530=B_SPLINE_CURVE_WITH_KNOTS('',3,(#46353,#46354,#46355,#46356,#46357,
#46358,#46359,#46360,#46361,#46362,#46363,#46364,#46365,#46366,#46367,#46368,
#46369,#46370,#46371,#46372,#46373,#46374,#46375,#46376,#46377,#46378,#46379,
#46380,#46381,#46382,#46383,#46384,#46385,#46386,#46387,#46388),
 .UNSPECIFIED.,.F.,.F.,(4,2,2,2,2,2,2,2,2,2,2,2,2,2,2,2,2,4),(-9.34899662094938,
-9.33105074122771,-9.2731055957996,-9.21285922380668,-9.15557513902431,
-9.09695672998933,-9.03722574734233,-8.98011691943174,-8.92085312448608,
-8.86184579512779,-8.80409668210845,-8.74406773839571,-8.6866111034004,
-8.62819119904668,-8.56848024689387,-8.51146096604764,-8.45239334999859,
-8.40244442487571),.UNSPECIFIED.);
#531=B_SPLINE_CURVE_WITH_KNOTS('',3,(#46393,#46394,#46395,#46396,#46397,
#46398,#46399,#46400,#46401,#46402,#46403,#46404,#46405,#46406,#46407,#46408,
#46409,#46410,#46411,#46412,#46413,#46414,#46415,#46416,#46417,#46418,#46419,
#46420,#46421,#46422,#46423,#46424,#46425,#46426,#46427,#46428),
 .UNSPECIFIED.,.F.,.F.,(4,2,2,2,2,2,2,2,2,2,2,2,2,2,2,2,2,4),(-7.08338076536595,
-7.02822732374101,-6.96956047673802,-6.91272645955143,-6.85321629033566,
-6.79519743717148,-6.73762196486497,-6.67802238589634,-6.62067249405759,
-6.5612313850799,-6.50240963138312,-6.44560095327405,-6.38610492232616,
-6.32792896640202,-6.27063480406051,-6.21085920145596,-6.15335144217075,
-6.14044228887836),.UNSPECIFIED.);
#532=B_SPLINE_CURVE_WITH_KNOTS('',3,(#46429,#46430,#46431,#46432,#46433,
#46434,#46435,#46436,#46437,#46438,#46439,#46440,#46441,#46442,#46443,#46444,
#46445,#46446,#46447,#46448,#46449,#46450,#46451,#46452,#46453,#46454,#46455,
#46456,#46457,#46458,#46459,#46460,#46461,#46462,#46463,#46464),
 .UNSPECIFIED.,.F.,.F.,(4,2,2,2,2,2,2,2,2,2,2,2,2,2,2,2,2,4),(-8.40244442487571,
-8.39284926891096,-8.33526507147472,-8.2754198338689,-8.21769694693658,
-8.15944175694345,-8.09972190021169,-8.04269482223153,-7.98378974191723,
-7.92364153499131,-7.86618654884418,-7.80648615931792,-7.74842299103831,
-7.69029380781885,-7.63053806985166,-7.57341695923763,-7.51463538863381,
-7.45587725387744),.UNSPECIFIED.);
#533=B_SPLINE_CURVE_WITH_KNOTS('',3,(#46469,#46470,#46471,#46472,#46473,
#46474,#46475,#46476,#46477,#46478,#46479,#46480,#46481,#46482,#46483,#46484,
#46485,#46486,#46487,#46488,#46489,#46490,#46491,#46492,#46493,#46494,#46495,
#46496,#46497,#46498,#46499,#46500,#46501,#46502,#46503,#46504,#46505,#46506),
 .UNSPECIFIED.,.F.,.F.,(4,2,2,2,2,2,2,2,2,2,2,2,2,2,2,2,2,2,4),(-8.02645494637709,
-8.02062061883662,-7.96340867156997,-7.903960246378,-7.84617097437453,-7.78828802935107,
-7.72879472313259,-7.67192938925804,-7.6133970541528,-7.55392347512622,
-7.4968374534328,-7.43753093954167,-7.3792524025024,-7.32148761472472,-7.26142618244933,
-7.20437909686838,-7.14493708373042,-7.08772772168777,-7.08338076536595),
 .UNSPECIFIED.);
#534=B_SPLINE_CURVE_WITH_KNOTS('',3,(#46507,#46508,#46509,#46510,#46511,
#46512,#46513,#46514,#46515,#46516,#46517,#46518,#46519,#46520,#46521,#46522,
#46523,#46524,#46525,#46526,#46527,#46528,#46529,#46530,#46531,#46532,#46533,
#46534,#46535,#46536,#46537,#46538,#46539,#46540,#46541,#46542,#46543,#46544),
 .UNSPECIFIED.,.F.,.F.,(4,2,2,2,2,2,2,2,2,2,2,2,2,2,2,2,2,2,4),(-7.45587725387744,
-7.45490013693559,-7.39757036603791,-7.33801115408158,-7.27944992870555,
-7.22143789013388,-7.16324228872916,-7.10513370792117,-7.04536440843998,
-6.98784351644384,-6.92765908972021,-6.86868506825907,-6.81159972067067,
-6.75181742847008,-6.69349388764354,-6.63572323919473,-6.57580712348971,
-6.51815521566034,-6.50836887295495),.UNSPECIFIED.);
#535=B_SPLINE_CURVE_WITH_KNOTS('',3,(#46549,#46550,#46551,#46552,#46553,
#46554,#46555,#46556,#46557,#46558,#46559,#46560,#46561,#46562,#46563,#46564,
#46565,#46566,#46567,#46568,#46569,#46570,#46571,#46572,#46573,#46574,#46575,
#46576,#46577,#46578,#46579,#46580,#46581,#46582,#46583,#46584),
 .UNSPECIFIED.,.F.,.F.,(4,2,2,2,2,2,2,2,2,2,2,2,2,2,2,2,2,4),(-8.96867340698881,
-8.954726041388,-8.89721705486442,-8.83743694489446,-8.7802428260537,-8.72206588455876,
-8.66261397449903,-8.6058398735651,-8.54701816312532,-8.48776662644217,
-8.43042380514485,-8.37082874094838,-8.31337464233727,-8.2553638382111,
-8.195904708086,-8.13912837602821,-8.08047063786001,-8.02645494637709),
 .UNSPECIFIED.);
#536=B_SPLINE_CURVE_WITH_KNOTS('',3,(#46585,#46586,#46587,#46588,#46589,
#46590,#46591,#46592,#46593,#46594,#46595,#46596,#46597,#46598,#46599,#46600,
#46601,#46602,#46603,#46604,#46605,#46606,#46607,#46608,#46609,#46610,#46611,
#46612,#46613,#46614,#46615,#46616,#46617,#46618,#46619,#46620),
 .UNSPECIFIED.,.F.,.F.,(4,2,2,2,2,2,2,2,2,2,2,2,2,2,2,2,2,4),(-6.50836887295495,
-6.45857330656199,-6.39943496988036,-6.34235328727518,-6.28257867687266,
-6.2240886431033,-6.16658070395808,-6.10647908395784,-6.0486606110832,-5.98961229240173,
-5.93027621485651,-5.87310049918669,-5.81330450149875,-5.75461438102413,
-5.69727475870434,-5.63695411223535,-5.57893812995217,-5.56079052540277),
 .UNSPECIFIED.);
#537=B_SPLINE_CURVE_WITH_KNOTS('',3,(#46625,#46626,#46627,#46628,#46629,
#46630,#46631,#46632,#46633,#46634,#46635,#46636,#46637,#46638,#46639,#46640,
#46641,#46642,#46643,#46644,#46645,#46646,#46647,#46648,#46649,#46650,#46651,
#46652,#46653,#46654,#46655,#46656,#46657,#46658,#46659,#46660),
 .UNSPECIFIED.,.F.,.F.,(4,2,2,2,2,2,2,2,2,2,2,2,2,2,2,2,2,4),(-9.91116502693244,
-9.88848172659285,-9.83066113567844,-9.77121178531178,-9.71437759038781,
-9.65590780022673,-9.59647959088436,-9.53945310607522,-9.48020958718447,
-9.42191865790845,-9.36421279874568,-9.30421438211681,-9.24718616399223,
-9.18880975199588,-9.12933611442946,-9.07246699404788,-9.01344815245977,
-8.96867340698881),.UNSPECIFIED.);
#538=B_SPLINE_CURVE_WITH_KNOTS('',3,(#46661,#46662,#46663,#46664,#46665,
#46666,#46667,#46668,#46669,#46670,#46671,#46672,#46673,#46674,#46675,#46676,
#46677,#46678,#46679,#46680,#46681,#46682,#46683,#46684,#46685,#46686,#46687,
#46688,#46689,#46690,#46691,#46692,#46693,#46694,#46695,#46696),
 .UNSPECIFIED.,.F.,.F.,(4,2,2,2,2,2,2,2,2,2,2,2,2,2,2,2,2,4),(-5.56079052540277,
-5.52032499325248,-5.46076339888321,-5.40343060697284,-5.34368112976859,
-5.28489746921949,-5.22775446056634,-5.16798355663942,-5.10985264323955,
-5.05174717925448,-4.99204636464476,-4.93459018081613,-4.8743772890817,
-4.815473646124,-4.75843127614468,-4.6986984995855,-4.64044506045571,-4.61376150694468),
 .UNSPECIFIED.);
#539=B_SPLINE_CURVE_WITH_KNOTS('',3,(#46701,#46702,#46703,#46704,#46705,
#46706,#46707,#46708,#46709,#46710,#46711,#46712,#46713,#46714,#46715,#46716,
#46717,#46718,#46719,#46720,#46721,#46722,#46723,#46724,#46725,#46726,#46727,
#46728,#46729,#46730,#46731,#46732,#46733,#46734,#46735,#46736),
 .UNSPECIFIED.,.F.,.F.,(4,2,2,2,2,2,2,2,2,2,2,2,2,2,2,2,2,4),(-10.8526636518455,
-10.8218563382694,-10.763751898801,-10.7043508376338,-10.6476297274538,
-10.5888807841235,-10.5296053803888,-10.4723299070045,-10.4128063061383,
-10.3553612254831,-10.2974181137557,-10.2380062710185,-10.1812709618512,
-10.1226811718715,-10.0628013902258,-10.0056518305266,-9.94626946773807,
-9.91116502693244),.UNSPECIFIED.);
#540=B_SPLINE_CURVE_WITH_KNOTS('',3,(#46737,#46738,#46739,#46740,#46741,
#46742,#46743,#46744,#46745,#46746,#46747,#46748,#46749,#46750,#46751,#46752,
#46753,#46754,#46755,#46756,#46757,#46758,#46759,#46760,#46761,#46762,#46763,
#46764,#46765,#46766,#46767,#46768,#46769,#46770,#46771,#46772),
 .UNSPECIFIED.,.F.,.F.,(4,2,2,2,2,2,2,2,2,2,2,2,2,2,2,2,2,4),(-4.61376150694468,
-4.58268504394349,-4.52284289180626,-4.46526072397115,-4.40565622753905,
-4.34659316243956,-4.28956654669504,-4.22984505241611,-4.17143000304458,
-4.11394358291504,-4.05392082544131,-3.99617659372884,-3.93711600484904,
-3.87785937905479,-3.82075170408198,-3.76101274778027,-3.7024018430971,
-3.66716520277466),.UNSPECIFIED.);
#541=B_SPLINE_CURVE_WITH_KNOTS('',3,(#46777,#46778,#46779,#46780,#46781,
#46782,#46783,#46784,#46785,#46786,#46787,#46788,#46789,#46790,#46791,#46792,
#46793,#46794,#46795,#46796,#46797,#46798,#46799,#46800,#46801,#46802,#46803,
#46804,#46805,#46806,#46807,#46808,#46809,#46810,#46811,#46812),
 .UNSPECIFIED.,.F.,.F.,(4,2,2,2,2,2,2,2,2,2,2,2,2,2,2,2,2,4),(-11.7943289504834,
-11.7550760696795,-11.6966860285444,-11.6373196802076,-11.5803693805583,
-11.5212061909831,-11.4629152278514,-11.4052850124585,-11.345367052905,
-11.2883712953563,-11.2300715499567,-11.1706526443042,-11.1138493310695,
-11.0549073697268,-10.9961716612307,-10.9387344559412,-10.8790306340246,
-10.8526636518455),.UNSPECIFIED.);
#542=B_SPLINE_CURVE_WITH_KNOTS('',3,(#46813,#46814,#46815,#46816,#46817,
#46818,#46819,#46820,#46821,#46822,#46823,#46824,#46825,#46826,#46827,#46828,
#46829,#46830,#46831,#46832,#46833,#46834,#46835,#46836,#46837,#46838,#46839,
#46840,#46841,#46842,#46843,#46844,#46845,#46846,#46847,#46848),
 .UNSPECIFIED.,.F.,.F.,(4,2,2,2,2,2,2,2,2,2,2,2,2,2,2,2,2,4),(-3.66716520277466,
-3.64509650595974,-3.58485895842258,-3.52692114130706,-3.46830941132696,
-3.40883077564351,-3.35157668733905,-3.29189146511806,-3.23319016450654,
-3.17609457994864,-3.11638652761123,-3.05833760937658,-3.00024818247934,
-2.94063377994132,-2.8832595066928,-2.82302963638987,-2.76421431619143,
-2.72088258416467),.UNSPECIFIED.);
#543=B_SPLINE_CURVE_WITH_KNOTS('',3,(#46853,#46854,#46855,#46856,#46857,
#46858,#46859,#46860,#46861,#46862,#46863,#46864,#46865,#46866,#46867,#46868,
#46869,#46870,#46871,#46872,#46873,#46874,#46875,#46876,#46877,#46878,#46879,
#46880,#46881,#46882,#46883,#46884,#46885,#46886,#46887,#46888),
 .UNSPECIFIED.,.F.,.F.,(4,2,2,2,2,2,2,2,2,2,2,2,2,2,2,2,2,4),(-12.7348788498405,
-12.6874188698587,-12.6287608191211,-12.5694727238362,-12.512281974616,
-12.4528479617241,-12.3954247373668,-12.337566819066,-12.2782189630685,
-12.2215392485701,-12.1630350707807,-12.1031371006023,-12.0460668731077,
-11.986768228256,-11.9289949150521,-11.8712537287554,-11.8118648425648,
-11.7943289504834),.UNSPECIFIED.);
#544=B_SPLINE_CURVE_WITH_KNOTS('',3,(#46889,#46890,#46891,#46892,#46893,
#46894,#46895,#46896,#46897,#46898,#46899,#46900,#46901,#46902,#46903,#46904,
#46905,#46906,#46907,#46908,#46909,#46910,#46911,#46912,#46913,#46914,#46915,
#46916,#46917,#46918,#46919,#46920,#46921,#46922,#46923,#46924),
 .UNSPECIFIED.,.F.,.F.,(4,2,2,2,2,2,2,2,2,2,2,2,2,2,2,2,2,4),(-2.72088258416467,
-2.70722964809425,-2.64756329476097,-2.58939773754221,-2.53166122802283,
-2.47191145895106,-2.41441668652848,-2.3548006927746,-2.29583132696041,
-2.23887512009193,-2.17922386530305,-2.12090205431747,-2.06345033675333,
-2.00352534511469,-1.94587345157856,-1.88681170049432,-1.82765340162895,
-1.77549971424008),.UNSPECIFIED.);
#545=B_SPLINE_CURVE_WITH_KNOTS('',3,(#46929,#46930,#46931,#46932,#46933,
#46934,#46935,#46936,#46937,#46938,#46939,#46940,#46941,#46942,#46943,#46944,
#46945,#46946,#46947,#46948,#46949,#46950,#46951,#46952,#46953,#46954,#46955,
#46956,#46957,#46958,#46959,#46960,#46961,#46962,#46963,#46964),
 .UNSPECIFIED.,.F.,.F.,(4,2,2,2,2,2,2,2,2,2,2,2,2,2,2,2,2,4),(-13.6754849562843,
-13.6190227092761,-13.5599587753475,-13.5016793981831,-13.4441430123469,
-13.3843245242679,-13.3273749651957,-13.269170262857,-13.2098232086566,
-13.1531017200101,-13.0942551920742,-13.0355170596057,-12.978169433214,
-12.9185604858425,-12.8614191319234,-12.8034051476152,-12.7440718372722,
-12.7348788498405),.UNSPECIFIED.);
#546=B_SPLINE_CURVE_WITH_KNOTS('',3,(#46965,#46966,#46967,#46968,#46969,
#46970,#46971,#46972,#46973,#46974,#46975,#46976,#46977,#46978,#46979,#46980,
#46981,#46982,#46983,#46984,#46985,#46986,#46987,#46988,#46989,#46990,#46991,
#46992,#46993,#46994,#46995,#46996,#46997,#46998,#46999,#47000,#47001,#47002),
 .UNSPECIFIED.,.F.,.F.,(4,2,2,2,2,2,2,2,2,2,2,2,2,2,2,2,2,2,4),(-1.77549971424008,
-1.77063002140922,-1.71096546150082,-1.65245246961115,-1.59519526069461,
-1.53506016305706,-1.4772190143837,-1.41862028356561,-1.35924387185229,
-1.30205503267682,-1.2423462699575,-1.18361240910777,-1.12644846804497,
-1.06607365316599,-1.00801565210581,-0.949767234086745,-0.890148542862124,
-0.832767419266973,-0.829142789718882),.UNSPECIFIED.);
#547=B_SPLINE_CURVE_WITH_KNOTS('',3,(#47008,#47009,#47010,#47011,#47012,
#47013,#47014,#47015,#47016,#47017,#47018,#47019,#47020,#47021,#47022,#47023,
#47024,#47025,#47026,#47027),.UNSPECIFIED.,.F.,.F.,(4,2,2,2,2,2,2,2,2,4),
(11.4063709592788,11.4483123767435,11.4945291489478,11.5392425816036,11.5860765085847,
11.6317930050088,11.6770207952941,11.723975630726,11.7607854872426,11.7962920971555),
 .UNSPECIFIED.);
#548=B_SPLINE_CURVE_WITH_KNOTS('',3,(#47030,#47031,#47032,#47033,#47034,
#47035,#47036,#47037,#47038,#47039,#47040,#47041,#47042,#47043,#47044,#47045,
#47046,#47047),.UNSPECIFIED.,.F.,.F.,(4,2,2,2,2,2,2,2,4),(0.,0.0289335200264656,
0.0567950287426251,0.102031362436064,0.149040124071446,0.194408682186974,
0.240180552923466,0.287104886295882,0.297239095913451),.UNSPECIFIED.);
#549=B_SPLINE_CURVE_WITH_KNOTS('',3,(#47052,#47053,#47054,#47055,#47056,
#47057,#47058,#47059,#47060,#47061,#47062,#47063,#47064,#47065,#47066,#47067,
#47068,#47069,#47070,#47071,#47072,#47073,#47074,#47075,#47076,#47077,#47078,
#47079,#47080,#47081,#47082,#47083,#47084,#47085,#47086,#47087,#47088,#47089),
 .UNSPECIFIED.,.F.,.F.,(4,2,2,2,2,2,2,2,2,2,2,2,2,2,2,2,2,2,4),(10.6639140416271,
10.6650947082322,10.7119817347136,10.7580804193876,10.8029993273581,10.8503734008782,
10.8959427839672,10.9417692986129,10.9885470228329,11.0335695774763,11.0804254452447,
11.1265643813013,11.1713443335741,11.218213374293,11.2638454555082,11.3093155266254,
11.3561724820038,11.4012663166318,11.4063709592788),.UNSPECIFIED.);
#550=B_SPLINE_CURVE_WITH_KNOTS('',3,(#47090,#47091,#47092,#47093,#47094,
#47095,#47096,#47097,#47098,#47099,#47100,#47101,#47102,#47103,#47104,#47105,
#47106,#47107,#47108,#47109,#47110,#47111,#47112,#47113,#47114,#47115,#47116,
#47117,#47118,#47119,#47120,#47121,#47122,#47123,#47124,#47125),
 .UNSPECIFIED.,.F.,.F.,(4,2,2,2,2,2,2,2,2,2,2,2,2,2,2,2,2,4),(0.297239095913451,
0.331909892910397,0.378184802292447,0.425437891635738,0.470595177353486,
0.517516832751099,0.563142306369242,0.608840424213731,0.655808186318039,
0.700696994400866,0.746904510560702,0.793857785223327,0.838950917376441,
0.885800877455259,0.931807710447616,0.977451263235396,1.0249004194449,1.04102688126702),
 .UNSPECIFIED.);
#551=B_SPLINE_CURVE_WITH_KNOTS('',3,(#47130,#47131,#47132,#47133,#47134,
#47135,#47136,#47137,#47138,#47139,#47140,#47141,#47142,#47143,#47144,#47145,
#47146,#47147,#47148,#47149,#47150,#47151,#47152,#47153,#47154,#47155,#47156,
#47157,#47158,#47159,#47160,#47161,#47162,#47163,#47164,#47165),
 .UNSPECIFIED.,.F.,.F.,(4,2,2,2,2,2,2,2,2,2,2,2,2,2,2,2,2,4),(9.92229190963911,
9.92979763035616,9.97661529584815,10.0223875882399,10.0674947390005,10.1145130077351,
10.1597537191833,10.2061418234609,10.252546736718,10.2972921295131,10.3441264845473,
10.3900441574768,10.4350167599153,10.4821947166382,10.5275825848168,10.5736460837947,
10.6202215550774,10.6639140416271),.UNSPECIFIED.);
#552=B_SPLINE_CURVE_WITH_KNOTS('',3,(#47166,#47167,#47168,#47169,#47170,
#47171,#47172,#47173,#47174,#47175,#47176,#47177,#47178,#47179,#47180,#47181,
#47182,#47183,#47184,#47185,#47186,#47187,#47188,#47189,#47190,#47191,#47192,
#47193,#47194,#47195,#47196,#47197,#47198,#47199,#47200,#47201),
 .UNSPECIFIED.,.F.,.F.,(4,2,2,2,2,2,2,2,2,2,2,2,2,2,2,2,2,4),(1.04102688126702,
1.06994936982564,1.11612372964813,1.1631224274379,1.20807774239958,1.25473316609544,
1.30100208017051,1.34647258781685,1.39373457189629,1.43885942222957,1.48486151898195,
1.53181724470879,1.57666541818597,1.62315856887522,1.66977391100141,1.71510631020256,
1.76221822633913,1.78477649063309),.UNSPECIFIED.);
#553=B_SPLINE_CURVE_WITH_KNOTS('',3,(#47206,#47207,#47208,#47209,#47210,
#47211,#47212,#47213,#47214,#47215,#47216,#47217,#47218,#47219,#47220,#47221,
#47222,#47223,#47224,#47225,#47226,#47227,#47228,#47229,#47230,#47231,#47232,
#47233,#47234,#47235,#47236,#47237,#47238,#47239,#47240,#47241),
 .UNSPECIFIED.,.F.,.F.,(4,2,2,2,2,2,2,2,2,2,2,2,2,2,2,2,2,4),(9.18066291513125,
9.19415090290438,9.24103359345902,9.28663151390442,9.33221017295977,9.37902708695585,
9.42408423987445,9.47131574850735,9.51748383149001,9.56220744499011,9.60904188441202,
9.65470687463485,9.70002122809167,9.74691845045314,9.7920482780309,9.83883277613507,
9.88510096784626,9.92229190963911),.UNSPECIFIED.);
#554=B_SPLINE_CURVE_WITH_KNOTS('',3,(#47242,#47243,#47244,#47245,#47246,
#47247,#47248,#47249,#47250,#47251,#47252,#47253,#47254,#47255,#47256,#47257,
#47258,#47259,#47260,#47261,#47262,#47263,#47264,#47265,#47266,#47267,#47268,
#47269,#47270,#47271,#47272,#47273,#47274,#47275,#47276,#47277),
 .UNSPECIFIED.,.F.,.F.,(4,2,2,2,2,2,2,2,2,2,2,2,2,2,2,2,2,4),(1.78477649063309,
1.80749817211998,1.85336437928791,1.90031249731947,1.94513254024406,1.99149805378257,
2.03852655563362,2.08375775348993,2.13075894105089,2.17626379582903,2.22203292704428,
2.26900641402836,2.31387226672767,2.36014760821912,2.40710960481156,2.4522612783082,
2.49917450341029,2.52844772796884),.UNSPECIFIED.);
#555=B_SPLINE_CURVE_WITH_KNOTS('',3,(#47282,#47283,#47284,#47285,#47286,
#47287,#47288,#47289,#47290,#47291,#47292,#47293,#47294,#47295,#47296,#47297,
#47298,#47299,#47300,#47301,#47302,#47303,#47304,#47305,#47306,#47307,#47308,
#47309,#47310,#47311,#47312,#47313,#47314,#47315,#47316,#47317),
 .UNSPECIFIED.,.F.,.F.,(4,2,2,2,2,2,2,2,2,2,2,2,2,2,2,2,2,4),(8.43774741884447,
8.45752571504742,8.50469343833677,8.5500742626266,8.59632293033626,8.64288344885183,
8.68775172489367,8.73467282146192,8.78075134679685,8.82574058111398,8.87308972399771,
8.91863816774379,8.9646115037511,9.01136150601258,9.05635901694108,9.10322659194124,
9.14933383291891,9.18066291513125),.UNSPECIFIED.);
#556=B_SPLINE_CURVE_WITH_KNOTS('',3,(#47318,#47319,#47320,#47321,#47322,
#47323,#47324,#47325,#47326,#47327,#47328,#47329,#47330,#47331,#47332,#47333,
#47334,#47335,#47336,#47337,#47338,#47339,#47340,#47341,#47342,#47343,#47344,
#47345,#47346,#47347,#47348,#47349,#47350,#47351,#47352,#47353),
 .UNSPECIFIED.,.F.,.F.,(4,2,2,2,2,2,2,2,2,2,2,2,2,2,2,2,2,4),(2.52844772796884,
2.54500824613052,2.59070535491167,2.638214681952,2.68319585525036,2.72942299914916,
2.77639940937737,2.82139145839567,2.86809231879591,2.91413323574597,2.95963794063351,
3.00693966003781,3.05194785331698,3.09798282203751,3.14489438166212,3.18973360823921,
3.23625334475753,3.27195608346076),.UNSPECIFIED.);
#557=B_SPLINE_CURVE_WITH_KNOTS('',3,(#47358,#47359,#47360,#47361,#47362,
#47363,#47364,#47365,#47366,#47367,#47368,#47369,#47370,#47371,#47372,#47373,
#47374,#47375,#47376,#47377,#47378,#47379,#47380,#47381,#47382,#47383,#47384,
#47385,#47386,#47387,#47388,#47389,#47390,#47391,#47392,#47393),
 .UNSPECIFIED.,.F.,.F.,(4,2,2,2,2,2,2,2,2,2,2,2,2,2,2,2,2,4),(7.69539854103273,
7.72155321848494,7.7684724835817,7.8136255677965,7.86065234102687,7.90693393580434,
7.9516908438395,7.99857209635814,8.04435399500581,8.0895977391991,8.13662142723008,
8.18186980363593,8.22847577989916,8.27487933356857,8.31965265394499,8.3665363700462,
8.41244823537304,8.43774741884447),.UNSPECIFIED.);
#558=B_SPLINE_CURVE_WITH_KNOTS('',3,(#47394,#47395,#47396,#47397,#47398,
#47399,#47400,#47401,#47402,#47403,#47404,#47405,#47406,#47407,#47408,#47409,
#47410,#47411,#47412,#47413,#47414,#47415,#47416,#47417,#47418,#47419,#47420,
#47421,#47422,#47423,#47424,#47425,#47426,#47427,#47428,#47429),
 .UNSPECIFIED.,.F.,.F.,(4,2,2,2,2,2,2,2,2,2,2,2,2,2,2,2,2,4),(3.27195608346076,
3.282592657188,3.3279388134706,3.37506873495414,3.42018650623354,3.46606423055494,
3.51294786154499,3.55771304574351,3.60408475803478,3.65080015723448,3.69602345065255,
3.74301955034469,3.78832280212397,3.83408062999374,3.88097059164275,3.92573930458549,
3.97199874621623,4.01433671221151),.UNSPECIFIED.);
#559=B_SPLINE_CURVE_WITH_KNOTS('',3,(#47434,#47435,#47436,#47437,#47438,
#47439,#47440,#47441,#47442,#47443,#47444,#47445,#47446,#47447,#47448,#47449,
#47450,#47451,#47452,#47453,#47454,#47455,#47456,#47457,#47458,#47459,#47460,
#47461,#47462,#47463,#47464,#47465,#47466,#47467,#47468,#47469),
 .UNSPECIFIED.,.F.,.F.,(4,2,2,2,2,2,2,2,2,2,2,2,2,2,2,2,2,4),(6.95232021216865,
6.98520940682934,7.03183776179107,7.07676034379647,7.12368218105456,7.16983534809316,
7.21477539351345,7.26220706699282,7.30783067803266,7.3536506056871,7.40048621914621,
7.44556384932218,7.49246290359126,7.5386603688324,7.5834734101616,7.63038481462985,
7.67607584920904,7.69539854103273),.UNSPECIFIED.);
#560=B_SPLINE_CURVE_WITH_KNOTS('',3,(#47470,#47471,#47472,#47473,#47474,
#47475,#47476,#47477,#47478,#47479,#47480,#47481,#47482,#47483,#47484,#47485,
#47486,#47487,#47488,#47489,#47490,#47491,#47492,#47493,#47494,#47495,#47496,
#47497,#47498,#47499,#47500,#47501,#47502,#47503,#47504,#47505,#47506,#47507),
 .UNSPECIFIED.,.F.,.F.,(4,2,2,2,2,2,2,2,2,2,2,2,2,2,2,2,2,2,4),(4.01433671221151,
4.01914805413287,4.06428615761616,4.11118860567824,4.15674023560365,4.20241784028498,
4.24934623552864,4.29418852097545,4.34037422725447,4.38728888642649,4.43235854054739,
4.47918474875809,4.52510312300865,4.57072126834585,4.61814520147569,4.66313508164065,
4.70928335610809,4.75623501458851,4.75775515205278),.UNSPECIFIED.);
#561=B_SPLINE_CURVE_WITH_KNOTS('',3,(#47512,#47513,#47514,#47515,#47516,
#47517,#47518,#47519,#47520,#47521,#47522,#47523,#47524,#47525,#47526,#47527,
#47528,#47529,#47530,#47531,#47532,#47533,#47534,#47535,#47536,#47537,#47538,
#47539,#47540,#47541,#47542,#47543,#47544,#47545,#47546,#47547),
 .UNSPECIFIED.,.F.,.F.,(4,2,2,2,2,2,2,2,2,2,2,2,2,2,2,2,2,4),(6.21040332353066,
6.24996363653887,6.29627383230895,6.34099487094829,6.38783578085351,6.43365110481032,
6.47875379116074,6.52581793545371,6.57110181115006,6.61745562645394,6.66390817507345,
6.70869049645745,6.75555365022892,6.80152025981645,6.84650073651534,6.89373059013836,
6.93916728504739,6.95232021216865),.UNSPECIFIED.);
#562=B_SPLINE_CURVE_WITH_KNOTS('',3,(#47548,#47549,#47550,#47551,#47552,
#47553,#47554,#47555,#47556,#47557,#47558,#47559,#47560,#47561,#47562,#47563,
#47564,#47565,#47566,#47567,#47568,#47569,#47570,#47571,#47572,#47573,#47574,
#47575,#47576,#47577,#47578,#47579,#47580,#47581,#47582,#47583),
 .UNSPECIFIED.,.F.,.F.,(4,2,2,2,2,2,2,2,2,2,2,2,2,2,2,2,2,4),(4.75775515205278,
4.80115954720664,4.84778657251392,4.89395239727177,4.93939241272434,4.98662379950037,
5.03167653106206,5.07764728797061,5.12455025523998,5.16935540816532,5.21581518399032,
5.26231483989851,5.30761133212679,5.3546868913279,5.39988274125814,5.44571192890845,
5.4926019451231,5.50046293121957),.UNSPECIFIED.);
#563=B_SPLINE_CURVE_WITH_KNOTS('',3,(#47588,#47589,#47590,#47591,#47592,
#47593,#47594,#47595,#47596,#47597,#47598,#47599,#47600,#47601,#47602,#47603,
#47604,#47605,#47606,#47607,#47608,#47609,#47610,#47611,#47612,#47613,#47614,
#47615,#47616,#47617,#47618,#47619,#47620,#47621,#47622,#47623,#47624,#47625),
 .UNSPECIFIED.,.F.,.F.,(4,2,2,2,2,2,2,2,2,2,2,2,2,2,2,2,2,2,4),(5.46823516997428,
5.46924523189168,5.51421339539498,5.56093347890932,5.60681683684292,5.65233399971011,
5.69965169327359,5.74457803521868,5.79062455915303,5.83749440380915,5.8823256252987,
5.92852964558371,5.97326608757821,6.0201185992117,6.06582034727076,6.11111957359516,
6.15805631170891,6.20322334029363,6.21040332353066),.UNSPECIFIED.);
#564=B_SPLINE_CURVE_WITH_KNOTS('',3,(#47626,#47627,#47628,#47629,#47630,
#47631,#47632,#47633,#47634,#47635,#47636,#47637,#47638,#47639,#47640,#47641,
#47642,#47643,#47644,#47645,#47646,#47647,#47648,#47649,#47650,#47651,#47652,
#47653,#47654,#47655,#47656,#47657,#47658,#47659,#47660,#47661),
 .UNSPECIFIED.,.F.,.F.,(4,2,2,2,2,2,2,2,2,2,2,2,2,2,2,2,2,4),(5.50046293121957,
5.53736683161235,5.58369353071173,5.6305968047525,5.67578632165126,5.72274499816332,
5.76815552869047,5.81388154564766,5.86079188348587,5.90559155055078,5.95219446597211,
5.9970962044243,6.04402631060266,6.09015041966504,6.13512165037609,6.18252051520117,
6.22811471720219,6.24337196603104),.UNSPECIFIED.);
#565=B_SPLINE_CURVE_WITH_KNOTS('',3,(#47666,#47667,#47668,#47669,#47670,
#47671,#47672,#47673,#47674,#47675,#47676,#47677,#47678,#47679,#47680,#47681,
#47682,#47683,#47684,#47685,#47686,#47687,#47688,#47689,#47690,#47691,#47692,
#47693,#47694,#47695,#47696,#47697,#47698,#47699,#47700,#47701),
 .UNSPECIFIED.,.F.,.F.,(4,2,2,2,2,2,2,2,2,2,2,2,2,2,2,2,2,4),(4.72706962089855,
4.73421323881064,4.77932354628057,4.82620128907514,4.87144673700927,4.91709114393615,
4.96388604536429,5.0085677160079,5.05471383888917,5.10184091457902,5.14687278115198,
5.19366407264861,5.2391662347845,5.28473750147929,5.33157602074619,5.37634188682691,
5.42242120372861,5.46823516997428),.UNSPECIFIED.);
#566=B_SPLINE_CURVE_WITH_KNOTS('',3,(#47702,#47703,#47704,#47705,#47706,
#47707,#47708,#47709,#47710,#47711,#47712,#47713,#47714,#47715,#47716,#47717,
#47718,#47719,#47720,#47721,#47722,#47723,#47724,#47725,#47726,#47727,#47728,
#47729,#47730,#47731,#47732,#47733,#47734,#47735,#47736,#47737),
 .UNSPECIFIED.,.F.,.F.,(4,2,2,2,2,2,2,2,2,2,2,2,2,2,2,2,2,4),(6.24337196603104,
6.27401821929249,6.32081950996656,6.36586527339041,6.4127571572649,6.4589180548967,
6.50373993867417,6.55064566532991,6.59629857778885,6.64183340160009,6.68871022418118,
6.73382376991178,6.78095970840426,6.82719337080345,6.87194020815821,6.91880678990272,
6.9645389314372,6.98590521985964),.UNSPECIFIED.);
#567=B_SPLINE_CURVE_WITH_KNOTS('',3,(#47742,#47743,#47744,#47745,#47746,
#47747,#47748,#47749,#47750,#47751,#47752,#47753,#47754,#47755,#47756,#47757,
#47758,#47759,#47760,#47761,#47762,#47763,#47764,#47765,#47766,#47767,#47768,
#47769,#47770,#47771,#47772,#47773,#47774,#47775,#47776,#47777),
 .UNSPECIFIED.,.F.,.F.,(4,2,2,2,2,2,2,2,2,2,2,2,2,2,2,2,2,4),(3.98607357350402,
3.99918191936072,4.04456087825365,4.09173064872777,4.13665634482318,4.18256457182781,
4.22936946042104,4.27409551151173,4.32048917025343,4.36678906526987,4.41201572517385,
4.45902034323992,4.50406884281734,4.54982631660765,4.5966093208145,4.64127491262894,
4.68752672363699,4.72706962089855),.UNSPECIFIED.);
#568=B_SPLINE_CURVE_WITH_KNOTS('',3,(#47778,#47779,#47780,#47781,#47782,
#47783,#47784,#47785,#47786,#47787,#47788,#47789,#47790,#47791,#47792,#47793,
#47794,#47795,#47796,#47797,#47798,#47799,#47800,#47801,#47802,#47803,#47804,
#47805,#47806,#47807,#47808,#47809,#47810,#47811,#47812,#47813),
 .UNSPECIFIED.,.F.,.F.,(4,2,2,2,2,2,2,2,2,2,2,2,2,2,2,2,2,4),(6.98590521985964,
7.00982424920481,7.05679371040423,7.10199149720955,7.1486926619025,7.19503766539008,
7.23977922568632,7.28663870486131,7.3324897765694,7.37758804450172,7.42469034180235,
7.47001006811599,7.51633373613469,7.56282588238178,7.60763958801924,7.65452614947266,
7.70053353816524,7.7280430341459),.UNSPECIFIED.);
#569=B_SPLINE_CURVE_WITH_KNOTS('',3,(#47818,#47819,#47820,#47821,#47822,
#47823,#47824,#47825,#47826,#47827,#47828,#47829,#47830,#47831,#47832,#47833,
#47834,#47835,#47836,#47837,#47838,#47839,#47840,#47841,#47842,#47843,#47844,
#47845,#47846,#47847,#47848,#47849,#47850,#47851,#47852,#47853),
 .UNSPECIFIED.,.F.,.F.,(4,2,2,2,2,2,2,2,2,2,2,2,2,2,2,2,2,4),(3.24392841407934,
3.26320118186788,3.30883357721227,3.35568585153,3.40044282038451,3.44658106056088,
3.49342094952175,3.53844090839015,3.58521656152064,3.63098154698795,3.67654687597848,
3.72391788461319,3.76880240701922,3.81489663770949,3.86175977891139,3.9066251798824,
3.95319412178152,3.98607357350402),.UNSPECIFIED.);
#570=B_SPLINE_CURVE_WITH_KNOTS('',3,(#47854,#47855,#47856,#47857,#47858,
#47859,#47860,#47861,#47862,#47863,#47864,#47865,#47866,#47867,#47868,#47869,
#47870,#47871,#47872,#47873,#47874,#47875,#47876,#47877,#47878,#47879,#47880,
#47881,#47882,#47883,#47884,#47885,#47886,#47887,#47888,#47889),
 .UNSPECIFIED.,.F.,.F.,(4,2,2,2,2,2,2,2,2,2,2,2,2,2,2,2,2,4),(7.7280430341459,
7.74552040966934,7.79279355251667,7.83827093210572,7.8842943505838,7.93096677709508,
7.97593141803747,8.02288189886512,8.06908057135937,8.1140384707018,8.16151829876598,
8.20718720882142,8.25300132576618,8.2998852910774,8.34500889959013,8.39194375347128,
8.43819004733793,8.47155481750159),.UNSPECIFIED.);
#571=B_SPLINE_CURVE_WITH_KNOTS('',3,(#47894,#47895,#47896,#47897,#47898,
#47899,#47900,#47901,#47902,#47903,#47904,#47905,#47906,#47907,#47908,#47909,
#47910,#47911,#47912,#47913,#47914,#47915,#47916,#47917,#47918,#47919,#47920,
#47921,#47922,#47923,#47924,#47925,#47926,#47927,#47928,#47929),
 .UNSPECIFIED.,.F.,.F.,(4,2,2,2,2,2,2,2,2,2,2,2,2,2,2,2,2,4),(2.50252141868207,
2.52776021043164,2.57361244595458,2.62043647340302,2.6651524611521,2.71149584066551,
2.75804622814296,2.80323613082756,2.85019899727244,2.89538716038286,2.941109939166,
2.98793181216642,3.03263210415199,3.07885401093438,3.12582513877793,3.17092021696239,
3.21777916276462,3.24392841407934),.UNSPECIFIED.);
#572=B_SPLINE_CURVE_WITH_KNOTS('',3,(#47930,#47931,#47932,#47933,#47934,
#47935,#47936,#47937,#47938,#47939,#47940,#47941,#47942,#47943,#47944,#47945,
#47946,#47947,#47948,#47949,#47950,#47951,#47952,#47953,#47954,#47955,#47956,
#47957,#47958,#47959,#47960,#47961,#47962,#47963,#47964,#47965),
 .UNSPECIFIED.,.F.,.F.,(4,2,2,2,2,2,2,2,2,2,2,2,2,2,2,2,2,4),(8.47155481750159,
8.48303098251424,8.52997744983096,8.57571769446406,8.62120106342097,8.66817233854124,
8.71337485643584,8.76038502225125,8.80672058392342,8.8515142195167,8.89843463378869,
8.94427102223284,8.98952825218029,9.0366093049851,9.0819121341257,9.12850816287234,
9.17497049631086,9.21453814874152),.UNSPECIFIED.);
#573=B_SPLINE_CURVE_WITH_KNOTS('',3,(#47970,#47971,#47972,#47973,#47974,
#47975,#47976,#47977,#47978,#47979,#47980,#47981,#47982,#47983,#47984,#47985,
#47986,#47987,#47988,#47989,#47990,#47991,#47992,#47993,#47994,#47995,#47996,
#47997,#47998,#47999,#48000,#48001,#48002,#48003,#48004,#48005),
 .UNSPECIFIED.,.F.,.F.,(4,2,2,2,2,2,2,2,2,2,2,2,2,2,2,2,2,4),(1.76055864693328,
1.79182126771535,1.83786803837673,1.88467512490527,1.92961375851794,1.97630255407359,
2.0222196260872,2.0677085751512,2.11499580318964,2.15992835930496,2.20594672076016,
2.2528077518393,2.29761785291437,2.34411769224053,2.39031055560415,2.43563240933956,
2.48273877805656,2.50252141868207),.UNSPECIFIED.);
#574=B_SPLINE_CURVE_WITH_KNOTS('',3,(#48006,#48007,#48008,#48009,#48010,
#48011,#48012,#48013,#48014,#48015,#48016,#48017,#48018,#48019,#48020,#48021,
#48022,#48023,#48024,#48025,#48026,#48027,#48028,#48029,#48030,#48031,#48032,
#48033,#48034,#48035,#48036,#48037,#48038,#48039,#48040,#48041,#48042,#48043),
 .UNSPECIFIED.,.F.,.F.,(4,2,2,2,2,2,2,2,2,2,2,2,2,2,2,2,2,2,4),(9.21453814874152,
9.21979055026988,9.26671782254207,9.31268919604266,9.35778979281078,9.40501998742909,
9.45046005687993,9.4967081920225,9.54333197258473,9.58825736766484,9.63522678342864,
9.68136954756796,9.72639248238748,9.77380894901864,9.81942121560885,9.86540543979499,
9.91222295415185,9.95728494289229,9.95826087397132),.UNSPECIFIED.);
#575=B_SPLINE_CURVE_WITH_KNOTS('',3,(#48048,#48049,#48050,#48051,#48052,
#48053,#48054,#48055,#48056,#48057,#48058,#48059,#48060,#48061,#48062,#48063,
#48064,#48065,#48066,#48067,#48068,#48069,#48070,#48071,#48072,#48073,#48074,
#48075,#48076,#48077,#48078,#48079,#48080,#48081,#48082,#48083),
 .UNSPECIFIED.,.F.,.F.,(4,2,2,2,2,2,2,2,2,2,2,2,2,2,2,2,2,4),(1.0198908055646,
1.05700253667009,1.10320928671584,1.14993696120769,1.19500709107715,1.24184222630525,
1.28709985760173,1.33270449750631,1.379478231302,1.42414417613706,1.4702513175641,
1.51742579982366,1.56242372917786,1.6091790650006,1.65470112473219,1.70023918105991,
1.74706140067451,1.76055864693328),.UNSPECIFIED.);
#576=B_SPLINE_CURVE_WITH_KNOTS('',3,(#48084,#48085,#48086,#48087,#48088,
#48089,#48090,#48091,#48092,#48093,#48094,#48095,#48096,#48097,#48098,#48099,
#48100,#48101,#48102,#48103,#48104,#48105,#48106,#48107,#48108,#48109,#48110,
#48111,#48112,#48113,#48114,#48115,#48116,#48117,#48118,#48119),
 .UNSPECIFIED.,.F.,.F.,(4,2,2,2,2,2,2,2,2,2,2,2,2,2,2,2,2,4),(9.95826087397132,
10.0042077855434,10.0503830644129,10.0952441977488,10.1421816171258,10.1878477047942,
10.2334488002604,10.2803373027871,10.3254627794739,10.3726944829175,10.4189361962616,
10.4637121618962,10.5106054781006,10.5563443378488,10.60168753486,10.6486621415555,
10.693865727852,10.7009872972758),.UNSPECIFIED.);
#577=B_SPLINE_CURVE_WITH_KNOTS('',3,(#48124,#48125,#48126,#48127,#48128,
#48129,#48130,#48131,#48132,#48133,#48134,#48135,#48136,#48137,#48138,#48139,
#48140,#48141,#48142,#48143,#48144,#48145,#48146,#48147,#48148,#48149,#48150,
#48151,#48152,#48153,#48154,#48155,#48156,#48157,#48158,#48159),
 .UNSPECIFIED.,.F.,.F.,(4,2,2,2,2,2,2,2,2,2,2,2,2,2,2,2,2,4),(0.279240333252414,
0.322844270949173,0.369357241132825,0.415363471402469,0.46069060038965,
0.507805353095372,0.55272028410885,0.598576537627569,0.645349536044773,
0.69003577120083,0.736378722628649,0.782709920293503,0.827890427170548,
0.874846064622692,0.919896118269451,0.965607538883625,1.01236420598534,
1.0198908055646),.UNSPECIFIED.);
#578=B_SPLINE_CURVE_WITH_KNOTS('',3,(#48160,#48161,#48162,#48163,#48164,
#48165,#48166,#48167,#48168,#48169,#48170,#48171,#48172,#48173,#48174,#48175,
#48176,#48177,#48178,#48179,#48180,#48181,#48182,#48183,#48184,#48185,#48186,
#48187,#48188,#48189,#48190,#48191,#48192,#48193,#48194,#48195),
 .UNSPECIFIED.,.F.,.F.,(4,2,2,2,2,2,2,2,2,2,2,2,2,2,2,2,2,4),(10.7009872972758,
10.7406554053031,10.7870025479307,10.8317614667191,10.8786424437052,10.9244941101883,
10.9696390710423,11.0167403153779,11.0620600256883,11.1084614451944,11.154950288831,
11.1997687866196,11.2466712469847,11.2926735167475,11.337694414731,11.3849606827389,
11.4304325644015,11.4435301988629),.UNSPECIFIED.);
#579=B_SPLINE_CURVE_WITH_KNOTS('',3,(#48198,#48199,#48200,#48201,#48202,
#48203,#48204,#48205,#48206,#48207,#48208,#48209,#48210,#48211,#48212,#48213,
#48214,#48215,#48216,#48217),.UNSPECIFIED.,.F.,.F.,(4,2,2,2,2,2,2,2,2,4),
(11.4435301988629,11.4765201718647,11.5231842534289,11.5681413990089,11.6151017516702,
11.6612899790245,11.7062685498772,11.753736029675,11.7850799770424,11.815365841815),
 .UNSPECIFIED.);
#580=B_SPLINE_CURVE_WITH_KNOTS('',3,(#48220,#48221,#48222,#48223,#48224,
#48225,#48226,#48227,#48228,#48229,#48230,#48231,#48232,#48233,#48234,#48235,
#48236,#48237),.UNSPECIFIED.,.F.,.F.,(4,2,2,2,2,2,2,2,4),(9.99999983579279E-7,
0.0240245188069277,0.0474912529693272,0.0929991717620865,0.140309272354935,
0.185169608656008,0.231206138227982,0.278031208662583,0.279240333252414),
 .UNSPECIFIED.);
#581=B_SPLINE_CURVE_WITH_KNOTS('',3,(#48240,#48241,#48242,#48243,#48244,
#48245,#48246,#48247,#48248,#48249,#48250,#48251,#48252,#48253,#48254,#48255,
#48256,#48257,#48258,#48259,#48260,#48261,#48262,#48263,#48264,#48265,#48266,
#48267,#48268,#48269,#48270,#48271),.UNSPECIFIED.,.F.,.F.,(4,2,2,2,2,2,
2,2,2,2,2,2,2,2,2,4),(-0.829142789718882,-0.77306457962365,-0.714223388829787,
-0.65718540765388,-0.597470281301096,-0.539279665144528,-0.481455062329678,
-0.4216816411846,-0.364162666057075,-0.304420722553672,-0.245430580868346,
-0.188433357111664,-0.128737077916135,-0.0703952695266761,-0.0354402198856821,
-9.99999999917733E-7),.UNSPECIFIED.);
#582=B_SPLINE_CURVE_WITH_KNOTS('',3,(#48274,#48275,#48276,#48277,#48278,
#48279,#48280,#48281,#48282,#48283,#48284,#48285,#48286,#48287,#48288,#48289,
#48290,#48291,#48292,#48293,#48294,#48295,#48296,#48297,#48298,#48299,#48300,
#48301,#48302,#48303),.UNSPECIFIED.,.F.,.F.,(4,2,2,2,2,2,2,2,2,2,2,2,2,
2,4),(-14.3815521744247,-14.3490819882549,-14.3173656294494,-14.2606308082457,
-14.2020989293593,-14.1427123139841,-14.0856330557203,-14.026327836904,
-13.9683949339112,-13.9106424935611,-13.8505851839565,-13.7937266961226,
-13.7353019168941,-13.6759104215302,-13.6754849562843),.UNSPECIFIED.);
#583=B_SPLINE_CURVE_WITH_KNOTS('',3,(#48322,#48323,#48324,#48325,#48326,
#48327,#48328,#48329,#48330,#48331,#48332,#48333,#48334,#48335,#48336,#48337,
#48338,#48339,#48340,#48341,#48342,#48343,#48344,#48345,#48346,#48347),
 .UNSPECIFIED.,.F.,.F.,(4,2,2,2,2,2,2,2,2,2,2,2,4),(0.480400932349348,0.485329977931986,
0.530683146887141,0.579550101290595,0.64089353991474,0.720505764207005,
0.804785042766715,0.896510611485352,0.997812688736786,1.10248963403809,
1.17665715785729,1.21374936533913,1.25141712065186),.UNSPECIFIED.);
#584=B_SPLINE_CURVE_WITH_KNOTS('',3,(#48351,#48352,#48353,#48354,#48355,
#48356,#48357,#48358,#48359,#48360,#48361,#48362,#48363,#48364,#48365,#48366),
 .UNSPECIFIED.,.F.,.F.,(4,2,2,2,2,2,2,4),(0.,0.0362708955824572,0.085273156200874,
0.169912753697905,0.248908834870632,0.337286385899651,0.42390178686825,
0.480400932349348),.UNSPECIFIED.);
#585=B_SPLINE_CURVE_WITH_KNOTS('',3,(#48367,#48368,#48369,#48370,#48371,
#48372,#48373,#48374,#48375,#48376,#48377,#48378),.UNSPECIFIED.,.F.,.F.,
(4,2,2,2,2,4),(-0.173020928061641,-0.143983119462096,-0.113362764878225,
-0.0824055056388063,-0.0457488593866804,-9.99999131029439E-7),
 .UNSPECIFIED.);
#586=B_SPLINE_CURVE_WITH_KNOTS('',3,(#48778,#48779,#48780,#48781,#48782,
#48783,#48784,#48785,#48786,#48787,#48788,#48789,#48790,#48791,#48792,#48793),
 .UNSPECIFIED.,.F.,.F.,(4,2,2,2,2,2,2,4),(-0.193591868481661,-0.164589722295103,
-0.136229103543845,-0.109019089206068,-0.086513074650219,-0.0622509824423357,
-0.0393944302207767,-1.00000006228451E-6),.UNSPECIFIED.);
#587=B_SPLINE_CURVE_WITH_KNOTS('',3,(#49184,#49185,#49186,#49187,#49188,
#49189,#49190,#49191,#49192,#49193,#49194,#49195,#49196,#49197,#49198,#49199,
#49200,#49201),.UNSPECIFIED.,.F.,.F.,(4,2,2,2,2,2,2,2,4),(-0.298889159334175,
-0.248475417408008,-0.215742180818938,-0.174449183868093,-0.150666431566684,
-0.103667997862826,-0.0537346078292575,-0.0261328721932875,-1.00000013070201E-6),
 .UNSPECIFIED.);
#588=B_SPLINE_CURVE_WITH_KNOTS('',3,(#49306,#49307,#49308,#49309,#49310,
#49311,#49312,#49313,#49314,#49315,#49316,#49317,#49318,#49319,#49320,#49321,
#49322,#49323,#49324,#49325,#49326,#49327,#49328,#49329,#49330),
 .UNSPECIFIED.,.F.,.F.,(4,3,3,3,3,3,3,3,4),(0.,0.160731090032336,0.25,0.407767129262868,
0.5,0.657767129262875,0.75,0.910731090032353,1.),.UNSPECIFIED.);
#589=B_SPLINE_CURVE_WITH_KNOTS('',3,(#49333,#49334,#49335,#49336,#49337,
#49338,#49339),.UNSPECIFIED.,.F.,.F.,(4,1,1,1,4),(0.,0.25,0.5,0.75,0.999999761822425),
 .UNSPECIFIED.);
#590=B_SPLINE_CURVE_WITH_KNOTS('',3,(#49345,#49346,#49347,#49348,#49349,
#49350,#49351,#49352,#49353,#49354,#49355,#49356,#49357,#49358,#49359,#49360,
#49361,#49362,#49363,#49364,#49365,#49366,#49367,#49368,#49369,#49370,#49371,
#49372,#49373,#49374,#49375,#49376,#49377,#49378,#49379,#49380,#49381,#49382,
#49383,#49384),.UNSPECIFIED.,.F.,.F.,(4,3,3,3,3,3,3,3,3,3,3,3,3,4),(0.235508041128149,
0.25,0.331910603091831,0.375,0.456895223609452,0.5,0.581895223609489,0.625,
0.706910603091898,0.75,0.831608731491742,0.875,0.958140783942944,0.999999441342508),
 .UNSPECIFIED.);
#591=B_SPLINE_CURVE_WITH_KNOTS('',3,(#49386,#49387,#49388,#49389),
 .UNSPECIFIED.,.F.,.F.,(4,4),(0.,0.987035809516257),.UNSPECIFIED.);
#592=B_SPLINE_CURVE_WITH_KNOTS('',3,(#49392,#49393,#49394,#49395,#49396,
#49397,#49398,#49399,#49400,#49401,#49402,#49403,#49404,#49405,#49406,#49407,
#49408,#49409,#49410,#49411,#49412,#49413,#49414,#49415),.UNSPECIFIED.,
 .F.,.F.,(4,2,2,2,2,2,2,2,2,2,2,4),(0.,0.100888900202487,0.125,0.22459286542628,
0.25,0.349878675008739,0.375,0.474842812735284,0.5,0.599842812735286,0.625,
0.715961029345133),.UNSPECIFIED.);
#593=B_SPLINE_CURVE_WITH_KNOTS('',3,(#49418,#49419,#49420,#49421,#49422,
#49423,#49424,#49425,#49426,#49427,#49428,#49429,#49430,#49431,#49432,#49433),
 .UNSPECIFIED.,.F.,.F.,(4,3,3,3,3,4),(0.715961029345133,0.75,0.849592865426306,
0.875,0.975888900203264,1.),.UNSPECIFIED.);
#594=B_SPLINE_CURVE_WITH_KNOTS('',3,(#49435,#49436,#49437,#49438,#49439,
#49440,#49441,#49442,#49443,#49444,#49445,#49446,#49447,#49448,#49449,#49450,
#49451,#49452,#49453,#49454,#49455,#49456,#49457,#49458,#49459),
 .UNSPECIFIED.,.F.,.F.,(4,3,3,3,3,3,3,3,4),(1.51276851349366E-6,0.156898311431348,
0.25,0.403657035544793,0.5,0.653657035544841,0.75,0.906896809192571,1.),
 .UNSPECIFIED.);
#595=B_SPLINE_CURVE_WITH_KNOTS('',3,(#49463,#49464,#49465,#49466,#49467,
#49468,#49469,#49470,#49471,#49472,#49473,#49474,#49475,#49476,#49477,#49478,
#49479,#49480,#49481),.UNSPECIFIED.,.F.,.F.,(4,3,3,3,3,3,4),(0.,0.25,0.491380882785342,
0.5,0.75,0.982966826876961,1.),.UNSPECIFIED.);
#596=B_SPLINE_CURVE_WITH_KNOTS('',3,(#49482,#49483,#49484,#49485,#49486,
#49487,#49488,#49489,#49490,#49491),.UNSPECIFIED.,.F.,.F.,(4,2,2,2,4),(0.,
0.0831407875458867,0.125,0.206497666001318,0.235508041094431),
 .UNSPECIFIED.);
#597=B_SPLINE_CURVE_WITH_KNOTS('',3,(#49494,#49495,#49496,#49497,#49498,
#49499,#49500,#49501,#49502,#49503,#49504,#49505,#49506,#49507,#49508,#49509,
#49510,#49511,#49512,#49513,#49514,#49515,#49516,#49517,#49518,#49519,#49520,
#49521,#49522,#49523,#49524,#49525,#49526,#49527,#49528,#49529,#49530,#49531,
#49532,#49533,#49534,#49535,#49536,#49537,#49538,#49539,#49540,#49541,#49542,
#49543,#49544,#49545,#49546,#49547,#49548,#49549,#49550,#49551,#49552,#49553,
#49554,#49555,#49556,#49557,#49558,#49559,#49560,#49561,#49562,#49563,#49564,
#49565,#49566,#49567,#49568,#49569,#49570,#49571,#49572,#49573,#49574,#49575,
#49576,#49577,#49578,#49579,#49580,#49581,#49582,#49583,#49584,#49585,#49586,
#49587,#49588,#49589),.UNSPECIFIED.,.F.,.F.,(4,2,2,2,2,2,2,2,2,2,2,2,2,
2,2,2,2,2,2,2,2,2,2,2,2,2,2,2,2,2,2,2,2,2,2,2,2,2,2,2,2,2,2,2,2,2,2,4),
(0.000203483817492821,0.0274848173325521,0.0563713830966491,0.167677917602274,
0.208184918082086,0.239301283250976,0.272826962459817,0.365270654699785,
0.43178988571008,0.47678039384355,0.587559073236576,0.632135152418474,0.664943612441571,
0.694797097900161,0.799548600392106,0.862971031190955,0.907614126172384,
0.988296557870209,1.06800029357004,1.09774395705088,1.13107244772413,1.22338481693792,
1.27276714107893,1.31911661255326,1.37385993664007,1.44604280082289,1.50302473070022,
1.53055325884595,1.56982870717352,1.63222593298961,1.71178156213431,1.75641486537916,
1.81980681943984,1.92449539617685,1.95434391906131,1.98714005868704,2.03169939876711,
2.14252612578957,2.18750485709249,2.25402546067906,2.3464077625176,2.37990009772018,
2.41102584148667,2.45156693199543,2.56907534347477,2.61465490234983,2.68897499185438,
2.74712781989908),.UNSPECIFIED.);
#598=B_SPLINE_CURVE_WITH_KNOTS('',3,(#49592,#49593,#49594,#49595,#49596,
#49597,#49598,#49599,#49600,#49601,#49602),.UNSPECIFIED.,.F.,.F.,(4,1,1,
1,1,1,1,1,4),(0.,0.125,0.25,0.375,0.5,0.625,0.75,0.875,0.999999067031556),
 .UNSPECIFIED.);
#599=B_SPLINE_CURVE_WITH_KNOTS('',3,(#49615,#49616,#49617,#49618,#49619,
#49620,#49621,#49622,#49623,#49624,#49625,#49626,#49627,#49628,#49629,#49630,
#49631,#49632,#49633,#49634,#49635,#49636,#49637,#49638,#49639,#49640,#49641,
#49642,#49643,#49644,#49645,#49646,#49647,#49648,#49649,#49650,#49651,#49652,
#49653,#49654,#49655,#49656,#49657,#49658,#49659,#49660,#49661,#49662,#49663,
#49664,#49665,#49666,#49667,#49668,#49669,#49670,#49671,#49672,#49673,#49674,
#49675,#49676,#49677,#49678,#49679,#49680,#49681,#49682,#49683,#49684,#49685,
#49686,#49687,#49688,#49689,#49690,#49691,#49692,#49693,#49694,#49695,#49696,
#49697,#49698,#49699,#49700,#49701,#49702,#49703,#49704,#49705),
 .UNSPECIFIED.,.F.,.F.,(4,3,3,3,3,3,3,3,3,3,3,3,3,3,3,3,3,3,3,3,3,3,3,3,
3,3,3,3,3,3,4),(0.,0.0549095480248197,0.0909168947914259,0.127664846372719,
0.147588217015191,0.152802982426264,0.157890055006788,0.195093310789768,
0.232935081254819,0.292943797457197,0.305066964469618,0.310416184503556,
0.349172960287603,0.387949178487593,0.446438776652271,0.460993647480443,
0.469743525078789,0.474867539044195,0.512454117005302,0.550939413816203,
0.624355350952517,0.633225532922949,0.64024307789027,0.680180338798595,
0.720316379107474,0.73809145220851,0.748199996374111,0.754956026360989,
0.795541316014259,0.835496820076563,0.862516963915765),.UNSPECIFIED.);
#600=B_SPLINE_CURVE_WITH_KNOTS('',3,(#49706,#49707,#49708,#49709,#49710,
#49711,#49712,#49713,#49714,#49715,#49716,#49717,#49718,#49719,#49720,#49721,
#49722,#49723,#49724,#49725,#49726,#49727,#49728,#49729,#49730,#49731,#49732,
#49733,#49734,#49735,#49736,#49737,#49738,#49739,#49740,#49741,#49742,#49743,
#49744,#49745,#49746,#49747,#49748,#49749,#49750,#49751,#49752,#49753,#49754,
#49755,#49756,#49757,#49758,#49759,#49760,#49761,#49762,#49763,#49764,#49765,
#49766,#49767,#49768,#49769,#49770,#49771,#49772),.UNSPECIFIED.,.F.,.F.,
(4,3,3,3,3,3,3,3,3,3,3,3,3,3,3,3,3,3,3,3,3,3,4),(0.,0.0399225644477167,
0.0623885722514162,0.164012510354697,0.170043304514999,0.174785078605868,
0.294020040644772,0.316832921701425,0.3295965682445,0.337876395007978,0.382194010439746,
0.420601788797671,0.476523089097994,0.50063461453704,0.506312621506711,
0.652610410209141,0.659762241707176,0.665735072710524,0.763244547674934,
0.769629684943624,0.806337248425914,0.842085556810208,0.865008878888598),
 .UNSPECIFIED.);
#601=B_SPLINE_CURVE_WITH_KNOTS('',3,(#49773,#49774,#49775,#49776,#49777,
#49778),.UNSPECIFIED.,.F.,.F.,(4,2,4),(3.98711970495987E-6,0.000952908437083531,
0.00170790873623591),.UNSPECIFIED.);
#602=B_SPLINE_CURVE_WITH_KNOTS('',3,(#49790,#49791,#49792,#49793,#49794,
#49795,#49796,#49797,#49798,#49799,#49800,#49801,#49802,#49803,#49804,#49805,
#49806,#49807,#49808,#49809,#49810,#49811,#49812,#49813,#49814,#49815,#49816,
#49817,#49818,#49819,#49820,#49821,#49822,#49823,#49824,#49825,#49826,#49827,
#49828,#49829,#49830,#49831,#49832,#49833,#49834,#49835,#49836,#49837,#49838,
#49839,#49840,#49841,#49842,#49843,#49844),.UNSPECIFIED.,.F.,.F.,(4,3,3,
3,3,3,3,3,3,3,3,3,3,3,3,3,3,3,4),(-0.854915111010944,-0.822925495947057,
-0.800365095426597,-0.75633398547855,-0.748469100844136,-0.742037773638304,
-0.645772245378637,-0.632162604915744,-0.459766793866444,-0.38991304085735,
-0.38779448365469,-0.315984565381592,-0.310449867153767,-0.30493629935315,
-0.167082233063672,-0.154397747235191,-0.14936263256871,-0.00258798757819179,
0.),.UNSPECIFIED.);
#603=B_SPLINE_CURVE_WITH_KNOTS('',3,(#49845,#49846,#49847,#49848,#49849,
#49850,#49851,#49852,#49853,#49854,#49855,#49856,#49857,#49858,#49859,#49860,
#49861,#49862,#49863,#49864,#49865,#49866,#49867,#49868,#49869,#49870,#49871,
#49872,#49873,#49874,#49875,#49876,#49877,#49878,#49879,#49880,#49881,#49882,
#49883,#49884,#49885,#49886,#49887,#49888,#49889,#49890,#49891,#49892,#49893,
#49894,#49895,#49896),.UNSPECIFIED.,.F.,.F.,(4,3,3,3,3,3,3,3,3,3,3,3,3,
3,3,3,3,4),(-0.865008878888613,-0.810020253230451,-0.667799397338663,-0.661220440996107,
-0.656149039337886,-0.510599083577838,-0.503912127317129,-0.497491726604393,
-0.417709321956839,-0.355786573118897,-0.34402092652179,-0.338375890722606,
-0.294627424667398,-0.255060288195652,-0.188293674813484,-0.175394629447954,
-0.00556396810409777,0.),.UNSPECIFIED.);
#604=B_SPLINE_CURVE_WITH_KNOTS('',3,(#49954,#49955,#49956,#49957,#49958,
#49959),.UNSPECIFIED.,.F.,.F.,(4,2,4),(0.000198558815412191,0.00408016890061404,
0.00800258217218409),.UNSPECIFIED.);
#605=CONICAL_SURFACE('',#10189,0.0026,0.394791119699761);
#606=CONICAL_SURFACE('',#10204,0.0026,0.394791119699761);
#607=CONICAL_SURFACE('',#10207,0.0026,0.394791119699761);
#608=CONICAL_SURFACE('',#10215,0.0027,0.540419500270585);
#609=CONICAL_SURFACE('',#10219,0.0027,0.540419500270585);
#610=CONICAL_SURFACE('',#10227,0.0027,0.540419500270585);
#611=CONICAL_SURFACE('',#10235,0.0027,0.540419500270585);
#612=CONICAL_SURFACE('',#10257,0.0026,0.394791119699761);
#613=CONICAL_SURFACE('',#10273,0.0041,0.785398163397448);
#614=CONICAL_SURFACE('',#10281,0.0079,0.785398163397448);
#615=CONICAL_SURFACE('',#10288,0.0079,0.785398163397448);
#616=CONICAL_SURFACE('',#10289,0.00305,0.785398163397448);
#617=CONICAL_SURFACE('',#10296,0.0023,0.950546840812075);
#618=CONICAL_SURFACE('',#10351,0.0045,0.0523598775598298);
#619=CONICAL_SURFACE('',#10353,0.0045,0.0523598775598298);
#620=CONICAL_SURFACE('',#10354,0.0045,0.0523598775598298);
#621=CONICAL_SURFACE('',#10355,0.0045,0.0523598775598298);
#622=CONICAL_SURFACE('',#10356,0.0045,0.0523598775598298);
#623=CONICAL_SURFACE('',#10357,0.0045,0.0523598775598298);
#624=CONICAL_SURFACE('',#10358,0.0045,0.0523598775598298);
#625=CONICAL_SURFACE('',#10360,0.0045,0.0523598775598298);
#626=CONICAL_SURFACE('',#10363,0.0045,0.0523598775598298);
#627=CONICAL_SURFACE('',#10366,0.0045,0.0523598775598298);
#628=CONICAL_SURFACE('',#10369,0.0045,0.0523598775598298);
#629=CONICAL_SURFACE('',#10372,0.0045,0.0523598775598298);
#630=CONICAL_SURFACE('',#10537,0.0032,0.785398163397449);
#631=CONICAL_SURFACE('',#10542,0.0032,0.785398163397448);
#632=CONICAL_SURFACE('',#10543,0.0016,0.785398163397449);
#633=CONICAL_SURFACE('',#10544,0.0031,0.785398163397449);
#634=CONICAL_SURFACE('',#10547,0.0016,0.785398163397449);
#635=CONICAL_SURFACE('',#10556,0.00175,0.785398163397448);
#636=CONICAL_SURFACE('',#10561,0.00175,0.785398163397449);
#637=CONICAL_SURFACE('',#10585,0.0031,0.785398163397448);
#638=CONICAL_SURFACE('',#10592,0.0016,0.785398163397448);
#639=CONICAL_SURFACE('',#10635,0.0011,0.785398163397448);
#640=CONICAL_SURFACE('',#10642,0.0022,0.785398163397448);
#641=CONICAL_SURFACE('',#10649,0.00155,0.832981266674431);
#642=CONICAL_SURFACE('',#10650,0.00265,0.785398163397448);
#643=CONICAL_SURFACE('',#10657,0.0029,0.785398163397448);
#644=CONICAL_SURFACE('',#10665,0.0029,0.785398163397449);
#645=CONICAL_SURFACE('',#10670,0.0028,0.785398163397449);
#646=CONICAL_SURFACE('',#10676,0.0028,0.785398163397448);
#647=CONICAL_SURFACE('',#10696,0.00125,0.643501108793284);
#648=CONICAL_SURFACE('',#10727,0.00075,1.43824479449822);
#649=CONICAL_SURFACE('',#10728,0.00075,1.43824479449822);
#650=CONICAL_SURFACE('',#10729,0.00075,1.43824479449822);
#651=CONICAL_SURFACE('',#10730,0.0006,0.321750554396642);
#652=CONICAL_SURFACE('',#10736,0.0012,0.674740942223553);
#653=CONICAL_SURFACE('',#10742,0.0024,0.785398163397448);
#654=CONICAL_SURFACE('',#10892,0.0013,0.785398163397448);
#655=CONICAL_SURFACE('',#10937,0.00115470053837925,0.78539816339745);
#656=CONICAL_SURFACE('',#10944,0.001125,0.785398163397445);
#657=CONICAL_SURFACE('',#10954,0.00115470053837925,0.78539816339745);
#658=CONICAL_SURFACE('',#10955,0.00115470053837925,0.78539816339745);
#659=CONICAL_SURFACE('',#10956,0.00115470053837925,0.78539816339745);
#660=CONICAL_SURFACE('',#10957,0.00115470053837925,0.78539816339745);
#661=CONICAL_SURFACE('',#10958,0.00115470053837925,0.78539816339745);
#662=CONICAL_SURFACE('',#11001,0.0027,0.785398163397448);
#663=CONICAL_SURFACE('',#11007,0.0027,0.785398163397448);
#664=CONICAL_SURFACE('',#11014,0.0039,0.785398163397448);
#665=(
BOUNDED_CURVE()
B_SPLINE_CURVE(2,(#13666,#13667,#13668),.UNSPECIFIED.,.F.,.F.)
B_SPLINE_CURVE_WITH_KNOTS((3,3),(0.,0.130388293175992),.UNSPECIFIED.)
CURVE()
GEOMETRIC_REPRESENTATION_ITEM()
RATIONAL_B_SPLINE_CURVE((1.,1.00525170247464,1.))
REPRESENTATION_ITEM('')
);
#666=(
BOUNDED_CURVE()
B_SPLINE_CURVE(2,(#13674,#13675,#13676),.UNSPECIFIED.,.F.,.F.)
B_SPLINE_CURVE_WITH_KNOTS((3,3),(0.,0.130388293175992),.UNSPECIFIED.)
CURVE()
GEOMETRIC_REPRESENTATION_ITEM()
RATIONAL_B_SPLINE_CURVE((1.,1.00525170247464,1.))
REPRESENTATION_ITEM('')
);
#667=(
BOUNDED_CURVE()
B_SPLINE_CURVE(2,(#13686,#13687,#13688),.UNSPECIFIED.,.F.,.F.)
B_SPLINE_CURVE_WITH_KNOTS((3,3),(0.,0.1309950991442),.UNSPECIFIED.)
CURVE()
GEOMETRIC_REPRESENTATION_ITEM()
RATIONAL_B_SPLINE_CURVE((1.,1.00582981008257,1.))
REPRESENTATION_ITEM('')
);
#668=(
BOUNDED_CURVE()
B_SPLINE_CURVE(2,(#13697,#13698,#13699),.UNSPECIFIED.,.F.,.F.)
B_SPLINE_CURVE_WITH_KNOTS((3,3),(0.,0.1309950991442),.UNSPECIFIED.)
CURVE()
GEOMETRIC_REPRESENTATION_ITEM()
RATIONAL_B_SPLINE_CURVE((1.,1.00582981008257,1.))
REPRESENTATION_ITEM('')
);
#669=(
BOUNDED_CURVE()
B_SPLINE_CURVE(2,(#13708,#13709,#13710),.UNSPECIFIED.,.F.,.F.)
B_SPLINE_CURVE_WITH_KNOTS((3,3),(0.,0.1309950991442),.UNSPECIFIED.)
CURVE()
GEOMETRIC_REPRESENTATION_ITEM()
RATIONAL_B_SPLINE_CURVE((1.,1.00582981008257,1.))
REPRESENTATION_ITEM('')
);
#670=(
BOUNDED_CURVE()
B_SPLINE_CURVE(2,(#13715,#13716,#13717),.UNSPECIFIED.,.F.,.F.)
B_SPLINE_CURVE_WITH_KNOTS((3,3),(0.,0.130388293175992),.UNSPECIFIED.)
CURVE()
GEOMETRIC_REPRESENTATION_ITEM()
RATIONAL_B_SPLINE_CURVE((1.,1.00525170247464,1.))
REPRESENTATION_ITEM('')
);
#671=(
BOUNDED_CURVE()
B_SPLINE_CURVE(2,(#13727,#13728,#13729),.UNSPECIFIED.,.F.,.F.)
B_SPLINE_CURVE_WITH_KNOTS((3,3),(0.,0.130388293175992),.UNSPECIFIED.)
CURVE()
GEOMETRIC_REPRESENTATION_ITEM()
RATIONAL_B_SPLINE_CURVE((1.,1.00525170247464,1.))
REPRESENTATION_ITEM('')
);
#672=(
BOUNDED_CURVE()
B_SPLINE_CURVE(2,(#13732,#13733,#13734),.UNSPECIFIED.,.F.,.F.)
B_SPLINE_CURVE_WITH_KNOTS((3,3),(0.,0.1309950991442),.UNSPECIFIED.)
CURVE()
GEOMETRIC_REPRESENTATION_ITEM()
RATIONAL_B_SPLINE_CURVE((1.,1.00582981008257,1.))
REPRESENTATION_ITEM('')
);
#673=(
BOUNDED_CURVE()
B_SPLINE_CURVE(2,(#13762,#13763,#13764),.UNSPECIFIED.,.F.,.F.)
B_SPLINE_CURVE_WITH_KNOTS((3,3),(0.13740622471284,0.194564395432606),
 .UNSPECIFIED.)
CURVE()
GEOMETRIC_REPRESENTATION_ITEM()
RATIONAL_B_SPLINE_CURVE((1.0210752443686,1.02155284321629,1.018780946918))
REPRESENTATION_ITEM('')
);
#674=(
BOUNDED_CURVE()
B_SPLINE_CURVE(2,(#13772,#13773,#13774),.UNSPECIFIED.,.F.,.F.)
B_SPLINE_CURVE_WITH_KNOTS((3,3),(-0.194564395432341,-0.137406224712621),
 .UNSPECIFIED.)
CURVE()
GEOMETRIC_REPRESENTATION_ITEM()
RATIONAL_B_SPLINE_CURVE((1.01878094691633,1.02155284321435,1.02107524436669))
REPRESENTATION_ITEM('')
);
#675=(
BOUNDED_CURVE()
B_SPLINE_CURVE(2,(#13806,#13807,#13808),.UNSPECIFIED.,.F.,.F.)
B_SPLINE_CURVE_WITH_KNOTS((3,3),(0.137406224811474,0.19456439553049),
 .UNSPECIFIED.)
CURVE()
GEOMETRIC_REPRESENTATION_ITEM()
RATIONAL_B_SPLINE_CURVE((1.02107524478079,1.02155284363217,1.01878094727436))
REPRESENTATION_ITEM('')
);
#676=(
BOUNDED_CURVE()
B_SPLINE_CURVE(2,(#13815,#13816,#13817),.UNSPECIFIED.,.F.,.F.)
B_SPLINE_CURVE_WITH_KNOTS((3,3),(-0.194564395470828,-0.137406224751148),
 .UNSPECIFIED.)
CURVE()
GEOMETRIC_REPRESENTATION_ITEM()
RATIONAL_B_SPLINE_CURVE((1.01878094706027,1.02155284338227,1.02107524453305))
REPRESENTATION_ITEM('')
);
#677=(
BOUNDED_CURVE()
B_SPLINE_CURVE(2,(#27879,#27880,#27881),.UNSPECIFIED.,.F.,.F.)
B_SPLINE_CURVE_WITH_KNOTS((3,3),(1.09880286001687,1.11425993114071),
 .UNSPECIFIED.)
CURVE()
GEOMETRIC_REPRESENTATION_ITEM()
RATIONAL_B_SPLINE_CURVE((1.37837837838126,1.31211005581294,1.24390243902605))
REPRESENTATION_ITEM('')
);
#678=(
BOUNDED_CURVE()
B_SPLINE_CURVE(2,(#27888,#27889,#27890),.UNSPECIFIED.,.F.,.F.)
B_SPLINE_CURVE_WITH_KNOTS((3,3),(0.0269674782770168,0.0424245494010484),
 .UNSPECIFIED.)
CURVE()
GEOMETRIC_REPRESENTATION_ITEM()
RATIONAL_B_SPLINE_CURVE((1.24390243902529,1.31211005581301,1.37837837838213))
REPRESENTATION_ITEM('')
);
#679=(
BOUNDED_CURVE()
B_SPLINE_CURVE(2,(#27949,#27950,#27951),.UNSPECIFIED.,.F.,.F.)
B_SPLINE_CURVE_WITH_KNOTS((3,3),(0.0269674782769955,0.0424245494010537),
 .UNSPECIFIED.)
CURVE()
GEOMETRIC_REPRESENTATION_ITEM()
RATIONAL_B_SPLINE_CURVE((1.2439024390251,1.31211005581295,1.37837837838218))
REPRESENTATION_ITEM('')
);
#680=(
BOUNDED_CURVE()
B_SPLINE_CURVE(2,(#27969,#27970,#27971),.UNSPECIFIED.,.F.,.F.)
B_SPLINE_CURVE_WITH_KNOTS((3,3),(1.09880286001689,1.11425993114073),
 .UNSPECIFIED.)
CURVE()
GEOMETRIC_REPRESENTATION_ITEM()
RATIONAL_B_SPLINE_CURVE((1.37837837838082,1.3121100558125,1.24390243902561))
REPRESENTATION_ITEM('')
);
#681=(
BOUNDED_CURVE()
B_SPLINE_CURVE(2,(#48307,#48308,#48309),.UNSPECIFIED.,.F.,.F.)
B_SPLINE_CURVE_WITH_KNOTS((3,3),(-0.321867155116299,-0.124274873543865),
 .UNSPECIFIED.)
CURVE()
GEOMETRIC_REPRESENTATION_ITEM()
RATIONAL_B_SPLINE_CURVE((1.46410161513778,1.69059892324148,1.46410161513778))
REPRESENTATION_ITEM('')
);
#682=(
BOUNDED_CURVE()
B_SPLINE_CURVE(2,(#49214,#49215,#49216),.UNSPECIFIED.,.F.,.F.)
B_SPLINE_CURVE_WITH_KNOTS((3,3),(-0.3218671551163,-0.124274873543865),
 .UNSPECIFIED.)
CURVE()
GEOMETRIC_REPRESENTATION_ITEM()
RATIONAL_B_SPLINE_CURVE((1.46410161513778,1.69059892324148,1.46410161513778))
REPRESENTATION_ITEM('')
);
#683=(
BOUNDED_CURVE()
B_SPLINE_CURVE(2,(#49218,#49219,#49220),.UNSPECIFIED.,.F.,.F.)
B_SPLINE_CURVE_WITH_KNOTS((3,3),(-0.321867155116299,-0.124274873543866),
 .UNSPECIFIED.)
CURVE()
GEOMETRIC_REPRESENTATION_ITEM()
RATIONAL_B_SPLINE_CURVE((1.46410161513778,1.69059892324148,1.46410161513778))
REPRESENTATION_ITEM('')
);
#684=(
BOUNDED_CURVE()
B_SPLINE_CURVE(2,(#49222,#49223,#49224),.UNSPECIFIED.,.F.,.F.)
B_SPLINE_CURVE_WITH_KNOTS((3,3),(-0.3218671551163,-0.124274873543865),
 .UNSPECIFIED.)
CURVE()
GEOMETRIC_REPRESENTATION_ITEM()
RATIONAL_B_SPLINE_CURVE((1.46410161513778,1.69059892324148,1.46410161513778))
REPRESENTATION_ITEM('')
);
#685=(
BOUNDED_CURVE()
B_SPLINE_CURVE(2,(#49226,#49227,#49228),.UNSPECIFIED.,.F.,.F.)
B_SPLINE_CURVE_WITH_KNOTS((3,3),(-0.3218671551163,-0.124274873543865),
 .UNSPECIFIED.)
CURVE()
GEOMETRIC_REPRESENTATION_ITEM()
RATIONAL_B_SPLINE_CURVE((1.46410161513778,1.69059892324148,1.46410161513778))
REPRESENTATION_ITEM('')
);
#686=(
BOUNDED_CURVE()
B_SPLINE_CURVE(2,(#49230,#49231,#49232),.UNSPECIFIED.,.F.,.F.)
B_SPLINE_CURVE_WITH_KNOTS((3,3),(-0.321867155116299,-0.124274873543866),
 .UNSPECIFIED.)
CURVE()
GEOMETRIC_REPRESENTATION_ITEM()
RATIONAL_B_SPLINE_CURVE((1.46410161513778,1.69059892324148,1.46410161513778))
REPRESENTATION_ITEM('')
);
#687=ELLIPSE('',#10162,0.0240831891575954,0.00200000000001);
#688=ELLIPSE('',#10163,0.0101980390271974,0.00200000000001);
#689=ELLIPSE('',#10165,0.0101980390271974,0.00200000000001);
#690=ELLIPSE('',#10166,0.0240831891575954,0.00200000000001);
#691=ELLIPSE('',#10168,0.0240831891575954,0.00200000000001);
#692=ELLIPSE('',#10169,0.0101980390271974,0.00200000000001);
#693=ELLIPSE('',#10171,0.0101980390271974,0.00200000000001);
#694=ELLIPSE('',#10172,0.0240831891575954,0.00200000000001);
#695=ELLIPSE('',#10174,0.0240831891575954,0.00200000000001);
#696=ELLIPSE('',#10175,0.0101980390271974,0.00200000000001);
#697=ELLIPSE('',#10177,0.0101980390271974,0.00200000000001);
#698=ELLIPSE('',#10178,0.0240831891575954,0.00200000000001);
#699=ELLIPSE('',#10180,0.0240831891575954,0.00200000000001);
#700=ELLIPSE('',#10181,0.0101980390271974,0.00200000000001);
#701=ELLIPSE('',#10183,0.0101980390271974,0.00200000000001);
#702=ELLIPSE('',#10184,0.0240831891575954,0.00200000000001);
#703=ELLIPSE('',#10402,0.00417722093727662,0.00387500000001);
#704=ELLIPSE('',#10406,0.00417722093727662,0.00387500000001);
#705=ELLIPSE('',#10579,0.00198146070825073,0.00138139923663895);
#706=ELLIPSE('',#10580,0.00189052267529393,0.00133517872970212);
#707=ELLIPSE('',#10581,0.00182395398435439,0.00131739606577714);
#708=ELLIPSE('',#10582,0.0020993200218241,0.00147094440040091);
#709=ELLIPSE('',#10600,0.00132114477356862,0.00112846649906451);
#710=FACE_BOUND('',#1658,.T.);
#711=FACE_BOUND('',#1663,.T.);
#712=FACE_BOUND('',#1723,.T.);
#713=FACE_BOUND('',#1726,.T.);
#714=FACE_BOUND('',#1731,.T.);
#715=FACE_BOUND('',#1740,.T.);
#716=FACE_BOUND('',#1742,.T.);
#717=FACE_BOUND('',#1744,.T.);
#718=FACE_BOUND('',#1746,.T.);
#719=FACE_BOUND('',#1748,.T.);
#720=FACE_BOUND('',#1750,.T.);
#721=FACE_BOUND('',#1752,.T.);
#722=FACE_BOUND('',#1754,.T.);
#723=FACE_BOUND('',#1756,.T.);
#724=FACE_BOUND('',#1758,.T.);
#725=FACE_BOUND('',#1760,.T.);
#726=FACE_BOUND('',#1762,.T.);
#727=FACE_BOUND('',#1764,.T.);
#728=FACE_BOUND('',#1766,.T.);
#729=FACE_BOUND('',#1768,.T.);
#730=FACE_BOUND('',#1785,.T.);
#731=FACE_BOUND('',#1792,.T.);
#732=FACE_BOUND('',#1795,.T.);
#733=FACE_BOUND('',#1797,.T.);
#734=FACE_BOUND('',#1800,.T.);
#735=FACE_BOUND('',#1802,.T.);
#736=FACE_BOUND('',#1805,.T.);
#737=FACE_BOUND('',#1807,.T.);
#738=FACE_BOUND('',#1810,.T.);
#739=FACE_BOUND('',#1812,.T.);
#740=FACE_BOUND('',#1815,.T.);
#741=FACE_BOUND('',#1894,.T.);
#742=FACE_BOUND('',#1897,.T.);
#743=FACE_BOUND('',#1898,.T.);
#744=FACE_BOUND('',#1917,.T.);
#745=FACE_BOUND('',#1931,.T.);
#746=FACE_BOUND('',#1932,.T.);
#747=FACE_BOUND('',#1939,.T.);
#748=FACE_BOUND('',#1977,.T.);
#749=FACE_BOUND('',#1980,.T.);
#750=FACE_BOUND('',#1990,.T.);
#751=FACE_BOUND('',#1995,.T.);
#752=FACE_BOUND('',#1998,.T.);
#753=FACE_BOUND('',#2016,.T.);
#754=FACE_BOUND('',#2020,.T.);
#755=FACE_BOUND('',#2023,.T.);
#756=FACE_BOUND('',#2031,.T.);
#757=FACE_BOUND('',#2037,.T.);
#758=FACE_BOUND('',#2055,.T.);
#759=FACE_BOUND('',#2063,.T.);
#760=FACE_BOUND('',#2101,.T.);
#761=FACE_BOUND('',#2102,.T.);
#762=FACE_BOUND('',#2137,.T.);
#763=FACE_BOUND('',#2139,.T.);
#764=FACE_BOUND('',#2197,.T.);
#765=FACE_BOUND('',#2203,.T.);
#766=FACE_BOUND('',#2205,.T.);
#767=FACE_BOUND('',#2235,.T.);
#768=FACE_BOUND('',#2238,.T.);
#769=TOROIDAL_SURFACE('',#10120,0.003,0.000375);
#770=TOROIDAL_SURFACE('',#10133,0.003,0.000375);
#771=TOROIDAL_SURFACE('',#10140,0.00285,0.0004);
#772=TOROIDAL_SURFACE('',#10156,0.0024,0.0004);
#773=TOROIDAL_SURFACE('',#10434,0.003,0.00075);
#774=TOROIDAL_SURFACE('',#10445,0.003,0.000375);
#775=TOROIDAL_SURFACE('',#10458,0.003,0.000375);
#776=TOROIDAL_SURFACE('',#10612,0.003,0.00025);
#777=TOROIDAL_SURFACE('',#10859,0.00685,0.0016);
#778=TOROIDAL_SURFACE('',#10973,0.003,0.00075);
#779=TOROIDAL_SURFACE('',#10984,0.003,0.00025);
#780=SHAPE_REPRESENTATION_RELATIONSHIP('SRR','None',#50148,#800);
#781=SHAPE_REPRESENTATION_RELATIONSHIP('SRR','None',#50149,#801);
#782=SHAPE_REPRESENTATION_RELATIONSHIP('SRR','None',#50150,#802);
#783=SHAPE_REPRESENTATION_RELATIONSHIP('SRR','None',#50151,#803);
#784=SHAPE_REPRESENTATION_RELATIONSHIP('SRR','None',#50152,#804);
#785=SHAPE_REPRESENTATION_RELATIONSHIP('SRR','None',#50153,#805);
#786=SHAPE_REPRESENTATION_RELATIONSHIP('SRR','None',#50154,#806);
#787=SHAPE_REPRESENTATION_RELATIONSHIP('SRR','None',#50155,#807);
#788=SHAPE_REPRESENTATION_RELATIONSHIP('SRR','None',#50156,#808);
#789=SHAPE_REPRESENTATION_RELATIONSHIP('SRR','None',#50157,#809);
#790=SHAPE_REPRESENTATION_RELATIONSHIP('SRR','None',#50158,#810);
#791=SHAPE_REPRESENTATION_RELATIONSHIP('SRR','None',#50159,#811);
#792=SHAPE_REPRESENTATION_RELATIONSHIP('SRR','None',#50160,#812);
#793=SHAPE_REPRESENTATION_RELATIONSHIP('SRR','None',#50161,#813);
#794=SHAPE_REPRESENTATION_RELATIONSHIP('SRR','None',#50162,#814);
#795=SHAPE_REPRESENTATION_RELATIONSHIP('SRR','None',#50163,#815);
#796=SHAPE_REPRESENTATION_RELATIONSHIP('SRR','None',#50164,#816);
#797=SHAPE_REPRESENTATION_RELATIONSHIP('SRR','None',#50165,#817);
#798=SHAPE_REPRESENTATION_RELATIONSHIP('SRR','None',#50166,#818);
#799=SHAPE_REPRESENTATION_RELATIONSHIP('SRR','None',#50167,#819);
#800=ADVANCED_BREP_SHAPE_REPRESENTATION('',(#840),#50061);
#801=ADVANCED_BREP_SHAPE_REPRESENTATION('',(#841),#50062);
#802=ADVANCED_BREP_SHAPE_REPRESENTATION('',(#842),#50063);
#803=ADVANCED_BREP_SHAPE_REPRESENTATION('',(#843),#50064);
#804=ADVANCED_BREP_SHAPE_REPRESENTATION('',(#844),#50065);
#805=ADVANCED_BREP_SHAPE_REPRESENTATION('',(#845),#50066);
#806=ADVANCED_BREP_SHAPE_REPRESENTATION('',(#846),#50067);
#807=ADVANCED_BREP_SHAPE_REPRESENTATION('',(#847),#50068);
#808=ADVANCED_BREP_SHAPE_REPRESENTATION('',(#848),#50069);
#809=ADVANCED_BREP_SHAPE_REPRESENTATION('',(#849),#50070);
#810=ADVANCED_BREP_SHAPE_REPRESENTATION('',(#850),#50071);
#811=ADVANCED_BREP_SHAPE_REPRESENTATION('',(#851),#50072);
#812=ADVANCED_BREP_SHAPE_REPRESENTATION('',(#852),#50073);
#813=ADVANCED_BREP_SHAPE_REPRESENTATION('',(#853),#50074);
#814=ADVANCED_BREP_SHAPE_REPRESENTATION('',(#854),#50075);
#815=ADVANCED_BREP_SHAPE_REPRESENTATION('',(#855),#50076);
#816=ADVANCED_BREP_SHAPE_REPRESENTATION('',(#856),#50077);
#817=ADVANCED_BREP_SHAPE_REPRESENTATION('',(#857),#50078);
#818=ADVANCED_BREP_SHAPE_REPRESENTATION('',(#858),#50079);
#819=ADVANCED_BREP_SHAPE_REPRESENTATION('',(#859),#50080);
#820=STYLED_ITEM('',(#50257),#840);
#821=STYLED_ITEM('',(#50258),#841);
#822=STYLED_ITEM('',(#50259),#842);
#823=STYLED_ITEM('',(#50260),#843);
#824=STYLED_ITEM('',(#50261),#844);
#825=STYLED_ITEM('',(#50259),#845);
#826=STYLED_ITEM('',(#50259),#846);
#827=STYLED_ITEM('',(#50262),#847);
#828=STYLED_ITEM('',(#50260),#848);
#829=STYLED_ITEM('',(#50259),#849);
#830=STYLED_ITEM('',(#50260),#850);
#831=STYLED_ITEM('',(#50261),#851);
#832=STYLED_ITEM('',(#50258),#852);
#833=STYLED_ITEM('',(#50259),#853);
#834=STYLED_ITEM('',(#50257),#854);
#835=STYLED_ITEM('',(#50262),#855);
#836=STYLED_ITEM('',(#50258),#856);
#837=STYLED_ITEM('',(#50259),#857);
#838=STYLED_ITEM('',(#50260),#858);
#839=STYLED_ITEM('',(#50261),#859);
#840=MANIFOLD_SOLID_BREP('Body1',#9865);
#841=MANIFOLD_SOLID_BREP('Body1',#9866);
#842=MANIFOLD_SOLID_BREP('Body1',#9867);
#843=MANIFOLD_SOLID_BREP('Body1',#9868);
#844=MANIFOLD_SOLID_BREP('Body1',#9869);
#845=MANIFOLD_SOLID_BREP('Body1',#9870);
#846=MANIFOLD_SOLID_BREP('Body1',#9871);
#847=MANIFOLD_SOLID_BREP('Body1',#9872);
#848=MANIFOLD_SOLID_BREP('Body1',#9873);
#849=MANIFOLD_SOLID_BREP('Body1',#9874);
#850=MANIFOLD_SOLID_BREP('Body1',#9875);
#851=MANIFOLD_SOLID_BREP('Body1',#9876);
#852=MANIFOLD_SOLID_BREP('Body1',#9877);
#853=MANIFOLD_SOLID_BREP('Body1',#9878);
#854=MANIFOLD_SOLID_BREP('Body1',#9879);
#855=MANIFOLD_SOLID_BREP('Body1',#9880);
#856=MANIFOLD_SOLID_BREP('Body1',#9881);
#857=MANIFOLD_SOLID_BREP('Body1',#9882);
#858=MANIFOLD_SOLID_BREP('Body1',#9883);
#859=MANIFOLD_SOLID_BREP('Body1',#9884);
#860=PLANE('',#10111);
#861=PLANE('',#10112);
#862=PLANE('',#10114);
#863=PLANE('',#10125);
#864=PLANE('',#10127);
#865=PLANE('',#10138);
#866=PLANE('',#10144);
#867=PLANE('',#10186);
#868=PLANE('',#10188);
#869=PLANE('',#10192);
#870=PLANE('',#10193);
#871=PLANE('',#10194);
#872=PLANE('',#10195);
#873=PLANE('',#10197);
#874=PLANE('',#10198);
#875=PLANE('',#10200);
#876=PLANE('',#10201);
#877=PLANE('',#10202);
#878=PLANE('',#10206);
#879=PLANE('',#10209);
#880=PLANE('',#10210);
#881=PLANE('',#10211);
#882=PLANE('',#10213);
#883=PLANE('',#10218);
#884=PLANE('',#10222);
#885=PLANE('',#10223);
#886=PLANE('',#10224);
#887=PLANE('',#10225);
#888=PLANE('',#10231);
#889=PLANE('',#10232);
#890=PLANE('',#10233);
#891=PLANE('',#10234);
#892=PLANE('',#10238);
#893=PLANE('',#10239);
#894=PLANE('',#10240);
#895=PLANE('',#10241);
#896=PLANE('',#10242);
#897=PLANE('',#10243);
#898=PLANE('',#10244);
#899=PLANE('',#10245);
#900=PLANE('',#10246);
#901=PLANE('',#10247);
#902=PLANE('',#10248);
#903=PLANE('',#10249);
#904=PLANE('',#10250);
#905=PLANE('',#10251);
#906=PLANE('',#10252);
#907=PLANE('',#10254);
#908=PLANE('',#10256);
#909=PLANE('',#10260);
#910=PLANE('',#10262);
#911=PLANE('',#10264);
#912=PLANE('',#10276);
#913=PLANE('',#10286);
#914=PLANE('',#10295);
#915=PLANE('',#10297);
#916=PLANE('',#10300);
#917=PLANE('',#10303);
#918=PLANE('',#10306);
#919=PLANE('',#10309);
#920=PLANE('',#10312);
#921=PLANE('',#10315);
#922=PLANE('',#10318);
#923=PLANE('',#10321);
#924=PLANE('',#10324);
#925=PLANE('',#10327);
#926=PLANE('',#10330);
#927=PLANE('',#10333);
#928=PLANE('',#10336);
#929=PLANE('',#10339);
#930=PLANE('',#10359);
#931=PLANE('',#10373);
#932=PLANE('',#10377);
#933=PLANE('',#10378);
#934=PLANE('',#10382);
#935=PLANE('',#10383);
#936=PLANE('',#10387);
#937=PLANE('',#10388);
#938=PLANE('',#10392);
#939=PLANE('',#10393);
#940=PLANE('',#10398);
#941=PLANE('',#10401);
#942=PLANE('',#10403);
#943=PLANE('',#10405);
#944=PLANE('',#10407);
#945=PLANE('',#10412);
#946=PLANE('',#10413);
#947=PLANE('',#10414);
#948=PLANE('',#10415);
#949=PLANE('',#10416);
#950=PLANE('',#10423);
#951=PLANE('',#10424);
#952=PLANE('',#10425);
#953=PLANE('',#10426);
#954=PLANE('',#10428);
#955=PLANE('',#10439);
#956=PLANE('',#10451);
#957=PLANE('',#10452);
#958=PLANE('',#10464);
#959=PLANE('',#10465);
#960=PLANE('',#10515);
#961=PLANE('',#10516);
#962=PLANE('',#10517);
#963=PLANE('',#10518);
#964=PLANE('',#10520);
#965=PLANE('',#10521);
#966=PLANE('',#10526);
#967=PLANE('',#10527);
#968=PLANE('',#10528);
#969=PLANE('',#10539);
#970=PLANE('',#10549);
#971=PLANE('',#10550);
#972=PLANE('',#10551);
#973=PLANE('',#10552);
#974=PLANE('',#10553);
#975=PLANE('',#10554);
#976=PLANE('',#10555);
#977=PLANE('',#10558);
#978=PLANE('',#10559);
#979=PLANE('',#10560);
#980=PLANE('',#10565);
#981=PLANE('',#10567);
#982=PLANE('',#10568);
#983=PLANE('',#10569);
#984=PLANE('',#10570);
#985=PLANE('',#10571);
#986=PLANE('',#10572);
#987=PLANE('',#10575);
#988=PLANE('',#10576);
#989=PLANE('',#10583);
#990=PLANE('',#10584);
#991=PLANE('',#10591);
#992=PLANE('',#10595);
#993=PLANE('',#10596);
#994=PLANE('',#10599);
#995=PLANE('',#10605);
#996=PLANE('',#10606);
#997=PLANE('',#10618);
#998=PLANE('',#10619);
#999=PLANE('',#10640);
#1000=PLANE('',#10645);
#1001=PLANE('',#10654);
#1002=PLANE('',#10659);
#1003=PLANE('',#10660);
#1004=PLANE('',#10663);
#1005=PLANE('',#10666);
#1006=PLANE('',#10675);
#1007=PLANE('',#10678);
#1008=PLANE('',#10695);
#1009=PLANE('',#10698);
#1010=PLANE('',#10699);
#1011=PLANE('',#10701);
#1012=PLANE('',#10702);
#1013=PLANE('',#10704);
#1014=PLANE('',#10705);
#1015=PLANE('',#10706);
#1016=PLANE('',#10707);
#1017=PLANE('',#10708);
#1018=PLANE('',#10709);
#1019=PLANE('',#10710);
#1020=PLANE('',#10712);
#1021=PLANE('',#10713);
#1022=PLANE('',#10714);
#1023=PLANE('',#10715);
#1024=PLANE('',#10716);
#1025=PLANE('',#10718);
#1026=PLANE('',#10719);
#1027=PLANE('',#10720);
#1028=PLANE('',#10721);
#1029=PLANE('',#10722);
#1030=PLANE('',#10723);
#1031=PLANE('',#10724);
#1032=PLANE('',#10725);
#1033=PLANE('',#10726);
#1034=PLANE('',#10739);
#1035=PLANE('',#10745);
#1036=PLANE('',#10746);
#1037=PLANE('',#10747);
#1038=PLANE('',#10809);
#1039=PLANE('',#10812);
#1040=PLANE('',#10813);
#1041=PLANE('',#10814);
#1042=PLANE('',#10815);
#1043=PLANE('',#10821);
#1044=PLANE('',#10822);
#1045=PLANE('',#10826);
#1046=PLANE('',#10827);
#1047=PLANE('',#10831);
#1048=PLANE('',#10832);
#1049=PLANE('',#10836);
#1050=PLANE('',#10837);
#1051=PLANE('',#10841);
#1052=PLANE('',#10842);
#1053=PLANE('',#10843);
#1054=PLANE('',#10844);
#1055=PLANE('',#10845);
#1056=PLANE('',#10846);
#1057=PLANE('',#10847);
#1058=PLANE('',#10848);
#1059=PLANE('',#10849);
#1060=PLANE('',#10850);
#1061=PLANE('',#10851);
#1062=PLANE('',#10852);
#1063=PLANE('',#10853);
#1064=PLANE('',#10854);
#1065=PLANE('',#10855);
#1066=PLANE('',#10856);
#1067=PLANE('',#10857);
#1068=PLANE('',#10858);
#1069=PLANE('',#10865);
#1070=PLANE('',#10866);
#1071=PLANE('',#10869);
#1072=PLANE('',#10870);
#1073=PLANE('',#10871);
#1074=PLANE('',#10874);
#1075=PLANE('',#10876);
#1076=PLANE('',#10877);
#1077=PLANE('',#10879);
#1078=PLANE('',#10883);
#1079=PLANE('',#10884);
#1080=PLANE('',#10888);
#1081=PLANE('',#10889);
#1082=PLANE('',#10890);
#1083=PLANE('',#10897);
#1084=PLANE('',#10898);
#1085=PLANE('',#10946);
#1086=PLANE('',#10947);
#1087=PLANE('',#10953);
#1088=PLANE('',#10959);
#1089=PLANE('',#10960);
#1090=PLANE('',#10961);
#1091=PLANE('',#10962);
#1092=PLANE('',#10963);
#1093=PLANE('',#10964);
#1094=PLANE('',#10965);
#1095=PLANE('',#10967);
#1096=PLANE('',#10978);
#1097=PLANE('',#10990);
#1098=PLANE('',#10991);
#1099=PLANE('',#11006);
#1100=PLANE('',#11009);
#1101=PLANE('',#11011);
#1102=FACE_OUTER_BOUND('',#1643,.T.);
#1103=FACE_OUTER_BOUND('',#1644,.T.);
#1104=FACE_OUTER_BOUND('',#1645,.T.);
#1105=FACE_OUTER_BOUND('',#1646,.T.);
#1106=FACE_OUTER_BOUND('',#1647,.T.);
#1107=FACE_OUTER_BOUND('',#1648,.T.);
#1108=FACE_OUTER_BOUND('',#1649,.T.);
#1109=FACE_OUTER_BOUND('',#1650,.T.);
#1110=FACE_OUTER_BOUND('',#1651,.T.);
#1111=FACE_OUTER_BOUND('',#1652,.T.);
#1112=FACE_OUTER_BOUND('',#1653,.T.);
#1113=FACE_OUTER_BOUND('',#1654,.T.);
#1114=FACE_OUTER_BOUND('',#1655,.T.);
#1115=FACE_OUTER_BOUND('',#1656,.T.);
#1116=FACE_OUTER_BOUND('',#1657,.T.);
#1117=FACE_OUTER_BOUND('',#1659,.T.);
#1118=FACE_OUTER_BOUND('',#1660,.T.);
#1119=FACE_OUTER_BOUND('',#1661,.T.);
#1120=FACE_OUTER_BOUND('',#1662,.T.);
#1121=FACE_OUTER_BOUND('',#1664,.T.);
#1122=FACE_OUTER_BOUND('',#1665,.T.);
#1123=FACE_OUTER_BOUND('',#1666,.T.);
#1124=FACE_OUTER_BOUND('',#1667,.T.);
#1125=FACE_OUTER_BOUND('',#1668,.T.);
#1126=FACE_OUTER_BOUND('',#1669,.T.);
#1127=FACE_OUTER_BOUND('',#1670,.T.);
#1128=FACE_OUTER_BOUND('',#1671,.T.);
#1129=FACE_OUTER_BOUND('',#1672,.T.);
#1130=FACE_OUTER_BOUND('',#1673,.T.);
#1131=FACE_OUTER_BOUND('',#1674,.T.);
#1132=FACE_OUTER_BOUND('',#1675,.T.);
#1133=FACE_OUTER_BOUND('',#1676,.T.);
#1134=FACE_OUTER_BOUND('',#1677,.T.);
#1135=FACE_OUTER_BOUND('',#1678,.T.);
#1136=FACE_OUTER_BOUND('',#1679,.T.);
#1137=FACE_OUTER_BOUND('',#1680,.T.);
#1138=FACE_OUTER_BOUND('',#1681,.T.);
#1139=FACE_OUTER_BOUND('',#1682,.T.);
#1140=FACE_OUTER_BOUND('',#1683,.T.);
#1141=FACE_OUTER_BOUND('',#1684,.T.);
#1142=FACE_OUTER_BOUND('',#1685,.T.);
#1143=FACE_OUTER_BOUND('',#1686,.T.);
#1144=FACE_OUTER_BOUND('',#1687,.T.);
#1145=FACE_OUTER_BOUND('',#1688,.T.);
#1146=FACE_OUTER_BOUND('',#1689,.T.);
#1147=FACE_OUTER_BOUND('',#1690,.T.);
#1148=FACE_OUTER_BOUND('',#1691,.T.);
#1149=FACE_OUTER_BOUND('',#1692,.T.);
#1150=FACE_OUTER_BOUND('',#1693,.T.);
#1151=FACE_OUTER_BOUND('',#1694,.T.);
#1152=FACE_OUTER_BOUND('',#1695,.T.);
#1153=FACE_OUTER_BOUND('',#1696,.T.);
#1154=FACE_OUTER_BOUND('',#1697,.T.);
#1155=FACE_OUTER_BOUND('',#1698,.T.);
#1156=FACE_OUTER_BOUND('',#1699,.T.);
#1157=FACE_OUTER_BOUND('',#1700,.T.);
#1158=FACE_OUTER_BOUND('',#1701,.T.);
#1159=FACE_OUTER_BOUND('',#1702,.T.);
#1160=FACE_OUTER_BOUND('',#1703,.T.);
#1161=FACE_OUTER_BOUND('',#1704,.T.);
#1162=FACE_OUTER_BOUND('',#1705,.T.);
#1163=FACE_OUTER_BOUND('',#1706,.T.);
#1164=FACE_OUTER_BOUND('',#1707,.T.);
#1165=FACE_OUTER_BOUND('',#1708,.T.);
#1166=FACE_OUTER_BOUND('',#1709,.T.);
#1167=FACE_OUTER_BOUND('',#1710,.T.);
#1168=FACE_OUTER_BOUND('',#1711,.T.);
#1169=FACE_OUTER_BOUND('',#1712,.T.);
#1170=FACE_OUTER_BOUND('',#1713,.T.);
#1171=FACE_OUTER_BOUND('',#1714,.T.);
#1172=FACE_OUTER_BOUND('',#1715,.T.);
#1173=FACE_OUTER_BOUND('',#1716,.T.);
#1174=FACE_OUTER_BOUND('',#1717,.T.);
#1175=FACE_OUTER_BOUND('',#1718,.T.);
#1176=FACE_OUTER_BOUND('',#1719,.T.);
#1177=FACE_OUTER_BOUND('',#1720,.T.);
#1178=FACE_OUTER_BOUND('',#1721,.T.);
#1179=FACE_OUTER_BOUND('',#1722,.T.);
#1180=FACE_OUTER_BOUND('',#1724,.T.);
#1181=FACE_OUTER_BOUND('',#1725,.T.);
#1182=FACE_OUTER_BOUND('',#1727,.T.);
#1183=FACE_OUTER_BOUND('',#1728,.T.);
#1184=FACE_OUTER_BOUND('',#1729,.T.);
#1185=FACE_OUTER_BOUND('',#1730,.T.);
#1186=FACE_OUTER_BOUND('',#1732,.T.);
#1187=FACE_OUTER_BOUND('',#1733,.T.);
#1188=FACE_OUTER_BOUND('',#1734,.T.);
#1189=FACE_OUTER_BOUND('',#1735,.T.);
#1190=FACE_OUTER_BOUND('',#1736,.T.);
#1191=FACE_OUTER_BOUND('',#1737,.T.);
#1192=FACE_OUTER_BOUND('',#1738,.T.);
#1193=FACE_OUTER_BOUND('',#1739,.T.);
#1194=FACE_OUTER_BOUND('',#1741,.T.);
#1195=FACE_OUTER_BOUND('',#1743,.T.);
#1196=FACE_OUTER_BOUND('',#1745,.T.);
#1197=FACE_OUTER_BOUND('',#1747,.T.);
#1198=FACE_OUTER_BOUND('',#1749,.T.);
#1199=FACE_OUTER_BOUND('',#1751,.T.);
#1200=FACE_OUTER_BOUND('',#1753,.T.);
#1201=FACE_OUTER_BOUND('',#1755,.T.);
#1202=FACE_OUTER_BOUND('',#1757,.T.);
#1203=FACE_OUTER_BOUND('',#1759,.T.);
#1204=FACE_OUTER_BOUND('',#1761,.T.);
#1205=FACE_OUTER_BOUND('',#1763,.T.);
#1206=FACE_OUTER_BOUND('',#1765,.T.);
#1207=FACE_OUTER_BOUND('',#1767,.T.);
#1208=FACE_OUTER_BOUND('',#1769,.T.);
#1209=FACE_OUTER_BOUND('',#1770,.T.);
#1210=FACE_OUTER_BOUND('',#1771,.T.);
#1211=FACE_OUTER_BOUND('',#1772,.T.);
#1212=FACE_OUTER_BOUND('',#1773,.T.);
#1213=FACE_OUTER_BOUND('',#1774,.T.);
#1214=FACE_OUTER_BOUND('',#1775,.T.);
#1215=FACE_OUTER_BOUND('',#1776,.T.);
#1216=FACE_OUTER_BOUND('',#1777,.T.);
#1217=FACE_OUTER_BOUND('',#1778,.T.);
#1218=FACE_OUTER_BOUND('',#1779,.T.);
#1219=FACE_OUTER_BOUND('',#1780,.T.);
#1220=FACE_OUTER_BOUND('',#1781,.T.);
#1221=FACE_OUTER_BOUND('',#1782,.T.);
#1222=FACE_OUTER_BOUND('',#1783,.T.);
#1223=FACE_OUTER_BOUND('',#1784,.T.);
#1224=FACE_OUTER_BOUND('',#1786,.T.);
#1225=FACE_OUTER_BOUND('',#1787,.T.);
#1226=FACE_OUTER_BOUND('',#1788,.T.);
#1227=FACE_OUTER_BOUND('',#1789,.T.);
#1228=FACE_OUTER_BOUND('',#1790,.T.);
#1229=FACE_OUTER_BOUND('',#1791,.T.);
#1230=FACE_OUTER_BOUND('',#1793,.T.);
#1231=FACE_OUTER_BOUND('',#1794,.T.);
#1232=FACE_OUTER_BOUND('',#1796,.T.);
#1233=FACE_OUTER_BOUND('',#1798,.T.);
#1234=FACE_OUTER_BOUND('',#1799,.T.);
#1235=FACE_OUTER_BOUND('',#1801,.T.);
#1236=FACE_OUTER_BOUND('',#1803,.T.);
#1237=FACE_OUTER_BOUND('',#1804,.T.);
#1238=FACE_OUTER_BOUND('',#1806,.T.);
#1239=FACE_OUTER_BOUND('',#1808,.T.);
#1240=FACE_OUTER_BOUND('',#1809,.T.);
#1241=FACE_OUTER_BOUND('',#1811,.T.);
#1242=FACE_OUTER_BOUND('',#1813,.T.);
#1243=FACE_OUTER_BOUND('',#1814,.T.);
#1244=FACE_OUTER_BOUND('',#1816,.T.);
#1245=FACE_OUTER_BOUND('',#1817,.T.);
#1246=FACE_OUTER_BOUND('',#1818,.T.);
#1247=FACE_OUTER_BOUND('',#1819,.T.);
#1248=FACE_OUTER_BOUND('',#1820,.T.);
#1249=FACE_OUTER_BOUND('',#1821,.T.);
#1250=FACE_OUTER_BOUND('',#1822,.T.);
#1251=FACE_OUTER_BOUND('',#1823,.T.);
#1252=FACE_OUTER_BOUND('',#1824,.T.);
#1253=FACE_OUTER_BOUND('',#1825,.T.);
#1254=FACE_OUTER_BOUND('',#1826,.T.);
#1255=FACE_OUTER_BOUND('',#1827,.T.);
#1256=FACE_OUTER_BOUND('',#1828,.T.);
#1257=FACE_OUTER_BOUND('',#1829,.T.);
#1258=FACE_OUTER_BOUND('',#1830,.T.);
#1259=FACE_OUTER_BOUND('',#1831,.T.);
#1260=FACE_OUTER_BOUND('',#1832,.T.);
#1261=FACE_OUTER_BOUND('',#1833,.T.);
#1262=FACE_OUTER_BOUND('',#1834,.T.);
#1263=FACE_OUTER_BOUND('',#1835,.T.);
#1264=FACE_OUTER_BOUND('',#1836,.T.);
#1265=FACE_OUTER_BOUND('',#1837,.T.);
#1266=FACE_OUTER_BOUND('',#1838,.T.);
#1267=FACE_OUTER_BOUND('',#1839,.T.);
#1268=FACE_OUTER_BOUND('',#1840,.T.);
#1269=FACE_OUTER_BOUND('',#1841,.T.);
#1270=FACE_OUTER_BOUND('',#1842,.T.);
#1271=FACE_OUTER_BOUND('',#1843,.T.);
#1272=FACE_OUTER_BOUND('',#1844,.T.);
#1273=FACE_OUTER_BOUND('',#1845,.T.);
#1274=FACE_OUTER_BOUND('',#1846,.T.);
#1275=FACE_OUTER_BOUND('',#1847,.T.);
#1276=FACE_OUTER_BOUND('',#1848,.T.);
#1277=FACE_OUTER_BOUND('',#1849,.T.);
#1278=FACE_OUTER_BOUND('',#1850,.T.);
#1279=FACE_OUTER_BOUND('',#1851,.T.);
#1280=FACE_OUTER_BOUND('',#1852,.T.);
#1281=FACE_OUTER_BOUND('',#1853,.T.);
#1282=FACE_OUTER_BOUND('',#1854,.T.);
#1283=FACE_OUTER_BOUND('',#1855,.T.);
#1284=FACE_OUTER_BOUND('',#1856,.T.);
#1285=FACE_OUTER_BOUND('',#1857,.T.);
#1286=FACE_OUTER_BOUND('',#1858,.T.);
#1287=FACE_OUTER_BOUND('',#1859,.T.);
#1288=FACE_OUTER_BOUND('',#1860,.T.);
#1289=FACE_OUTER_BOUND('',#1861,.T.);
#1290=FACE_OUTER_BOUND('',#1862,.T.);
#1291=FACE_OUTER_BOUND('',#1863,.T.);
#1292=FACE_OUTER_BOUND('',#1864,.T.);
#1293=FACE_OUTER_BOUND('',#1865,.T.);
#1294=FACE_OUTER_BOUND('',#1866,.T.);
#1295=FACE_OUTER_BOUND('',#1867,.T.);
#1296=FACE_OUTER_BOUND('',#1868,.T.);
#1297=FACE_OUTER_BOUND('',#1869,.T.);
#1298=FACE_OUTER_BOUND('',#1870,.T.);
#1299=FACE_OUTER_BOUND('',#1871,.T.);
#1300=FACE_OUTER_BOUND('',#1872,.T.);
#1301=FACE_OUTER_BOUND('',#1873,.T.);
#1302=FACE_OUTER_BOUND('',#1874,.T.);
#1303=FACE_OUTER_BOUND('',#1875,.T.);
#1304=FACE_OUTER_BOUND('',#1876,.T.);
#1305=FACE_OUTER_BOUND('',#1877,.T.);
#1306=FACE_OUTER_BOUND('',#1878,.T.);
#1307=FACE_OUTER_BOUND('',#1879,.T.);
#1308=FACE_OUTER_BOUND('',#1880,.T.);
#1309=FACE_OUTER_BOUND('',#1881,.T.);
#1310=FACE_OUTER_BOUND('',#1882,.T.);
#1311=FACE_OUTER_BOUND('',#1883,.T.);
#1312=FACE_OUTER_BOUND('',#1884,.T.);
#1313=FACE_OUTER_BOUND('',#1885,.T.);
#1314=FACE_OUTER_BOUND('',#1886,.T.);
#1315=FACE_OUTER_BOUND('',#1887,.T.);
#1316=FACE_OUTER_BOUND('',#1888,.T.);
#1317=FACE_OUTER_BOUND('',#1889,.T.);
#1318=FACE_OUTER_BOUND('',#1890,.T.);
#1319=FACE_OUTER_BOUND('',#1891,.T.);
#1320=FACE_OUTER_BOUND('',#1892,.T.);
#1321=FACE_OUTER_BOUND('',#1893,.T.);
#1322=FACE_OUTER_BOUND('',#1895,.T.);
#1323=FACE_OUTER_BOUND('',#1896,.T.);
#1324=FACE_OUTER_BOUND('',#1899,.T.);
#1325=FACE_OUTER_BOUND('',#1900,.T.);
#1326=FACE_OUTER_BOUND('',#1901,.T.);
#1327=FACE_OUTER_BOUND('',#1902,.T.);
#1328=FACE_OUTER_BOUND('',#1903,.T.);
#1329=FACE_OUTER_BOUND('',#1904,.T.);
#1330=FACE_OUTER_BOUND('',#1905,.T.);
#1331=FACE_OUTER_BOUND('',#1906,.T.);
#1332=FACE_OUTER_BOUND('',#1907,.T.);
#1333=FACE_OUTER_BOUND('',#1908,.T.);
#1334=FACE_OUTER_BOUND('',#1909,.T.);
#1335=FACE_OUTER_BOUND('',#1910,.T.);
#1336=FACE_OUTER_BOUND('',#1911,.T.);
#1337=FACE_OUTER_BOUND('',#1912,.T.);
#1338=FACE_OUTER_BOUND('',#1913,.T.);
#1339=FACE_OUTER_BOUND('',#1914,.T.);
#1340=FACE_OUTER_BOUND('',#1915,.T.);
#1341=FACE_OUTER_BOUND('',#1916,.T.);
#1342=FACE_OUTER_BOUND('',#1918,.T.);
#1343=FACE_OUTER_BOUND('',#1919,.T.);
#1344=FACE_OUTER_BOUND('',#1920,.T.);
#1345=FACE_OUTER_BOUND('',#1921,.T.);
#1346=FACE_OUTER_BOUND('',#1922,.T.);
#1347=FACE_OUTER_BOUND('',#1923,.T.);
#1348=FACE_OUTER_BOUND('',#1924,.T.);
#1349=FACE_OUTER_BOUND('',#1925,.T.);
#1350=FACE_OUTER_BOUND('',#1926,.T.);
#1351=FACE_OUTER_BOUND('',#1927,.T.);
#1352=FACE_OUTER_BOUND('',#1928,.T.);
#1353=FACE_OUTER_BOUND('',#1929,.T.);
#1354=FACE_OUTER_BOUND('',#1930,.T.);
#1355=FACE_OUTER_BOUND('',#1933,.T.);
#1356=FACE_OUTER_BOUND('',#1934,.T.);
#1357=FACE_OUTER_BOUND('',#1935,.T.);
#1358=FACE_OUTER_BOUND('',#1936,.T.);
#1359=FACE_OUTER_BOUND('',#1937,.T.);
#1360=FACE_OUTER_BOUND('',#1938,.T.);
#1361=FACE_OUTER_BOUND('',#1940,.T.);
#1362=FACE_OUTER_BOUND('',#1941,.T.);
#1363=FACE_OUTER_BOUND('',#1942,.T.);
#1364=FACE_OUTER_BOUND('',#1943,.T.);
#1365=FACE_OUTER_BOUND('',#1944,.T.);
#1366=FACE_OUTER_BOUND('',#1945,.T.);
#1367=FACE_OUTER_BOUND('',#1946,.T.);
#1368=FACE_OUTER_BOUND('',#1947,.T.);
#1369=FACE_OUTER_BOUND('',#1948,.T.);
#1370=FACE_OUTER_BOUND('',#1949,.T.);
#1371=FACE_OUTER_BOUND('',#1950,.T.);
#1372=FACE_OUTER_BOUND('',#1951,.T.);
#1373=FACE_OUTER_BOUND('',#1952,.T.);
#1374=FACE_OUTER_BOUND('',#1953,.T.);
#1375=FACE_OUTER_BOUND('',#1954,.T.);
#1376=FACE_OUTER_BOUND('',#1955,.T.);
#1377=FACE_OUTER_BOUND('',#1956,.T.);
#1378=FACE_OUTER_BOUND('',#1957,.T.);
#1379=FACE_OUTER_BOUND('',#1958,.T.);
#1380=FACE_OUTER_BOUND('',#1959,.T.);
#1381=FACE_OUTER_BOUND('',#1960,.T.);
#1382=FACE_OUTER_BOUND('',#1961,.T.);
#1383=FACE_OUTER_BOUND('',#1962,.T.);
#1384=FACE_OUTER_BOUND('',#1963,.T.);
#1385=FACE_OUTER_BOUND('',#1964,.T.);
#1386=FACE_OUTER_BOUND('',#1965,.T.);
#1387=FACE_OUTER_BOUND('',#1966,.T.);
#1388=FACE_OUTER_BOUND('',#1967,.T.);
#1389=FACE_OUTER_BOUND('',#1968,.T.);
#1390=FACE_OUTER_BOUND('',#1969,.T.);
#1391=FACE_OUTER_BOUND('',#1970,.T.);
#1392=FACE_OUTER_BOUND('',#1971,.T.);
#1393=FACE_OUTER_BOUND('',#1972,.T.);
#1394=FACE_OUTER_BOUND('',#1973,.T.);
#1395=FACE_OUTER_BOUND('',#1974,.T.);
#1396=FACE_OUTER_BOUND('',#1975,.T.);
#1397=FACE_OUTER_BOUND('',#1976,.T.);
#1398=FACE_OUTER_BOUND('',#1978,.T.);
#1399=FACE_OUTER_BOUND('',#1979,.T.);
#1400=FACE_OUTER_BOUND('',#1981,.T.);
#1401=FACE_OUTER_BOUND('',#1982,.T.);
#1402=FACE_OUTER_BOUND('',#1983,.T.);
#1403=FACE_OUTER_BOUND('',#1984,.T.);
#1404=FACE_OUTER_BOUND('',#1985,.T.);
#1405=FACE_OUTER_BOUND('',#1986,.T.);
#1406=FACE_OUTER_BOUND('',#1987,.T.);
#1407=FACE_OUTER_BOUND('',#1988,.T.);
#1408=FACE_OUTER_BOUND('',#1989,.T.);
#1409=FACE_OUTER_BOUND('',#1991,.T.);
#1410=FACE_OUTER_BOUND('',#1992,.T.);
#1411=FACE_OUTER_BOUND('',#1993,.T.);
#1412=FACE_OUTER_BOUND('',#1994,.T.);
#1413=FACE_OUTER_BOUND('',#1996,.T.);
#1414=FACE_OUTER_BOUND('',#1997,.T.);
#1415=FACE_OUTER_BOUND('',#1999,.T.);
#1416=FACE_OUTER_BOUND('',#2000,.T.);
#1417=FACE_OUTER_BOUND('',#2001,.T.);
#1418=FACE_OUTER_BOUND('',#2002,.T.);
#1419=FACE_OUTER_BOUND('',#2003,.T.);
#1420=FACE_OUTER_BOUND('',#2004,.T.);
#1421=FACE_OUTER_BOUND('',#2005,.T.);
#1422=FACE_OUTER_BOUND('',#2006,.T.);
#1423=FACE_OUTER_BOUND('',#2007,.T.);
#1424=FACE_OUTER_BOUND('',#2008,.T.);
#1425=FACE_OUTER_BOUND('',#2009,.T.);
#1426=FACE_OUTER_BOUND('',#2010,.T.);
#1427=FACE_OUTER_BOUND('',#2011,.T.);
#1428=FACE_OUTER_BOUND('',#2012,.T.);
#1429=FACE_OUTER_BOUND('',#2013,.T.);
#1430=FACE_OUTER_BOUND('',#2014,.T.);
#1431=FACE_OUTER_BOUND('',#2015,.T.);
#1432=FACE_OUTER_BOUND('',#2017,.T.);
#1433=FACE_OUTER_BOUND('',#2018,.T.);
#1434=FACE_OUTER_BOUND('',#2019,.T.);
#1435=FACE_OUTER_BOUND('',#2021,.T.);
#1436=FACE_OUTER_BOUND('',#2022,.T.);
#1437=FACE_OUTER_BOUND('',#2024,.T.);
#1438=FACE_OUTER_BOUND('',#2025,.T.);
#1439=FACE_OUTER_BOUND('',#2026,.T.);
#1440=FACE_OUTER_BOUND('',#2027,.T.);
#1441=FACE_OUTER_BOUND('',#2028,.T.);
#1442=FACE_OUTER_BOUND('',#2029,.T.);
#1443=FACE_OUTER_BOUND('',#2030,.T.);
#1444=FACE_OUTER_BOUND('',#2032,.T.);
#1445=FACE_OUTER_BOUND('',#2033,.T.);
#1446=FACE_OUTER_BOUND('',#2034,.T.);
#1447=FACE_OUTER_BOUND('',#2035,.T.);
#1448=FACE_OUTER_BOUND('',#2036,.T.);
#1449=FACE_OUTER_BOUND('',#2038,.T.);
#1450=FACE_OUTER_BOUND('',#2039,.T.);
#1451=FACE_OUTER_BOUND('',#2040,.T.);
#1452=FACE_OUTER_BOUND('',#2041,.T.);
#1453=FACE_OUTER_BOUND('',#2042,.T.);
#1454=FACE_OUTER_BOUND('',#2043,.T.);
#1455=FACE_OUTER_BOUND('',#2044,.T.);
#1456=FACE_OUTER_BOUND('',#2045,.T.);
#1457=FACE_OUTER_BOUND('',#2046,.T.);
#1458=FACE_OUTER_BOUND('',#2047,.T.);
#1459=FACE_OUTER_BOUND('',#2048,.T.);
#1460=FACE_OUTER_BOUND('',#2049,.T.);
#1461=FACE_OUTER_BOUND('',#2050,.T.);
#1462=FACE_OUTER_BOUND('',#2051,.T.);
#1463=FACE_OUTER_BOUND('',#2052,.T.);
#1464=FACE_OUTER_BOUND('',#2053,.T.);
#1465=FACE_OUTER_BOUND('',#2054,.T.);
#1466=FACE_OUTER_BOUND('',#2056,.T.);
#1467=FACE_OUTER_BOUND('',#2057,.T.);
#1468=FACE_OUTER_BOUND('',#2058,.T.);
#1469=FACE_OUTER_BOUND('',#2059,.T.);
#1470=FACE_OUTER_BOUND('',#2060,.T.);
#1471=FACE_OUTER_BOUND('',#2061,.T.);
#1472=FACE_OUTER_BOUND('',#2062,.T.);
#1473=FACE_OUTER_BOUND('',#2064,.T.);
#1474=FACE_OUTER_BOUND('',#2065,.T.);
#1475=FACE_OUTER_BOUND('',#2066,.T.);
#1476=FACE_OUTER_BOUND('',#2067,.T.);
#1477=FACE_OUTER_BOUND('',#2068,.T.);
#1478=FACE_OUTER_BOUND('',#2069,.T.);
#1479=FACE_OUTER_BOUND('',#2070,.T.);
#1480=FACE_OUTER_BOUND('',#2071,.T.);
#1481=FACE_OUTER_BOUND('',#2072,.T.);
#1482=FACE_OUTER_BOUND('',#2073,.T.);
#1483=FACE_OUTER_BOUND('',#2074,.T.);
#1484=FACE_OUTER_BOUND('',#2075,.T.);
#1485=FACE_OUTER_BOUND('',#2076,.T.);
#1486=FACE_OUTER_BOUND('',#2077,.T.);
#1487=FACE_OUTER_BOUND('',#2078,.T.);
#1488=FACE_OUTER_BOUND('',#2079,.T.);
#1489=FACE_OUTER_BOUND('',#2080,.T.);
#1490=FACE_OUTER_BOUND('',#2081,.T.);
#1491=FACE_OUTER_BOUND('',#2082,.T.);
#1492=FACE_OUTER_BOUND('',#2083,.T.);
#1493=FACE_OUTER_BOUND('',#2084,.T.);
#1494=FACE_OUTER_BOUND('',#2085,.T.);
#1495=FACE_OUTER_BOUND('',#2086,.T.);
#1496=FACE_OUTER_BOUND('',#2087,.T.);
#1497=FACE_OUTER_BOUND('',#2088,.T.);
#1498=FACE_OUTER_BOUND('',#2089,.T.);
#1499=FACE_OUTER_BOUND('',#2090,.T.);
#1500=FACE_OUTER_BOUND('',#2091,.T.);
#1501=FACE_OUTER_BOUND('',#2092,.T.);
#1502=FACE_OUTER_BOUND('',#2093,.T.);
#1503=FACE_OUTER_BOUND('',#2094,.T.);
#1504=FACE_OUTER_BOUND('',#2095,.T.);
#1505=FACE_OUTER_BOUND('',#2096,.T.);
#1506=FACE_OUTER_BOUND('',#2097,.T.);
#1507=FACE_OUTER_BOUND('',#2098,.T.);
#1508=FACE_OUTER_BOUND('',#2099,.T.);
#1509=FACE_OUTER_BOUND('',#2100,.T.);
#1510=FACE_OUTER_BOUND('',#2103,.T.);
#1511=FACE_OUTER_BOUND('',#2104,.T.);
#1512=FACE_OUTER_BOUND('',#2105,.T.);
#1513=FACE_OUTER_BOUND('',#2106,.T.);
#1514=FACE_OUTER_BOUND('',#2107,.T.);
#1515=FACE_OUTER_BOUND('',#2108,.T.);
#1516=FACE_OUTER_BOUND('',#2109,.T.);
#1517=FACE_OUTER_BOUND('',#2110,.T.);
#1518=FACE_OUTER_BOUND('',#2111,.T.);
#1519=FACE_OUTER_BOUND('',#2112,.T.);
#1520=FACE_OUTER_BOUND('',#2113,.T.);
#1521=FACE_OUTER_BOUND('',#2114,.T.);
#1522=FACE_OUTER_BOUND('',#2115,.T.);
#1523=FACE_OUTER_BOUND('',#2116,.T.);
#1524=FACE_OUTER_BOUND('',#2117,.T.);
#1525=FACE_OUTER_BOUND('',#2118,.T.);
#1526=FACE_OUTER_BOUND('',#2119,.T.);
#1527=FACE_OUTER_BOUND('',#2120,.T.);
#1528=FACE_OUTER_BOUND('',#2121,.T.);
#1529=FACE_OUTER_BOUND('',#2122,.T.);
#1530=FACE_OUTER_BOUND('',#2123,.T.);
#1531=FACE_OUTER_BOUND('',#2124,.T.);
#1532=FACE_OUTER_BOUND('',#2125,.T.);
#1533=FACE_OUTER_BOUND('',#2126,.T.);
#1534=FACE_OUTER_BOUND('',#2127,.T.);
#1535=FACE_OUTER_BOUND('',#2128,.T.);
#1536=FACE_OUTER_BOUND('',#2129,.T.);
#1537=FACE_OUTER_BOUND('',#2130,.T.);
#1538=FACE_OUTER_BOUND('',#2131,.T.);
#1539=FACE_OUTER_BOUND('',#2132,.T.);
#1540=FACE_OUTER_BOUND('',#2133,.T.);
#1541=FACE_OUTER_BOUND('',#2134,.T.);
#1542=FACE_OUTER_BOUND('',#2135,.T.);
#1543=FACE_OUTER_BOUND('',#2136,.T.);
#1544=FACE_OUTER_BOUND('',#2138,.T.);
#1545=FACE_OUTER_BOUND('',#2140,.T.);
#1546=FACE_OUTER_BOUND('',#2141,.T.);
#1547=FACE_OUTER_BOUND('',#2142,.T.);
#1548=FACE_OUTER_BOUND('',#2143,.T.);
#1549=FACE_OUTER_BOUND('',#2144,.T.);
#1550=FACE_OUTER_BOUND('',#2145,.T.);
#1551=FACE_OUTER_BOUND('',#2146,.T.);
#1552=FACE_OUTER_BOUND('',#2147,.T.);
#1553=FACE_OUTER_BOUND('',#2148,.T.);
#1554=FACE_OUTER_BOUND('',#2149,.T.);
#1555=FACE_OUTER_BOUND('',#2150,.T.);
#1556=FACE_OUTER_BOUND('',#2151,.T.);
#1557=FACE_OUTER_BOUND('',#2152,.T.);
#1558=FACE_OUTER_BOUND('',#2153,.T.);
#1559=FACE_OUTER_BOUND('',#2154,.T.);
#1560=FACE_OUTER_BOUND('',#2155,.T.);
#1561=FACE_OUTER_BOUND('',#2156,.T.);
#1562=FACE_OUTER_BOUND('',#2157,.T.);
#1563=FACE_OUTER_BOUND('',#2158,.T.);
#1564=FACE_OUTER_BOUND('',#2159,.T.);
#1565=FACE_OUTER_BOUND('',#2160,.T.);
#1566=FACE_OUTER_BOUND('',#2161,.T.);
#1567=FACE_OUTER_BOUND('',#2162,.T.);
#1568=FACE_OUTER_BOUND('',#2163,.T.);
#1569=FACE_OUTER_BOUND('',#2164,.T.);
#1570=FACE_OUTER_BOUND('',#2165,.T.);
#1571=FACE_OUTER_BOUND('',#2166,.T.);
#1572=FACE_OUTER_BOUND('',#2167,.T.);
#1573=FACE_OUTER_BOUND('',#2168,.T.);
#1574=FACE_OUTER_BOUND('',#2169,.T.);
#1575=FACE_OUTER_BOUND('',#2170,.T.);
#1576=FACE_OUTER_BOUND('',#2171,.T.);
#1577=FACE_OUTER_BOUND('',#2172,.T.);
#1578=FACE_OUTER_BOUND('',#2173,.T.);
#1579=FACE_OUTER_BOUND('',#2174,.T.);
#1580=FACE_OUTER_BOUND('',#2175,.T.);
#1581=FACE_OUTER_BOUND('',#2176,.T.);
#1582=FACE_OUTER_BOUND('',#2177,.T.);
#1583=FACE_OUTER_BOUND('',#2178,.T.);
#1584=FACE_OUTER_BOUND('',#2179,.T.);
#1585=FACE_OUTER_BOUND('',#2180,.T.);
#1586=FACE_OUTER_BOUND('',#2181,.T.);
#1587=FACE_OUTER_BOUND('',#2182,.T.);
#1588=FACE_OUTER_BOUND('',#2183,.T.);
#1589=FACE_OUTER_BOUND('',#2184,.T.);
#1590=FACE_OUTER_BOUND('',#2185,.T.);
#1591=FACE_OUTER_BOUND('',#2186,.T.);
#1592=FACE_OUTER_BOUND('',#2187,.T.);
#1593=FACE_OUTER_BOUND('',#2188,.T.);
#1594=FACE_OUTER_BOUND('',#2189,.T.);
#1595=FACE_OUTER_BOUND('',#2190,.T.);
#1596=FACE_OUTER_BOUND('',#2191,.T.);
#1597=FACE_OUTER_BOUND('',#2192,.T.);
#1598=FACE_OUTER_BOUND('',#2193,.T.);
#1599=FACE_OUTER_BOUND('',#2194,.T.);
#1600=FACE_OUTER_BOUND('',#2195,.T.);
#1601=FACE_OUTER_BOUND('',#2196,.T.);
#1602=FACE_OUTER_BOUND('',#2198,.T.);
#1603=FACE_OUTER_BOUND('',#2199,.T.);
#1604=FACE_OUTER_BOUND('',#2200,.T.);
#1605=FACE_OUTER_BOUND('',#2201,.T.);
#1606=FACE_OUTER_BOUND('',#2202,.T.);
#1607=FACE_OUTER_BOUND('',#2204,.T.);
#1608=FACE_OUTER_BOUND('',#2206,.T.);
#1609=FACE_OUTER_BOUND('',#2207,.T.);
#1610=FACE_OUTER_BOUND('',#2208,.T.);
#1611=FACE_OUTER_BOUND('',#2209,.T.);
#1612=FACE_OUTER_BOUND('',#2210,.T.);
#1613=FACE_OUTER_BOUND('',#2211,.T.);
#1614=FACE_OUTER_BOUND('',#2212,.T.);
#1615=FACE_OUTER_BOUND('',#2213,.T.);
#1616=FACE_OUTER_BOUND('',#2214,.T.);
#1617=FACE_OUTER_BOUND('',#2215,.T.);
#1618=FACE_OUTER_BOUND('',#2216,.T.);
#1619=FACE_OUTER_BOUND('',#2217,.T.);
#1620=FACE_OUTER_BOUND('',#2218,.T.);
#1621=FACE_OUTER_BOUND('',#2219,.T.);
#1622=FACE_OUTER_BOUND('',#2220,.T.);
#1623=FACE_OUTER_BOUND('',#2221,.T.);
#1624=FACE_OUTER_BOUND('',#2222,.T.);
#1625=FACE_OUTER_BOUND('',#2223,.T.);
#1626=FACE_OUTER_BOUND('',#2224,.T.);
#1627=FACE_OUTER_BOUND('',#2225,.T.);
#1628=FACE_OUTER_BOUND('',#2226,.T.);
#1629=FACE_OUTER_BOUND('',#2227,.T.);
#1630=FACE_OUTER_BOUND('',#2228,.T.);
#1631=FACE_OUTER_BOUND('',#2229,.T.);
#1632=FACE_OUTER_BOUND('',#2230,.T.);
#1633=FACE_OUTER_BOUND('',#2231,.T.);
#1634=FACE_OUTER_BOUND('',#2232,.T.);
#1635=FACE_OUTER_BOUND('',#2233,.T.);
#1636=FACE_OUTER_BOUND('',#2234,.T.);
#1637=FACE_OUTER_BOUND('',#2236,.T.);
#1638=FACE_OUTER_BOUND('',#2237,.T.);
#1639=FACE_OUTER_BOUND('',#2239,.T.);
#1640=FACE_OUTER_BOUND('',#2240,.T.);
#1641=FACE_OUTER_BOUND('',#2241,.T.);
#1642=FACE_OUTER_BOUND('',#2242,.T.);
#1643=EDGE_LOOP('',(#6226,#6227,#6228,#6229));
#1644=EDGE_LOOP('',(#6230));
#1645=EDGE_LOOP('',(#6231));
#1646=EDGE_LOOP('',(#6232));
#1647=EDGE_LOOP('',(#6233,#6234,#6235,#6236,#6237));
#1648=EDGE_LOOP('',(#6238,#6239,#6240,#6241,#6242,#6243));
#1649=EDGE_LOOP('',(#6244,#6245,#6246,#6247,#6248));
#1650=EDGE_LOOP('',(#6249));
#1651=EDGE_LOOP('',(#6250));
#1652=EDGE_LOOP('',(#6251,#6252,#6253,#6254,#6255));
#1653=EDGE_LOOP('',(#6256,#6257,#6258,#6259,#6260,#6261));
#1654=EDGE_LOOP('',(#6262,#6263,#6264,#6265,#6266));
#1655=EDGE_LOOP('',(#6267));
#1656=EDGE_LOOP('',(#6268,#6269,#6270,#6271));
#1657=EDGE_LOOP('',(#6272));
#1658=EDGE_LOOP('',(#6273));
#1659=EDGE_LOOP('',(#6274,#6275,#6276,#6277,#6278,#6279,#6280,#6281,#6282,
#6283,#6284,#6285,#6286,#6287,#6288,#6289,#6290,#6291,#6292,#6293));
#1660=EDGE_LOOP('',(#6294,#6295,#6296,#6297));
#1661=EDGE_LOOP('',(#6298,#6299,#6300,#6301,#6302,#6303,#6304,#6305,#6306,
#6307,#6308,#6309,#6310,#6311,#6312,#6313,#6314,#6315,#6316,#6317,#6318,
#6319,#6320,#6321,#6322,#6323,#6324,#6325,#6326,#6327,#6328,#6329,#6330,
#6331,#6332,#6333,#6334,#6335,#6336,#6337,#6338,#6339,#6340,#6341));
#1662=EDGE_LOOP('',(#6342));
#1663=EDGE_LOOP('',(#6343));
#1664=EDGE_LOOP('',(#6344,#6345,#6346,#6347));
#1665=EDGE_LOOP('',(#6348,#6349,#6350,#6351));
#1666=EDGE_LOOP('',(#6352,#6353,#6354,#6355));
#1667=EDGE_LOOP('',(#6356,#6357,#6358,#6359));
#1668=EDGE_LOOP('',(#6360,#6361,#6362,#6363));
#1669=EDGE_LOOP('',(#6364,#6365,#6366,#6367));
#1670=EDGE_LOOP('',(#6368,#6369,#6370,#6371));
#1671=EDGE_LOOP('',(#6372,#6373,#6374,#6375,#6376));
#1672=EDGE_LOOP('',(#6377,#6378,#6379,#6380));
#1673=EDGE_LOOP('',(#6381,#6382,#6383,#6384));
#1674=EDGE_LOOP('',(#6385,#6386,#6387,#6388));
#1675=EDGE_LOOP('',(#6389,#6390,#6391,#6392));
#1676=EDGE_LOOP('',(#6393,#6394,#6395,#6396));
#1677=EDGE_LOOP('',(#6397,#6398,#6399,#6400));
#1678=EDGE_LOOP('',(#6401,#6402,#6403,#6404));
#1679=EDGE_LOOP('',(#6405,#6406,#6407,#6408));
#1680=EDGE_LOOP('',(#6409,#6410,#6411,#6412,#6413));
#1681=EDGE_LOOP('',(#6414,#6415,#6416,#6417));
#1682=EDGE_LOOP('',(#6418,#6419,#6420,#6421));
#1683=EDGE_LOOP('',(#6422,#6423,#6424,#6425,#6426));
#1684=EDGE_LOOP('',(#6427,#6428,#6429,#6430));
#1685=EDGE_LOOP('',(#6431,#6432,#6433,#6434));
#1686=EDGE_LOOP('',(#6435,#6436,#6437,#6438,#6439));
#1687=EDGE_LOOP('',(#6440,#6441,#6442,#6443));
#1688=EDGE_LOOP('',(#6444,#6445,#6446,#6447,#6448));
#1689=EDGE_LOOP('',(#6449,#6450,#6451,#6452));
#1690=EDGE_LOOP('',(#6453,#6454,#6455,#6456,#6457));
#1691=EDGE_LOOP('',(#6458,#6459,#6460,#6461,#6462));
#1692=EDGE_LOOP('',(#6463,#6464,#6465,#6466));
#1693=EDGE_LOOP('',(#6467,#6468,#6469,#6470,#6471));
#1694=EDGE_LOOP('',(#6472,#6473,#6474,#6475));
#1695=EDGE_LOOP('',(#6476,#6477,#6478,#6479));
#1696=EDGE_LOOP('',(#6480,#6481,#6482,#6483,#6484));
#1697=EDGE_LOOP('',(#6485,#6486,#6487,#6488,#6489));
#1698=EDGE_LOOP('',(#6490,#6491,#6492,#6493));
#1699=EDGE_LOOP('',(#6494,#6495,#6496,#6497));
#1700=EDGE_LOOP('',(#6498,#6499,#6500,#6501));
#1701=EDGE_LOOP('',(#6502,#6503,#6504,#6505));
#1702=EDGE_LOOP('',(#6506,#6507,#6508,#6509));
#1703=EDGE_LOOP('',(#6510,#6511,#6512,#6513));
#1704=EDGE_LOOP('',(#6514,#6515,#6516,#6517));
#1705=EDGE_LOOP('',(#6518,#6519,#6520,#6521));
#1706=EDGE_LOOP('',(#6522,#6523,#6524,#6525));
#1707=EDGE_LOOP('',(#6526,#6527,#6528,#6529));
#1708=EDGE_LOOP('',(#6530,#6531,#6532,#6533));
#1709=EDGE_LOOP('',(#6534,#6535,#6536,#6537));
#1710=EDGE_LOOP('',(#6538,#6539,#6540,#6541));
#1711=EDGE_LOOP('',(#6542,#6543,#6544,#6545));
#1712=EDGE_LOOP('',(#6546,#6547,#6548,#6549));
#1713=EDGE_LOOP('',(#6550,#6551,#6552,#6553));
#1714=EDGE_LOOP('',(#6554,#6555,#6556,#6557));
#1715=EDGE_LOOP('',(#6558,#6559,#6560,#6561));
#1716=EDGE_LOOP('',(#6562,#6563,#6564,#6565));
#1717=EDGE_LOOP('',(#6566,#6567,#6568,#6569));
#1718=EDGE_LOOP('',(#6570,#6571,#6572,#6573));
#1719=EDGE_LOOP('',(#6574,#6575,#6576,#6577));
#1720=EDGE_LOOP('',(#6578,#6579,#6580,#6581));
#1721=EDGE_LOOP('',(#6582,#6583,#6584,#6585,#6586,#6587,#6588,#6589,#6590,
#6591,#6592,#6593,#6594,#6595,#6596,#6597,#6598,#6599,#6600,#6601,#6602,
#6603,#6604,#6605,#6606,#6607,#6608,#6609,#6610,#6611,#6612,#6613));
#1722=EDGE_LOOP('',(#6614,#6615,#6616,#6617,#6618,#6619,#6620,#6621,#6622,
#6623,#6624,#6625,#6626,#6627,#6628,#6629,#6630,#6631,#6632,#6633,#6634,
#6635,#6636,#6637,#6638,#6639,#6640,#6641,#6642,#6643,#6644));
#1723=EDGE_LOOP('',(#6645));
#1724=EDGE_LOOP('',(#6646,#6647,#6648,#6649));
#1725=EDGE_LOOP('',(#6650));
#1726=EDGE_LOOP('',(#6651));
#1727=EDGE_LOOP('',(#6652,#6653,#6654,#6655,#6656));
#1728=EDGE_LOOP('',(#6657,#6658,#6659,#6660));
#1729=EDGE_LOOP('',(#6661,#6662,#6663,#6664));
#1730=EDGE_LOOP('',(#6665));
#1731=EDGE_LOOP('',(#6666));
#1732=EDGE_LOOP('',(#6667,#6668,#6669,#6670));
#1733=EDGE_LOOP('',(#6671,#6672,#6673,#6674,#6675,#6676));
#1734=EDGE_LOOP('',(#6677,#6678,#6679,#6680,#6681,#6682));
#1735=EDGE_LOOP('',(#6683,#6684,#6685,#6686));
#1736=EDGE_LOOP('',(#6687,#6688,#6689,#6690,#6691,#6692,#6693,#6694,#6695,
#6696,#6697,#6698,#6699,#6700,#6701,#6702,#6703,#6704,#6705,#6706,#6707,
#6708,#6709,#6710,#6711,#6712,#6713,#6714,#6715,#6716,#6717,#6718));
#1737=EDGE_LOOP('',(#6719,#6720,#6721,#6722,#6723,#6724,#6725,#6726,#6727,
#6728,#6729,#6730,#6731,#6732,#6733,#6734,#6735,#6736,#6737,#6738,#6739,
#6740,#6741,#6742,#6743,#6744,#6745,#6746,#6747,#6748,#6749));
#1738=EDGE_LOOP('',(#6750,#6751,#6752,#6753,#6754));
#1739=EDGE_LOOP('',(#6755));
#1740=EDGE_LOOP('',(#6756));
#1741=EDGE_LOOP('',(#6757));
#1742=EDGE_LOOP('',(#6758));
#1743=EDGE_LOOP('',(#6759));
#1744=EDGE_LOOP('',(#6760));
#1745=EDGE_LOOP('',(#6761));
#1746=EDGE_LOOP('',(#6762));
#1747=EDGE_LOOP('',(#6763));
#1748=EDGE_LOOP('',(#6764));
#1749=EDGE_LOOP('',(#6765));
#1750=EDGE_LOOP('',(#6766));
#1751=EDGE_LOOP('',(#6767));
#1752=EDGE_LOOP('',(#6768));
#1753=EDGE_LOOP('',(#6769));
#1754=EDGE_LOOP('',(#6770));
#1755=EDGE_LOOP('',(#6771));
#1756=EDGE_LOOP('',(#6772));
#1757=EDGE_LOOP('',(#6773));
#1758=EDGE_LOOP('',(#6774));
#1759=EDGE_LOOP('',(#6775));
#1760=EDGE_LOOP('',(#6776));
#1761=EDGE_LOOP('',(#6777));
#1762=EDGE_LOOP('',(#6778));
#1763=EDGE_LOOP('',(#6779));
#1764=EDGE_LOOP('',(#6780));
#1765=EDGE_LOOP('',(#6781));
#1766=EDGE_LOOP('',(#6782));
#1767=EDGE_LOOP('',(#6783));
#1768=EDGE_LOOP('',(#6784));
#1769=EDGE_LOOP('',(#6785,#6786,#6787,#6788));
#1770=EDGE_LOOP('',(#6789,#6790,#6791,#6792));
#1771=EDGE_LOOP('',(#6793,#6794,#6795,#6796));
#1772=EDGE_LOOP('',(#6797,#6798,#6799,#6800));
#1773=EDGE_LOOP('',(#6801,#6802,#6803,#6804));
#1774=EDGE_LOOP('',(#6805,#6806,#6807,#6808));
#1775=EDGE_LOOP('',(#6809,#6810,#6811,#6812));
#1776=EDGE_LOOP('',(#6813,#6814,#6815,#6816));
#1777=EDGE_LOOP('',(#6817,#6818,#6819,#6820));
#1778=EDGE_LOOP('',(#6821,#6822,#6823,#6824));
#1779=EDGE_LOOP('',(#6825,#6826,#6827,#6828));
#1780=EDGE_LOOP('',(#6829,#6830,#6831,#6832));
#1781=EDGE_LOOP('',(#6833,#6834,#6835,#6836));
#1782=EDGE_LOOP('',(#6837,#6838,#6839,#6840));
#1783=EDGE_LOOP('',(#6841,#6842,#6843,#6844));
#1784=EDGE_LOOP('',(#6845));
#1785=EDGE_LOOP('',(#6846,#6847,#6848,#6849));
#1786=EDGE_LOOP('',(#6850,#6851,#6852,#6853));
#1787=EDGE_LOOP('',(#6854,#6855,#6856,#6857));
#1788=EDGE_LOOP('',(#6858,#6859,#6860,#6861));
#1789=EDGE_LOOP('',(#6862,#6863,#6864,#6865));
#1790=EDGE_LOOP('',(#6866,#6867,#6868,#6869));
#1791=EDGE_LOOP('',(#6870));
#1792=EDGE_LOOP('',(#6871));
#1793=EDGE_LOOP('',(#6872,#6873,#6874,#6875));
#1794=EDGE_LOOP('',(#6876));
#1795=EDGE_LOOP('',(#6877));
#1796=EDGE_LOOP('',(#6878));
#1797=EDGE_LOOP('',(#6879));
#1798=EDGE_LOOP('',(#6880,#6881,#6882,#6883));
#1799=EDGE_LOOP('',(#6884));
#1800=EDGE_LOOP('',(#6885));
#1801=EDGE_LOOP('',(#6886));
#1802=EDGE_LOOP('',(#6887));
#1803=EDGE_LOOP('',(#6888,#6889,#6890,#6891));
#1804=EDGE_LOOP('',(#6892));
#1805=EDGE_LOOP('',(#6893));
#1806=EDGE_LOOP('',(#6894));
#1807=EDGE_LOOP('',(#6895));
#1808=EDGE_LOOP('',(#6896,#6897,#6898,#6899));
#1809=EDGE_LOOP('',(#6900));
#1810=EDGE_LOOP('',(#6901));
#1811=EDGE_LOOP('',(#6902));
#1812=EDGE_LOOP('',(#6903));
#1813=EDGE_LOOP('',(#6904,#6905,#6906,#6907));
#1814=EDGE_LOOP('',(#6908));
#1815=EDGE_LOOP('',(#6909));
#1816=EDGE_LOOP('',(#6910,#6911,#6912,#6913));
#1817=EDGE_LOOP('',(#6914,#6915,#6916,#6917));
#1818=EDGE_LOOP('',(#6918,#6919,#6920));
#1819=EDGE_LOOP('',(#6921,#6922,#6923,#6924));
#1820=EDGE_LOOP('',(#6925,#6926,#6927));
#1821=EDGE_LOOP('',(#6928,#6929,#6930,#6931,#6932,#6933));
#1822=EDGE_LOOP('',(#6934,#6935,#6936,#6937,#6938,#6939));
#1823=EDGE_LOOP('',(#6940,#6941,#6942,#6943,#6944,#6945));
#1824=EDGE_LOOP('',(#6946,#6947,#6948,#6949));
#1825=EDGE_LOOP('',(#6950,#6951,#6952,#6953));
#1826=EDGE_LOOP('',(#6954,#6955,#6956,#6957));
#1827=EDGE_LOOP('',(#6958,#6959,#6960,#6961));
#1828=EDGE_LOOP('',(#6962,#6963,#6964,#6965,#6966,#6967));
#1829=EDGE_LOOP('',(#6968,#6969,#6970,#6971,#6972,#6973));
#1830=EDGE_LOOP('',(#6974,#6975,#6976,#6977,#6978,#6979));
#1831=EDGE_LOOP('',(#6980,#6981,#6982,#6983,#6984,#6985,#6986,#6987,#6988,
#6989));
#1832=EDGE_LOOP('',(#6990,#6991,#6992,#6993,#6994,#6995,#6996,#6997));
#1833=EDGE_LOOP('',(#6998));
#1834=EDGE_LOOP('',(#6999,#7000,#7001,#7002,#7003));
#1835=EDGE_LOOP('',(#7004,#7005,#7006,#7007,#7008,#7009));
#1836=EDGE_LOOP('',(#7010,#7011,#7012,#7013,#7014));
#1837=EDGE_LOOP('',(#7015));
#1838=EDGE_LOOP('',(#7016,#7017,#7018,#7019,#7020));
#1839=EDGE_LOOP('',(#7021,#7022,#7023,#7024,#7025,#7026));
#1840=EDGE_LOOP('',(#7027,#7028,#7029,#7030,#7031));
#1841=EDGE_LOOP('',(#7032));
#1842=EDGE_LOOP('',(#7033));
#1843=EDGE_LOOP('',(#7034,#7035,#7036,#7037,#7038));
#1844=EDGE_LOOP('',(#7039,#7040,#7041,#7042,#7043,#7044));
#1845=EDGE_LOOP('',(#7045,#7046,#7047,#7048,#7049));
#1846=EDGE_LOOP('',(#7050));
#1847=EDGE_LOOP('',(#7051));
#1848=EDGE_LOOP('',(#7052,#7053,#7054,#7055,#7056,#7057));
#1849=EDGE_LOOP('',(#7058,#7059,#7060,#7061,#7062));
#1850=EDGE_LOOP('',(#7063,#7064,#7065,#7066,#7067));
#1851=EDGE_LOOP('',(#7068,#7069,#7070,#7071));
#1852=EDGE_LOOP('',(#7072,#7073,#7074,#7075));
#1853=EDGE_LOOP('',(#7076,#7077,#7078,#7079));
#1854=EDGE_LOOP('',(#7080,#7081,#7082,#7083,#7084));
#1855=EDGE_LOOP('',(#7085,#7086,#7087,#7088));
#1856=EDGE_LOOP('',(#7089,#7090,#7091,#7092,#7093));
#1857=EDGE_LOOP('',(#7094,#7095,#7096,#7097,#7098,#7099));
#1858=EDGE_LOOP('',(#7100,#7101,#7102,#7103));
#1859=EDGE_LOOP('',(#7104,#7105,#7106,#7107));
#1860=EDGE_LOOP('',(#7108,#7109,#7110,#7111));
#1861=EDGE_LOOP('',(#7112,#7113,#7114,#7115,#7116,#7117));
#1862=EDGE_LOOP('',(#7118,#7119,#7120,#7121));
#1863=EDGE_LOOP('',(#7122,#7123,#7124,#7125));
#1864=EDGE_LOOP('',(#7126,#7127,#7128,#7129));
#1865=EDGE_LOOP('',(#7130,#7131,#7132,#7133));
#1866=EDGE_LOOP('',(#7134,#7135,#7136,#7137,#7138));
#1867=EDGE_LOOP('',(#7139,#7140,#7141,#7142,#7143));
#1868=EDGE_LOOP('',(#7144,#7145,#7146,#7147));
#1869=EDGE_LOOP('',(#7148,#7149,#7150,#7151));
#1870=EDGE_LOOP('',(#7152,#7153,#7154,#7155));
#1871=EDGE_LOOP('',(#7156,#7157,#7158,#7159));
#1872=EDGE_LOOP('',(#7160,#7161,#7162,#7163));
#1873=EDGE_LOOP('',(#7164,#7165,#7166,#7167));
#1874=EDGE_LOOP('',(#7168,#7169,#7170,#7171));
#1875=EDGE_LOOP('',(#7172,#7173,#7174,#7175));
#1876=EDGE_LOOP('',(#7176,#7177,#7178,#7179));
#1877=EDGE_LOOP('',(#7180,#7181,#7182,#7183));
#1878=EDGE_LOOP('',(#7184,#7185,#7186,#7187));
#1879=EDGE_LOOP('',(#7188,#7189,#7190,#7191));
#1880=EDGE_LOOP('',(#7192,#7193,#7194,#7195));
#1881=EDGE_LOOP('',(#7196,#7197,#7198,#7199));
#1882=EDGE_LOOP('',(#7200,#7201,#7202,#7203));
#1883=EDGE_LOOP('',(#7204,#7205,#7206,#7207));
#1884=EDGE_LOOP('',(#7208,#7209,#7210,#7211));
#1885=EDGE_LOOP('',(#7212,#7213,#7214,#7215));
#1886=EDGE_LOOP('',(#7216,#7217,#7218,#7219));
#1887=EDGE_LOOP('',(#7220,#7221,#7222,#7223));
#1888=EDGE_LOOP('',(#7224,#7225,#7226,#7227));
#1889=EDGE_LOOP('',(#7228,#7229,#7230,#7231));
#1890=EDGE_LOOP('',(#7232,#7233,#7234,#7235));
#1891=EDGE_LOOP('',(#7236,#7237,#7238,#7239));
#1892=EDGE_LOOP('',(#7240,#7241,#7242,#7243));
#1893=EDGE_LOOP('',(#7244,#7245,#7246,#7247,#7248,#7249,#7250,#7251));
#1894=EDGE_LOOP('',(#7252));
#1895=EDGE_LOOP('',(#7253,#7254,#7255,#7256));
#1896=EDGE_LOOP('',(#7257,#7258,#7259,#7260,#7261,#7262,#7263));
#1897=EDGE_LOOP('',(#7264));
#1898=EDGE_LOOP('',(#7265));
#1899=EDGE_LOOP('',(#7266,#7267,#7268));
#1900=EDGE_LOOP('',(#7269,#7270,#7271));
#1901=EDGE_LOOP('',(#7272,#7273,#7274,#7275,#7276,#7277,#7278,#7279,#7280,
#7281,#7282));
#1902=EDGE_LOOP('',(#7283,#7284,#7285,#7286));
#1903=EDGE_LOOP('',(#7287,#7288,#7289,#7290));
#1904=EDGE_LOOP('',(#7291,#7292,#7293,#7294));
#1905=EDGE_LOOP('',(#7295,#7296,#7297,#7298,#7299,#7300,#7301,#7302,#7303,
#7304,#7305));
#1906=EDGE_LOOP('',(#7306,#7307,#7308,#7309));
#1907=EDGE_LOOP('',(#7310,#7311,#7312,#7313));
#1908=EDGE_LOOP('',(#7314,#7315,#7316,#7317,#7318));
#1909=EDGE_LOOP('',(#7319,#7320,#7321,#7322,#7323,#7324,#7325));
#1910=EDGE_LOOP('',(#7326,#7327,#7328,#7329,#7330,#7331));
#1911=EDGE_LOOP('',(#7332,#7333,#7334,#7335));
#1912=EDGE_LOOP('',(#7336,#7337,#7338,#7339));
#1913=EDGE_LOOP('',(#7340,#7341,#7342,#7343,#7344,#7345));
#1914=EDGE_LOOP('',(#7346,#7347,#7348,#7349));
#1915=EDGE_LOOP('',(#7350,#7351,#7352,#7353));
#1916=EDGE_LOOP('',(#7354,#7355,#7356,#7357,#7358,#7359,#7360,#7361));
#1917=EDGE_LOOP('',(#7362,#7363,#7364,#7365));
#1918=EDGE_LOOP('',(#7366,#7367,#7368,#7369,#7370,#7371));
#1919=EDGE_LOOP('',(#7372,#7373,#7374,#7375,#7376,#7377));
#1920=EDGE_LOOP('',(#7378,#7379,#7380,#7381));
#1921=EDGE_LOOP('',(#7382,#7383,#7384,#7385));
#1922=EDGE_LOOP('',(#7386,#7387,#7388,#7389,#7390,#7391));
#1923=EDGE_LOOP('',(#7392,#7393,#7394,#7395,#7396,#7397,#7398,#7399,#7400,
#7401,#7402,#7403,#7404,#7405,#7406,#7407,#7408,#7409,#7410,#7411,#7412,
#7413,#7414,#7415));
#1924=EDGE_LOOP('',(#7416,#7417,#7418,#7419));
#1925=EDGE_LOOP('',(#7420,#7421,#7422,#7423));
#1926=EDGE_LOOP('',(#7424,#7425,#7426));
#1927=EDGE_LOOP('',(#7427,#7428,#7429,#7430));
#1928=EDGE_LOOP('',(#7431,#7432,#7433));
#1929=EDGE_LOOP('',(#7434,#7435,#7436));
#1930=EDGE_LOOP('',(#7437,#7438,#7439,#7440));
#1931=EDGE_LOOP('',(#7441));
#1932=EDGE_LOOP('',(#7442));
#1933=EDGE_LOOP('',(#7443,#7444,#7445));
#1934=EDGE_LOOP('',(#7446,#7447,#7448,#7449));
#1935=EDGE_LOOP('',(#7450,#7451,#7452,#7453,#7454));
#1936=EDGE_LOOP('',(#7455,#7456,#7457,#7458,#7459,#7460,#7461,#7462,#7463,
#7464,#7465,#7466,#7467,#7468,#7469,#7470,#7471,#7472,#7473,#7474,#7475,
#7476,#7477,#7478,#7479,#7480,#7481,#7482,#7483,#7484,#7485,#7486,#7487,
#7488));
#1937=EDGE_LOOP('',(#7489,#7490,#7491,#7492,#7493,#7494,#7495,#7496,#7497,
#7498,#7499,#7500,#7501,#7502,#7503,#7504,#7505,#7506,#7507,#7508,#7509,
#7510,#7511,#7512,#7513,#7514,#7515,#7516,#7517,#7518,#7519,#7520));
#1938=EDGE_LOOP('',(#7521,#7522,#7523,#7524));
#1939=EDGE_LOOP('',(#7525,#7526,#7527,#7528,#7529,#7530,#7531,#7532,#7533,
#7534,#7535,#7536,#7537,#7538,#7539,#7540,#7541,#7542,#7543,#7544,#7545,
#7546,#7547,#7548,#7549));
#1940=EDGE_LOOP('',(#7550,#7551,#7552));
#1941=EDGE_LOOP('',(#7553,#7554,#7555));
#1942=EDGE_LOOP('',(#7556,#7557,#7558,#7559,#7560,#7561,#7562,#7563,#7564,
#7565,#7566,#7567,#7568,#7569,#7570,#7571,#7572,#7573,#7574,#7575,#7576,
#7577,#7578,#7579));
#1943=EDGE_LOOP('',(#7580,#7581,#7582,#7583,#7584,#7585,#7586,#7587,#7588,
#7589,#7590,#7591,#7592,#7593,#7594,#7595,#7596,#7597));
#1944=EDGE_LOOP('',(#7598,#7599,#7600,#7601,#7602,#7603));
#1945=EDGE_LOOP('',(#7604,#7605,#7606,#7607,#7608,#7609,#7610,#7611,#7612,
#7613,#7614,#7615,#7616,#7617,#7618,#7619,#7620,#7621));
#1946=EDGE_LOOP('',(#7622,#7623,#7624,#7625,#7626,#7627,#7628,#7629,#7630,
#7631,#7632,#7633,#7634,#7635,#7636,#7637,#7638,#7639,#7640,#7641,#7642,
#7643,#7644));
#1947=EDGE_LOOP('',(#7645,#7646,#7647,#7648,#7649,#7650,#7651,#7652,#7653,
#7654,#7655,#7656,#7657,#7658,#7659,#7660,#7661,#7662,#7663,#7664,#7665,
#7666,#7667,#7668,#7669));
#1948=EDGE_LOOP('',(#7670,#7671,#7672,#7673,#7674));
#1949=EDGE_LOOP('',(#7675,#7676,#7677,#7678));
#1950=EDGE_LOOP('',(#7679,#7680,#7681,#7682,#7683,#7684));
#1951=EDGE_LOOP('',(#7685,#7686,#7687,#7688));
#1952=EDGE_LOOP('',(#7689,#7690,#7691,#7692,#7693));
#1953=EDGE_LOOP('',(#7694,#7695,#7696));
#1954=EDGE_LOOP('',(#7697,#7698,#7699));
#1955=EDGE_LOOP('',(#7700,#7701,#7702,#7703,#7704));
#1956=EDGE_LOOP('',(#7705,#7706,#7707,#7708));
#1957=EDGE_LOOP('',(#7709,#7710,#7711,#7712));
#1958=EDGE_LOOP('',(#7713,#7714,#7715,#7716));
#1959=EDGE_LOOP('',(#7717,#7718,#7719,#7720));
#1960=EDGE_LOOP('',(#7721,#7722,#7723,#7724));
#1961=EDGE_LOOP('',(#7725,#7726,#7727,#7728));
#1962=EDGE_LOOP('',(#7729,#7730,#7731,#7732));
#1963=EDGE_LOOP('',(#7733,#7734));
#1964=EDGE_LOOP('',(#7735,#7736,#7737,#7738,#7739));
#1965=EDGE_LOOP('',(#7740,#7741,#7742,#7743,#7744));
#1966=EDGE_LOOP('',(#7745,#7746,#7747,#7748,#7749,#7750));
#1967=EDGE_LOOP('',(#7751,#7752,#7753,#7754,#7755));
#1968=EDGE_LOOP('',(#7756));
#1969=EDGE_LOOP('',(#7757));
#1970=EDGE_LOOP('',(#7758,#7759,#7760,#7761,#7762,#7763,#7764,#7765,#7766,
#7767,#7768,#7769,#7770,#7771,#7772,#7773,#7774,#7775,#7776,#7777,#7778,
#7779,#7780,#7781));
#1971=EDGE_LOOP('',(#7782,#7783,#7784,#7785,#7786,#7787,#7788,#7789,#7790,
#7791,#7792,#7793,#7794,#7795,#7796,#7797,#7798,#7799,#7800,#7801,#7802));
#1972=EDGE_LOOP('',(#7803,#7804,#7805,#7806,#7807,#7808,#7809,#7810,#7811,
#7812,#7813,#7814,#7815,#7816));
#1973=EDGE_LOOP('',(#7817,#7818,#7819,#7820,#7821,#7822,#7823,#7824,#7825,
#7826,#7827,#7828,#7829,#7830));
#1974=EDGE_LOOP('',(#7831,#7832,#7833,#7834));
#1975=EDGE_LOOP('',(#7835,#7836,#7837,#7838));
#1976=EDGE_LOOP('',(#7839));
#1977=EDGE_LOOP('',(#7840));
#1978=EDGE_LOOP('',(#7841,#7842,#7843,#7844));
#1979=EDGE_LOOP('',(#7845));
#1980=EDGE_LOOP('',(#7846));
#1981=EDGE_LOOP('',(#7847,#7848,#7849,#7850));
#1982=EDGE_LOOP('',(#7851,#7852,#7853,#7854));
#1983=EDGE_LOOP('',(#7855,#7856,#7857,#7858));
#1984=EDGE_LOOP('',(#7859,#7860,#7861,#7862));
#1985=EDGE_LOOP('',(#7863,#7864,#7865,#7866,#7867));
#1986=EDGE_LOOP('',(#7868,#7869,#7870,#7871,#7872,#7873,#7874,#7875,#7876,
#7877,#7878,#7879,#7880,#7881,#7882,#7883,#7884,#7885,#7886,#7887,#7888,
#7889,#7890,#7891,#7892));
#1987=EDGE_LOOP('',(#7893,#7894,#7895,#7896,#7897,#7898,#7899,#7900,#7901,
#7902,#7903,#7904,#7905,#7906,#7907,#7908,#7909,#7910,#7911));
#1988=EDGE_LOOP('',(#7912,#7913,#7914,#7915,#7916,#7917,#7918));
#1989=EDGE_LOOP('',(#7919));
#1990=EDGE_LOOP('',(#7920));
#1991=EDGE_LOOP('',(#7921,#7922,#7923,#7924,#7925,#7926,#7927,#7928,#7929,
#7930,#7931,#7932,#7933,#7934));
#1992=EDGE_LOOP('',(#7935,#7936,#7937,#7938,#7939));
#1993=EDGE_LOOP('',(#7940,#7941,#7942,#7943,#7944,#7945,#7946,#7947,#7948,
#7949,#7950,#7951,#7952,#7953));
#1994=EDGE_LOOP('',(#7954,#7955,#7956,#7957));
#1995=EDGE_LOOP('',(#7958));
#1996=EDGE_LOOP('',(#7959,#7960,#7961,#7962,#7963,#7964));
#1997=EDGE_LOOP('',(#7965,#7966,#7967,#7968));
#1998=EDGE_LOOP('',(#7969));
#1999=EDGE_LOOP('',(#7970,#7971,#7972,#7973));
#2000=EDGE_LOOP('',(#7974,#7975,#7976,#7977));
#2001=EDGE_LOOP('',(#7978,#7979,#7980,#7981));
#2002=EDGE_LOOP('',(#7982));
#2003=EDGE_LOOP('',(#7983,#7984,#7985,#7986));
#2004=EDGE_LOOP('',(#7987));
#2005=EDGE_LOOP('',(#7988,#7989,#7990,#7991));
#2006=EDGE_LOOP('',(#7992,#7993,#7994,#7995,#7996));
#2007=EDGE_LOOP('',(#7997,#7998,#7999,#8000));
#2008=EDGE_LOOP('',(#8001,#8002,#8003,#8004));
#2009=EDGE_LOOP('',(#8005,#8006,#8007,#8008));
#2010=EDGE_LOOP('',(#8009,#8010,#8011,#8012,#8013,#8014,#8015,#8016));
#2011=EDGE_LOOP('',(#8017,#8018,#8019,#8020));
#2012=EDGE_LOOP('',(#8021,#8022,#8023,#8024));
#2013=EDGE_LOOP('',(#8025,#8026,#8027,#8028,#8029,#8030,#8031,#8032,#8033,
#8034,#8035,#8036));
#2014=EDGE_LOOP('',(#8037,#8038,#8039,#8040));
#2015=EDGE_LOOP('',(#8041,#8042,#8043,#8044,#8045,#8046,#8047,#8048,#8049,
#8050,#8051,#8052));
#2016=EDGE_LOOP('',(#8053,#8054));
#2017=EDGE_LOOP('',(#8055,#8056,#8057,#8058,#8059));
#2018=EDGE_LOOP('',(#8060,#8061,#8062,#8063));
#2019=EDGE_LOOP('',(#8064,#8065,#8066,#8067,#8068,#8069,#8070,#8071));
#2020=EDGE_LOOP('',(#8072));
#2021=EDGE_LOOP('',(#8073,#8074,#8075,#8076));
#2022=EDGE_LOOP('',(#8077,#8078,#8079,#8080,#8081,#8082,#8083,#8084));
#2023=EDGE_LOOP('',(#8085));
#2024=EDGE_LOOP('',(#8086,#8087,#8088,#8089));
#2025=EDGE_LOOP('',(#8090,#8091,#8092,#8093));
#2026=EDGE_LOOP('',(#8094,#8095,#8096,#8097,#8098,#8099,#8100,#8101));
#2027=EDGE_LOOP('',(#8102,#8103,#8104,#8105));
#2028=EDGE_LOOP('',(#8106,#8107,#8108,#8109));
#2029=EDGE_LOOP('',(#8110,#8111,#8112,#8113));
#2030=EDGE_LOOP('',(#8114,#8115,#8116,#8117,#8118,#8119,#8120,#8121,#8122,
#8123,#8124,#8125));
#2031=EDGE_LOOP('',(#8126));
#2032=EDGE_LOOP('',(#8127,#8128,#8129,#8130));
#2033=EDGE_LOOP('',(#8131,#8132,#8133,#8134));
#2034=EDGE_LOOP('',(#8135,#8136,#8137,#8138));
#2035=EDGE_LOOP('',(#8139,#8140,#8141,#8142));
#2036=EDGE_LOOP('',(#8143,#8144,#8145,#8146,#8147,#8148,#8149,#8150));
#2037=EDGE_LOOP('',(#8151));
#2038=EDGE_LOOP('',(#8152,#8153,#8154,#8155));
#2039=EDGE_LOOP('',(#8156,#8157,#8158,#8159));
#2040=EDGE_LOOP('',(#8160,#8161,#8162,#8163,#8164,#8165,#8166,#8167));
#2041=EDGE_LOOP('',(#8168,#8169,#8170,#8171));
#2042=EDGE_LOOP('',(#8172,#8173,#8174,#8175));
#2043=EDGE_LOOP('',(#8176,#8177,#8178,#8179,#8180,#8181,#8182,#8183));
#2044=EDGE_LOOP('',(#8184,#8185,#8186,#8187));
#2045=EDGE_LOOP('',(#8188,#8189,#8190,#8191));
#2046=EDGE_LOOP('',(#8192,#8193,#8194,#8195));
#2047=EDGE_LOOP('',(#8196,#8197,#8198,#8199));
#2048=EDGE_LOOP('',(#8200,#8201,#8202));
#2049=EDGE_LOOP('',(#8203,#8204,#8205));
#2050=EDGE_LOOP('',(#8206,#8207,#8208));
#2051=EDGE_LOOP('',(#8209,#8210,#8211,#8212,#8213));
#2052=EDGE_LOOP('',(#8214,#8215,#8216,#8217));
#2053=EDGE_LOOP('',(#8218,#8219,#8220,#8221));
#2054=EDGE_LOOP('',(#8222));
#2055=EDGE_LOOP('',(#8223));
#2056=EDGE_LOOP('',(#8224,#8225,#8226,#8227,#8228));
#2057=EDGE_LOOP('',(#8229,#8230,#8231,#8232,#8233,#8234,#8235));
#2058=EDGE_LOOP('',(#8236,#8237,#8238,#8239,#8240));
#2059=EDGE_LOOP('',(#8241,#8242,#8243,#8244,#8245,#8246,#8247,#8248,#8249,
#8250,#8251,#8252,#8253,#8254,#8255));
#2060=EDGE_LOOP('',(#8256,#8257,#8258,#8259,#8260));
#2061=EDGE_LOOP('',(#8261,#8262,#8263,#8264,#8265,#8266,#8267,#8268,#8269,
#8270,#8271,#8272,#8273,#8274,#8275));
#2062=EDGE_LOOP('',(#8276));
#2063=EDGE_LOOP('',(#8277));
#2064=EDGE_LOOP('',(#8278,#8279,#8280,#8281));
#2065=EDGE_LOOP('',(#8282,#8283,#8284,#8285));
#2066=EDGE_LOOP('',(#8286,#8287,#8288,#8289));
#2067=EDGE_LOOP('',(#8290,#8291,#8292,#8293));
#2068=EDGE_LOOP('',(#8294,#8295,#8296,#8297));
#2069=EDGE_LOOP('',(#8298,#8299,#8300,#8301));
#2070=EDGE_LOOP('',(#8302,#8303,#8304,#8305));
#2071=EDGE_LOOP('',(#8306,#8307,#8308,#8309));
#2072=EDGE_LOOP('',(#8310,#8311,#8312,#8313));
#2073=EDGE_LOOP('',(#8314,#8315,#8316,#8317));
#2074=EDGE_LOOP('',(#8318,#8319,#8320,#8321));
#2075=EDGE_LOOP('',(#8322,#8323,#8324,#8325));
#2076=EDGE_LOOP('',(#8326,#8327,#8328,#8329));
#2077=EDGE_LOOP('',(#8330,#8331,#8332,#8333));
#2078=EDGE_LOOP('',(#8334,#8335,#8336,#8337));
#2079=EDGE_LOOP('',(#8338,#8339,#8340,#8341));
#2080=EDGE_LOOP('',(#8342,#8343,#8344,#8345));
#2081=EDGE_LOOP('',(#8346,#8347,#8348,#8349));
#2082=EDGE_LOOP('',(#8350,#8351,#8352,#8353));
#2083=EDGE_LOOP('',(#8354,#8355,#8356,#8357));
#2084=EDGE_LOOP('',(#8358,#8359,#8360,#8361));
#2085=EDGE_LOOP('',(#8362,#8363,#8364,#8365,#8366));
#2086=EDGE_LOOP('',(#8367,#8368,#8369,#8370));
#2087=EDGE_LOOP('',(#8371,#8372,#8373,#8374,#8375));
#2088=EDGE_LOOP('',(#8376,#8377,#8378,#8379,#8380,#8381));
#2089=EDGE_LOOP('',(#8382,#8383,#8384,#8385));
#2090=EDGE_LOOP('',(#8386,#8387,#8388,#8389,#8390));
#2091=EDGE_LOOP('',(#8391,#8392,#8393,#8394));
#2092=EDGE_LOOP('',(#8395,#8396,#8397,#8398,#8399));
#2093=EDGE_LOOP('',(#8400,#8401,#8402,#8403,#8404,#8405));
#2094=EDGE_LOOP('',(#8406,#8407,#8408,#8409,#8410,#8411));
#2095=EDGE_LOOP('',(#8412,#8413,#8414,#8415,#8416,#8417));
#2096=EDGE_LOOP('',(#8418,#8419,#8420,#8421,#8422,#8423,#8424,#8425,#8426,
#8427,#8428,#8429,#8430,#8431,#8432,#8433));
#2097=EDGE_LOOP('',(#8434,#8435,#8436,#8437,#8438,#8439,#8440));
#2098=EDGE_LOOP('',(#8441,#8442,#8443,#8444,#8445,#8446,#8447,#8448,#8449,
#8450,#8451,#8452,#8453,#8454,#8455,#8456));
#2099=EDGE_LOOP('',(#8457,#8458,#8459,#8460,#8461,#8462,#8463));
#2100=EDGE_LOOP('',(#8464,#8465,#8466,#8467,#8468,#8469,#8470,#8471,#8472,
#8473,#8474,#8475));
#2101=EDGE_LOOP('',(#8476));
#2102=EDGE_LOOP('',(#8477));
#2103=EDGE_LOOP('',(#8478,#8479,#8480,#8481));
#2104=EDGE_LOOP('',(#8482,#8483,#8484,#8485));
#2105=EDGE_LOOP('',(#8486,#8487,#8488,#8489,#8490,#8491));
#2106=EDGE_LOOP('',(#8492,#8493,#8494,#8495));
#2107=EDGE_LOOP('',(#8496,#8497,#8498,#8499));
#2108=EDGE_LOOP('',(#8500,#8501,#8502,#8503,#8504,#8505));
#2109=EDGE_LOOP('',(#8506,#8507,#8508,#8509));
#2110=EDGE_LOOP('',(#8510,#8511,#8512,#8513,#8514,#8515,#8516));
#2111=EDGE_LOOP('',(#8517,#8518,#8519,#8520));
#2112=EDGE_LOOP('',(#8521,#8522,#8523,#8524));
#2113=EDGE_LOOP('',(#8525,#8526,#8527,#8528,#8529,#8530,#8531));
#2114=EDGE_LOOP('',(#8532,#8533,#8534,#8535));
#2115=EDGE_LOOP('',(#8536,#8537,#8538,#8539));
#2116=EDGE_LOOP('',(#8540,#8541,#8542,#8543));
#2117=EDGE_LOOP('',(#8544,#8545,#8546,#8547,#8548,#8549));
#2118=EDGE_LOOP('',(#8550,#8551,#8552,#8553));
#2119=EDGE_LOOP('',(#8554,#8555,#8556,#8557));
#2120=EDGE_LOOP('',(#8558,#8559,#8560,#8561,#8562,#8563));
#2121=EDGE_LOOP('',(#8564,#8565,#8566,#8567,#8568,#8569,#8570));
#2122=EDGE_LOOP('',(#8571,#8572,#8573,#8574,#8575,#8576,#8577));
#2123=EDGE_LOOP('',(#8578,#8579,#8580,#8581));
#2124=EDGE_LOOP('',(#8582,#8583,#8584,#8585,#8586,#8587));
#2125=EDGE_LOOP('',(#8588,#8589,#8590,#8591));
#2126=EDGE_LOOP('',(#8592,#8593,#8594,#8595));
#2127=EDGE_LOOP('',(#8596,#8597,#8598,#8599));
#2128=EDGE_LOOP('',(#8600,#8601,#8602,#8603));
#2129=EDGE_LOOP('',(#8604,#8605,#8606,#8607));
#2130=EDGE_LOOP('',(#8608,#8609,#8610,#8611));
#2131=EDGE_LOOP('',(#8612,#8613,#8614,#8615,#8616,#8617));
#2132=EDGE_LOOP('',(#8618,#8619,#8620,#8621));
#2133=EDGE_LOOP('',(#8622,#8623,#8624,#8625));
#2134=EDGE_LOOP('',(#8626,#8627,#8628,#8629));
#2135=EDGE_LOOP('',(#8630,#8631,#8632,#8633));
#2136=EDGE_LOOP('',(#8634));
#2137=EDGE_LOOP('',(#8635));
#2138=EDGE_LOOP('',(#8636,#8637,#8638,#8639,#8640,#8641));
#2139=EDGE_LOOP('',(#8642));
#2140=EDGE_LOOP('',(#8643,#8644,#8645,#8646));
#2141=EDGE_LOOP('',(#8647,#8648,#8649,#8650,#8651,#8652));
#2142=EDGE_LOOP('',(#8653,#8654,#8655,#8656,#8657,#8658,#8659,#8660,#8661,
#8662,#8663,#8664));
#2143=EDGE_LOOP('',(#8665,#8666,#8667,#8668,#8669,#8670,#8671,#8672,#8673,
#8674,#8675,#8676));
#2144=EDGE_LOOP('',(#8677,#8678,#8679,#8680));
#2145=EDGE_LOOP('',(#8681,#8682,#8683,#8684));
#2146=EDGE_LOOP('',(#8685,#8686,#8687,#8688,#8689,#8690,#8691));
#2147=EDGE_LOOP('',(#8692,#8693,#8694,#8695));
#2148=EDGE_LOOP('',(#8696,#8697,#8698,#8699));
#2149=EDGE_LOOP('',(#8700,#8701,#8702,#8703,#8704,#8705,#8706,#8707,#8708));
#2150=EDGE_LOOP('',(#8709,#8710,#8711,#8712));
#2151=EDGE_LOOP('',(#8713,#8714,#8715,#8716));
#2152=EDGE_LOOP('',(#8717,#8718,#8719,#8720));
#2153=EDGE_LOOP('',(#8721,#8722,#8723,#8724));
#2154=EDGE_LOOP('',(#8725,#8726,#8727,#8728,#8729,#8730,#8731));
#2155=EDGE_LOOP('',(#8732,#8733,#8734,#8735,#8736,#8737,#8738,#8739,#8740,
#8741,#8742,#8743,#8744,#8745,#8746,#8747));
#2156=EDGE_LOOP('',(#8748,#8749,#8750,#8751,#8752,#8753,#8754,#8755,#8756,
#8757,#8758,#8759));
#2157=EDGE_LOOP('',(#8760,#8761,#8762,#8763));
#2158=EDGE_LOOP('',(#8764,#8765,#8766,#8767));
#2159=EDGE_LOOP('',(#8768));
#2160=EDGE_LOOP('',(#8769));
#2161=EDGE_LOOP('',(#8770,#8771,#8772,#8773));
#2162=EDGE_LOOP('',(#8774,#8775,#8776,#8777));
#2163=EDGE_LOOP('',(#8778,#8779,#8780,#8781));
#2164=EDGE_LOOP('',(#8782,#8783,#8784,#8785));
#2165=EDGE_LOOP('',(#8786,#8787,#8788,#8789));
#2166=EDGE_LOOP('',(#8790,#8791,#8792,#8793));
#2167=EDGE_LOOP('',(#8794,#8795,#8796,#8797));
#2168=EDGE_LOOP('',(#8798,#8799,#8800,#8801));
#2169=EDGE_LOOP('',(#8802,#8803,#8804,#8805));
#2170=EDGE_LOOP('',(#8806,#8807,#8808,#8809));
#2171=EDGE_LOOP('',(#8810,#8811,#8812,#8813));
#2172=EDGE_LOOP('',(#8814,#8815,#8816,#8817));
#2173=EDGE_LOOP('',(#8818,#8819,#8820,#8821));
#2174=EDGE_LOOP('',(#8822,#8823,#8824,#8825));
#2175=EDGE_LOOP('',(#8826,#8827,#8828,#8829));
#2176=EDGE_LOOP('',(#8830,#8831,#8832,#8833));
#2177=EDGE_LOOP('',(#8834,#8835,#8836,#8837));
#2178=EDGE_LOOP('',(#8838,#8839,#8840,#8841));
#2179=EDGE_LOOP('',(#8842,#8843,#8844,#8845));
#2180=EDGE_LOOP('',(#8846,#8847,#8848,#8849));
#2181=EDGE_LOOP('',(#8850,#8851,#8852,#8853));
#2182=EDGE_LOOP('',(#8854,#8855,#8856,#8857));
#2183=EDGE_LOOP('',(#8858,#8859,#8860,#8861));
#2184=EDGE_LOOP('',(#8862,#8863,#8864,#8865));
#2185=EDGE_LOOP('',(#8866,#8867,#8868,#8869));
#2186=EDGE_LOOP('',(#8870,#8871,#8872,#8873));
#2187=EDGE_LOOP('',(#8874,#8875,#8876,#8877));
#2188=EDGE_LOOP('',(#8878,#8879,#8880,#8881));
#2189=EDGE_LOOP('',(#8882,#8883,#8884,#8885));
#2190=EDGE_LOOP('',(#8886,#8887,#8888,#8889));
#2191=EDGE_LOOP('',(#8890,#8891,#8892,#8893));
#2192=EDGE_LOOP('',(#8894,#8895,#8896,#8897));
#2193=EDGE_LOOP('',(#8898,#8899,#8900,#8901));
#2194=EDGE_LOOP('',(#8902,#8903));
#2195=EDGE_LOOP('',(#8904,#8905,#8906,#8907));
#2196=EDGE_LOOP('',(#8908));
#2197=EDGE_LOOP('',(#8909));
#2198=EDGE_LOOP('',(#8910,#8911,#8912,#8913,#8914,#8915,#8916,#8917));
#2199=EDGE_LOOP('',(#8918));
#2200=EDGE_LOOP('',(#8919,#8920,#8921,#8922,#8923,#8924,#8925,#8926,#8927,
#8928,#8929,#8930,#8931,#8932,#8933,#8934,#8935,#8936,#8937,#8938,#8939,
#8940,#8941,#8942,#8943,#8944,#8945,#8946,#8947,#8948,#8949,#8950,#8951,
#8952,#8953,#8954));
#2201=EDGE_LOOP('',(#8955,#8956,#8957,#8958,#8959,#8960,#8961,#8962,#8963,
#8964,#8965,#8966,#8967,#8968,#8969,#8970,#8971,#8972,#8973,#8974,#8975,
#8976,#8977,#8978,#8979,#8980,#8981,#8982,#8983,#8984,#8985,#8986,#8987,
#8988,#8989));
#2202=EDGE_LOOP('',(#8990));
#2203=EDGE_LOOP('',(#8991,#8992,#8993,#8994,#8995,#8996));
#2204=EDGE_LOOP('',(#8997));
#2205=EDGE_LOOP('',(#8998,#8999,#9000,#9001));
#2206=EDGE_LOOP('',(#9002,#9003));
#2207=EDGE_LOOP('',(#9004,#9005));
#2208=EDGE_LOOP('',(#9006,#9007));
#2209=EDGE_LOOP('',(#9008,#9009));
#2210=EDGE_LOOP('',(#9010,#9011));
#2211=EDGE_LOOP('',(#9012,#9013,#9014,#9015,#9016,#9017));
#2212=EDGE_LOOP('',(#9018,#9019,#9020,#9021));
#2213=EDGE_LOOP('',(#9022,#9023,#9024,#9025));
#2214=EDGE_LOOP('',(#9026,#9027,#9028,#9029));
#2215=EDGE_LOOP('',(#9030,#9031,#9032,#9033));
#2216=EDGE_LOOP('',(#9034,#9035,#9036,#9037));
#2217=EDGE_LOOP('',(#9038,#9039,#9040,#9041));
#2218=EDGE_LOOP('',(#9042));
#2219=EDGE_LOOP('',(#9043,#9044,#9045,#9046,#9047));
#2220=EDGE_LOOP('',(#9048,#9049,#9050,#9051,#9052,#9053));
#2221=EDGE_LOOP('',(#9054,#9055,#9056,#9057,#9058));
#2222=EDGE_LOOP('',(#9059));
#2223=EDGE_LOOP('',(#9060,#9061,#9062,#9063,#9064));
#2224=EDGE_LOOP('',(#9065,#9066,#9067,#9068,#9069,#9070));
#2225=EDGE_LOOP('',(#9071,#9072,#9073,#9074,#9075));
#2226=EDGE_LOOP('',(#9076));
#2227=EDGE_LOOP('',(#9077));
#2228=EDGE_LOOP('',(#9078,#9079,#9080,#9081));
#2229=EDGE_LOOP('',(#9082,#9083,#9084,#9085,#9086));
#2230=EDGE_LOOP('',(#9087,#9088,#9089,#9090,#9091,#9092));
#2231=EDGE_LOOP('',(#9093,#9094,#9095,#9096));
#2232=EDGE_LOOP('',(#9097,#9098,#9099,#9100));
#2233=EDGE_LOOP('',(#9101,#9102,#9103,#9104));
#2234=EDGE_LOOP('',(#9105,#9106,#9107,#9108,#9109));
#2235=EDGE_LOOP('',(#9110));
#2236=EDGE_LOOP('',(#9111,#9112,#9113,#9114));
#2237=EDGE_LOOP('',(#9115));
#2238=EDGE_LOOP('',(#9116));
#2239=EDGE_LOOP('',(#9117,#9118,#9119,#9120,#9121));
#2240=EDGE_LOOP('',(#9122,#9123,#9124,#9125,#9126,#9127,#9128,#9129,#9130,
#9131));
#2241=EDGE_LOOP('',(#9132,#9133,#9134,#9135,#9136,#9137,#9138));
#2242=EDGE_LOOP('',(#9139,#9140,#9141,#9142,#9143,#9144,#9145));
#2243=LINE('',#13477,#2821);
#2244=LINE('',#13489,#2822);
#2245=LINE('',#13500,#2823);
#2246=LINE('',#13510,#2824);
#2247=LINE('',#13521,#2825);
#2248=LINE('',#13538,#2826);
#2249=LINE('',#13542,#2827);
#2250=LINE('',#13546,#2828);
#2251=LINE('',#13550,#2829);
#2252=LINE('',#13554,#2830);
#2253=LINE('',#13558,#2831);
#2254=LINE('',#13562,#2832);
#2255=LINE('',#13566,#2833);
#2256=LINE('',#13568,#2834);
#2257=LINE('',#13577,#2835);
#2258=LINE('',#13583,#2836);
#2259=LINE('',#13587,#2837);
#2260=LINE('',#13591,#2838);
#2261=LINE('',#13595,#2839);
#2262=LINE('',#13603,#2840);
#2263=LINE('',#13607,#2841);
#2264=LINE('',#13611,#2842);
#2265=LINE('',#13615,#2843);
#2266=LINE('',#13623,#2844);
#2267=LINE('',#13627,#2845);
#2268=LINE('',#13631,#2846);
#2269=LINE('',#13635,#2847);
#2270=LINE('',#13643,#2848);
#2271=LINE('',#13647,#2849);
#2272=LINE('',#13651,#2850);
#2273=LINE('',#13655,#2851);
#2274=LINE('',#13664,#2852);
#2275=LINE('',#13669,#2853);
#2276=LINE('',#13679,#2854);
#2277=LINE('',#13681,#2855);
#2278=LINE('',#13684,#2856);
#2279=LINE('',#13689,#2857);
#2280=LINE('',#13692,#2858);
#2281=LINE('',#13700,#2859);
#2282=LINE('',#13701,#2860);
#2283=LINE('',#13705,#2861);
#2284=LINE('',#13711,#2862);
#2285=LINE('',#13718,#2863);
#2286=LINE('',#13719,#2864);
#2287=LINE('',#13723,#2865);
#2288=LINE('',#13735,#2866);
#2289=LINE('',#13739,#2867);
#2290=LINE('',#13742,#2868);
#2291=LINE('',#13743,#2869);
#2292=LINE('',#13746,#2870);
#2293=LINE('',#13749,#2871);
#2294=LINE('',#13750,#2872);
#2295=LINE('',#13754,#2873);
#2296=LINE('',#13765,#2874);
#2297=LINE('',#13766,#2875);
#2298=LINE('',#13767,#2876);
#2299=LINE('',#13777,#2877);
#2300=LINE('',#13779,#2878);
#2301=LINE('',#13780,#2879);
#2302=LINE('',#13782,#2880);
#2303=LINE('',#13787,#2881);
#2304=LINE('',#13788,#2882);
#2305=LINE('',#13789,#2883);
#2306=LINE('',#13797,#2884);
#2307=LINE('',#13799,#2885);
#2308=LINE('',#13800,#2886);
#2309=LINE('',#13802,#2887);
#2310=LINE('',#13809,#2888);
#2311=LINE('',#13810,#2889);
#2312=LINE('',#13811,#2890);
#2313=LINE('',#13820,#2891);
#2314=LINE('',#13822,#2892);
#2315=LINE('',#13823,#2893);
#2316=LINE('',#13825,#2894);
#2317=LINE('',#13827,#2895);
#2318=LINE('',#13829,#2896);
#2319=LINE('',#13831,#2897);
#2320=LINE('',#13833,#2898);
#2321=LINE('',#13835,#2899);
#2322=LINE('',#13837,#2900);
#2323=LINE('',#13839,#2901);
#2324=LINE('',#13841,#2902);
#2325=LINE('',#13847,#2903);
#2326=LINE('',#13849,#2904);
#2327=LINE('',#13851,#2905);
#2328=LINE('',#13856,#2906);
#2329=LINE('',#13859,#2907);
#2330=LINE('',#13862,#2908);
#2331=LINE('',#16783,#2909);
#2332=LINE('',#16790,#2910);
#2333=LINE('',#16798,#2911);
#2334=LINE('',#16802,#2912);
#2335=LINE('',#16808,#2913);
#2336=LINE('',#16813,#2914);
#2337=LINE('',#16817,#2915);
#2338=LINE('',#17808,#2916);
#2339=LINE('',#17887,#2917);
#2340=LINE('',#17889,#2918);
#2341=LINE('',#17891,#2919);
#2342=LINE('',#17893,#2920);
#2343=LINE('',#17895,#2921);
#2344=LINE('',#17897,#2922);
#2345=LINE('',#17899,#2923);
#2346=LINE('',#17901,#2924);
#2347=LINE('',#17904,#2925);
#2348=LINE('',#17907,#2926);
#2349=LINE('',#17909,#2927);
#2350=LINE('',#17911,#2928);
#2351=LINE('',#17913,#2929);
#2352=LINE('',#17915,#2930);
#2353=LINE('',#17917,#2931);
#2354=LINE('',#17923,#2932);
#2355=LINE('',#17929,#2933);
#2356=LINE('',#17935,#2934);
#2357=LINE('',#17941,#2935);
#2358=LINE('',#17944,#2936);
#2359=LINE('',#17951,#2937);
#2360=LINE('',#17959,#2938);
#2361=LINE('',#17967,#2939);
#2362=LINE('',#17975,#2940);
#2363=LINE('',#17985,#2941);
#2364=LINE('',#17988,#2942);
#2365=LINE('',#17993,#2943);
#2366=LINE('',#17995,#2944);
#2367=LINE('',#17998,#2945);
#2368=LINE('',#18001,#2946);
#2369=LINE('',#18008,#2947);
#2370=LINE('',#18010,#2948);
#2371=LINE('',#18011,#2949);
#2372=LINE('',#18015,#2950);
#2373=LINE('',#18018,#2951);
#2374=LINE('',#18022,#2952);
#2375=LINE('',#18026,#2953);
#2376=LINE('',#18028,#2954);
#2377=LINE('',#18029,#2955);
#2378=LINE('',#18032,#2956);
#2379=LINE('',#18034,#2957);
#2380=LINE('',#18036,#2958);
#2381=LINE('',#18037,#2959);
#2382=LINE('',#18041,#2960);
#2383=LINE('',#18043,#2961);
#2384=LINE('',#18045,#2962);
#2385=LINE('',#18046,#2963);
#2386=LINE('',#18050,#2964);
#2387=LINE('',#18052,#2965);
#2388=LINE('',#18054,#2966);
#2389=LINE('',#18055,#2967);
#2390=LINE('',#18057,#2968);
#2391=LINE('',#18058,#2969);
#2392=LINE('',#18066,#2970);
#2393=LINE('',#18069,#2971);
#2394=LINE('',#18070,#2972);
#2395=LINE('',#18072,#2973);
#2396=LINE('',#18073,#2974);
#2397=LINE('',#18084,#2975);
#2398=LINE('',#18095,#2976);
#2399=LINE('',#18102,#2977);
#2400=LINE('',#18114,#2978);
#2401=LINE('',#18123,#2979);
#2402=LINE('',#18135,#2980);
#2403=LINE('',#18143,#2981);
#2404=LINE('',#18223,#2982);
#2405=LINE('',#18592,#2983);
#2406=LINE('',#18957,#2984);
#2407=LINE('',#19317,#2985);
#2408=LINE('',#19677,#2986);
#2409=LINE('',#20039,#2987);
#2410=LINE('',#20412,#2988);
#2411=LINE('',#20536,#2989);
#2412=LINE('',#20646,#2990);
#2413=LINE('',#21044,#2991);
#2414=LINE('',#21466,#2992);
#2415=LINE('',#21858,#2993);
#2416=LINE('',#22280,#2994);
#2417=LINE('',#22704,#2995);
#2418=LINE('',#23110,#2996);
#2419=LINE('',#23528,#2997);
#2420=LINE('',#23930,#2998);
#2421=LINE('',#24346,#2999);
#2422=LINE('',#24745,#3000);
#2423=LINE('',#25168,#3001);
#2424=LINE('',#25304,#3002);
#2425=LINE('',#25357,#3003);
#2426=LINE('',#25444,#3004);
#2427=LINE('',#25659,#3005);
#2428=LINE('',#25866,#3006);
#2429=LINE('',#26073,#3007);
#2430=LINE('',#26298,#3008);
#2431=LINE('',#26379,#3009);
#2432=LINE('',#26436,#3010);
#2433=LINE('',#26538,#3011);
#2434=LINE('',#26640,#3012);
#2435=LINE('',#26742,#3013);
#2436=LINE('',#26850,#3014);
#2437=LINE('',#26952,#3015);
#2438=LINE('',#27054,#3016);
#2439=LINE('',#27168,#3017);
#2440=LINE('',#27267,#3018);
#2441=LINE('',#27369,#3019);
#2442=LINE('',#27471,#3020);
#2443=LINE('',#27858,#3021);
#2444=LINE('',#27860,#3022);
#2445=LINE('',#27862,#3023);
#2446=LINE('',#27863,#3024);
#2447=LINE('',#27866,#3025);
#2448=LINE('',#27868,#3026);
#2449=LINE('',#27869,#3027);
#2450=LINE('',#27872,#3028);
#2451=LINE('',#27874,#3029);
#2452=LINE('',#27875,#3030);
#2453=LINE('',#27882,#3031);
#2454=LINE('',#27884,#3032);
#2455=LINE('',#27886,#3033);
#2456=LINE('',#27891,#3034);
#2457=LINE('',#27896,#3035);
#2458=LINE('',#27897,#3036);
#2459=LINE('',#27901,#3037);
#2460=LINE('',#27902,#3038);
#2461=LINE('',#27904,#3039);
#2462=LINE('',#27906,#3040);
#2463=LINE('',#27915,#3041);
#2464=LINE('',#27917,#3042);
#2465=LINE('',#27923,#3043);
#2466=LINE('',#27924,#3044);
#2467=LINE('',#27928,#3045);
#2468=LINE('',#27930,#3046);
#2469=LINE('',#27932,#3047);
#2470=LINE('',#27934,#3048);
#2471=LINE('',#27939,#3049);
#2472=LINE('',#27945,#3050);
#2473=LINE('',#27957,#3051);
#2474=LINE('',#27959,#3052);
#2475=LINE('',#27961,#3053);
#2476=LINE('',#27962,#3054);
#2477=LINE('',#27964,#3055);
#2478=LINE('',#27966,#3056);
#2479=LINE('',#27973,#3057);
#2480=LINE('',#27979,#3058);
#2481=LINE('',#27982,#3059);
#2482=LINE('',#27988,#3060);
#2483=LINE('',#27990,#3061);
#2484=LINE('',#27991,#3062);
#2485=LINE('',#27993,#3063);
#2486=LINE('',#27995,#3064);
#2487=LINE('',#28002,#3065);
#2488=LINE('',#28003,#3066);
#2489=LINE('',#28004,#3067);
#2490=LINE('',#28007,#3068);
#2491=LINE('',#28009,#3069);
#2492=LINE('',#28010,#3070);
#2493=LINE('',#28013,#3071);
#2494=LINE('',#28015,#3072);
#2495=LINE('',#28016,#3073);
#2496=LINE('',#28019,#3074);
#2497=LINE('',#28020,#3075);
#2498=LINE('',#28077,#3076);
#2499=LINE('',#28083,#3077);
#2500=LINE('',#28085,#3078);
#2501=LINE('',#28086,#3079);
#2502=LINE('',#28089,#3080);
#2503=LINE('',#28090,#3081);
#2504=LINE('',#28093,#3082);
#2505=LINE('',#28095,#3083);
#2506=LINE('',#28096,#3084);
#2507=LINE('',#28100,#3085);
#2508=LINE('',#29355,#3086);
#2509=LINE('',#29358,#3087);
#2510=LINE('',#29360,#3088);
#2511=LINE('',#29361,#3089);
#2512=LINE('',#29367,#3090);
#2513=LINE('',#29369,#3091);
#2514=LINE('',#30512,#3092);
#2515=LINE('',#30597,#3093);
#2516=LINE('',#30682,#3094);
#2517=LINE('',#30685,#3095);
#2518=LINE('',#30687,#3096);
#2519=LINE('',#33779,#3097);
#2520=LINE('',#34593,#3098);
#2521=LINE('',#34770,#3099);
#2522=LINE('',#34782,#3100);
#2523=LINE('',#39240,#3101);
#2524=LINE('',#39245,#3102);
#2525=LINE('',#39253,#3103);
#2526=LINE('',#39260,#3104);
#2527=LINE('',#39263,#3105);
#2528=LINE('',#39267,#3106);
#2529=LINE('',#39270,#3107);
#2530=LINE('',#40002,#3108);
#2531=LINE('',#40468,#3109);
#2532=LINE('',#40473,#3110);
#2533=LINE('',#40479,#3111);
#2534=LINE('',#40484,#3112);
#2535=LINE('',#40488,#3113);
#2536=LINE('',#40495,#3114);
#2537=LINE('',#40582,#3115);
#2538=LINE('',#40905,#3116);
#2539=LINE('',#41223,#3117);
#2540=LINE('',#41543,#3118);
#2541=LINE('',#41891,#3119);
#2542=LINE('',#41921,#3120);
#2543=LINE('',#43613,#3121);
#2544=LINE('',#43615,#3122);
#2545=LINE('',#43617,#3123);
#2546=LINE('',#43619,#3124);
#2547=LINE('',#43621,#3125);
#2548=LINE('',#43623,#3126);
#2549=LINE('',#43625,#3127);
#2550=LINE('',#43627,#3128);
#2551=LINE('',#43629,#3129);
#2552=LINE('',#43631,#3130);
#2553=LINE('',#43633,#3131);
#2554=LINE('',#43634,#3132);
#2555=LINE('',#43637,#3133);
#2556=LINE('',#43641,#3134);
#2557=LINE('',#43643,#3135);
#2558=LINE('',#43644,#3136);
#2559=LINE('',#43647,#3137);
#2560=LINE('',#43649,#3138);
#2561=LINE('',#43651,#3139);
#2562=LINE('',#43653,#3140);
#2563=LINE('',#43655,#3141);
#2564=LINE('',#43656,#3142);
#2565=LINE('',#43661,#3143);
#2566=LINE('',#43663,#3144);
#2567=LINE('',#43664,#3145);
#2568=LINE('',#43667,#3146);
#2569=LINE('',#43669,#3147);
#2570=LINE('',#43671,#3148);
#2571=LINE('',#43673,#3149);
#2572=LINE('',#43675,#3150);
#2573=LINE('',#43676,#3151);
#2574=LINE('',#43681,#3152);
#2575=LINE('',#43682,#3153);
#2576=LINE('',#43685,#3154);
#2577=LINE('',#43687,#3155);
#2578=LINE('',#43688,#3156);
#2579=LINE('',#43691,#3157);
#2580=LINE('',#43693,#3158);
#2581=LINE('',#43695,#3159);
#2582=LINE('',#43697,#3160);
#2583=LINE('',#43699,#3161);
#2584=LINE('',#43700,#3162);
#2585=LINE('',#43703,#3163);
#2586=LINE('',#43704,#3164);
#2587=LINE('',#43707,#3165);
#2588=LINE('',#43708,#3166);
#2589=LINE('',#43711,#3167);
#2590=LINE('',#43713,#3168);
#2591=LINE('',#43714,#3169);
#2592=LINE('',#43717,#3170);
#2593=LINE('',#43718,#3171);
#2594=LINE('',#43720,#3172);
#2595=LINE('',#43722,#3173);
#2596=LINE('',#43723,#3174);
#2597=LINE('',#43725,#3175);
#2598=LINE('',#43727,#3176);
#2599=LINE('',#43728,#3177);
#2600=LINE('',#43733,#3178);
#2601=LINE('',#43734,#3179);
#2602=LINE('',#43737,#3180);
#2603=LINE('',#43738,#3181);
#2604=LINE('',#43741,#3182);
#2605=LINE('',#43742,#3183);
#2606=LINE('',#43745,#3184);
#2607=LINE('',#43746,#3185);
#2608=LINE('',#43749,#3186);
#2609=LINE('',#43750,#3187);
#2610=LINE('',#43751,#3188);
#2611=LINE('',#43756,#3189);
#2612=LINE('',#43758,#3190);
#2613=LINE('',#43761,#3191);
#2614=LINE('',#43763,#3192);
#2615=LINE('',#43766,#3193);
#2616=LINE('',#43847,#3194);
#2617=LINE('',#43850,#3195);
#2618=LINE('',#43853,#3196);
#2619=LINE('',#43858,#3197);
#2620=LINE('',#43865,#3198);
#2621=LINE('',#43870,#3199);
#2622=LINE('',#43876,#3200);
#2623=LINE('',#43881,#3201);
#2624=LINE('',#45423,#3202);
#2625=LINE('',#45424,#3203);
#2626=LINE('',#45468,#3204);
#2627=LINE('',#45469,#3205);
#2628=LINE('',#45471,#3206);
#2629=LINE('',#45472,#3207);
#2630=LINE('',#45516,#3208);
#2631=LINE('',#45517,#3209);
#2632=LINE('',#45561,#3210);
#2633=LINE('',#45562,#3211);
#2634=LINE('',#45564,#3212);
#2635=LINE('',#45565,#3213);
#2636=LINE('',#45567,#3214);
#2637=LINE('',#45568,#3215);
#2638=LINE('',#45570,#3216);
#2639=LINE('',#45571,#3217);
#2640=LINE('',#45574,#3218);
#2641=LINE('',#45576,#3219);
#2642=LINE('',#45580,#3220);
#2643=LINE('',#45582,#3221);
#2644=LINE('',#45584,#3222);
#2645=LINE('',#45588,#3223);
#2646=LINE('',#45589,#3224);
#2647=LINE('',#45592,#3225);
#2648=LINE('',#45594,#3226);
#2649=LINE('',#45596,#3227);
#2650=LINE('',#45598,#3228);
#2651=LINE('',#45599,#3229);
#2652=LINE('',#45602,#3230);
#2653=LINE('',#45604,#3231);
#2654=LINE('',#45606,#3232);
#2655=LINE('',#45608,#3233);
#2656=LINE('',#45610,#3234);
#2657=LINE('',#45612,#3235);
#2658=LINE('',#45614,#3236);
#2659=LINE('',#45615,#3237);
#2660=LINE('',#45618,#3238);
#2661=LINE('',#45620,#3239);
#2662=LINE('',#45622,#3240);
#2663=LINE('',#45624,#3241);
#2664=LINE('',#45625,#3242);
#2665=LINE('',#45636,#3243);
#2666=LINE('',#45639,#3244);
#2667=LINE('',#45641,#3245);
#2668=LINE('',#45642,#3246);
#2669=LINE('',#45645,#3247);
#2670=LINE('',#45647,#3248);
#2671=LINE('',#45648,#3249);
#2672=LINE('',#45654,#3250);
#2673=LINE('',#45657,#3251);
#2674=LINE('',#45659,#3252);
#2675=LINE('',#45660,#3253);
#2676=LINE('',#45663,#3254);
#2677=LINE('',#45664,#3255);
#2678=LINE('',#45670,#3256);
#2679=LINE('',#45673,#3257);
#2680=LINE('',#45675,#3258);
#2681=LINE('',#45677,#3259);
#2682=LINE('',#45679,#3260);
#2683=LINE('',#45681,#3261);
#2684=LINE('',#45682,#3262);
#2685=LINE('',#45684,#3263);
#2686=LINE('',#45690,#3264);
#2687=LINE('',#45693,#3265);
#2688=LINE('',#45696,#3266);
#2689=LINE('',#45698,#3267);
#2690=LINE('',#45700,#3268);
#2691=LINE('',#45702,#3269);
#2692=LINE('',#45704,#3270);
#2693=LINE('',#45705,#3271);
#2694=LINE('',#45708,#3272);
#2695=LINE('',#45709,#3273);
#2696=LINE('',#45715,#3274);
#2697=LINE('',#45718,#3275);
#2698=LINE('',#45721,#3276);
#2699=LINE('',#45723,#3277);
#2700=LINE('',#45724,#3278);
#2701=LINE('',#45727,#3279);
#2702=LINE('',#45729,#3280);
#2703=LINE('',#45731,#3281);
#2704=LINE('',#45732,#3282);
#2705=LINE('',#45735,#3283);
#2706=LINE('',#45737,#3284);
#2707=LINE('',#45738,#3285);
#2708=LINE('',#45740,#3286);
#2709=LINE('',#45743,#3287);
#2710=LINE('',#45744,#3288);
#2711=LINE('',#45746,#3289);
#2712=LINE('',#45748,#3290);
#2713=LINE('',#45750,#3291);
#2714=LINE('',#45752,#3292);
#2715=LINE('',#45753,#3293);
#2716=LINE('',#45756,#3294);
#2717=LINE('',#45758,#3295);
#2718=LINE('',#45759,#3296);
#2719=LINE('',#45760,#3297);
#2720=LINE('',#45763,#3298);
#2721=LINE('',#45764,#3299);
#2722=LINE('',#45766,#3300);
#2723=LINE('',#45768,#3301);
#2724=LINE('',#45771,#3302);
#2725=LINE('',#45772,#3303);
#2726=LINE('',#45775,#3304);
#2727=LINE('',#45776,#3305);
#2728=LINE('',#45779,#3306);
#2729=LINE('',#45780,#3307);
#2730=LINE('',#45782,#3308);
#2731=LINE('',#45784,#3309);
#2732=LINE('',#45785,#3310);
#2733=LINE('',#45787,#3311);
#2734=LINE('',#45791,#3312);
#2735=LINE('',#45792,#3313);
#2736=LINE('',#45795,#3314);
#2737=LINE('',#45796,#3315);
#2738=LINE('',#45805,#3316);
#2739=LINE('',#45812,#3317);
#2740=LINE('',#45814,#3318);
#2741=LINE('',#45816,#3319);
#2742=LINE('',#45818,#3320);
#2743=LINE('',#45819,#3321);
#2744=LINE('',#45821,#3322);
#2745=LINE('',#45823,#3323);
#2746=LINE('',#45824,#3324);
#2747=LINE('',#45828,#3325);
#2748=LINE('',#45831,#3326);
#2749=LINE('',#45832,#3327);
#2750=LINE('',#45834,#3328);
#2751=LINE('',#45837,#3329);
#2752=LINE('',#45840,#3330);
#2753=LINE('',#45842,#3331);
#2754=LINE('',#45845,#3332);
#2755=LINE('',#45851,#3333);
#2756=LINE('',#45853,#3334);
#2757=LINE('',#45854,#3335);
#2758=LINE('',#45857,#3336);
#2759=LINE('',#45859,#3337);
#2760=LINE('',#45860,#3338);
#2761=LINE('',#45866,#3339);
#2762=LINE('',#45868,#3340);
#2763=LINE('',#45869,#3341);
#2764=LINE('',#45877,#3342);
#2765=LINE('',#45882,#3343);
#2766=LINE('',#45889,#3344);
#2767=LINE('',#45932,#3345);
#2768=LINE('',#46012,#3346);
#2769=LINE('',#46088,#3347);
#2770=LINE('',#46164,#3348);
#2771=LINE('',#46240,#3349);
#2772=LINE('',#46316,#3350);
#2773=LINE('',#46392,#3351);
#2774=LINE('',#46468,#3352);
#2775=LINE('',#46548,#3353);
#2776=LINE('',#46624,#3354);
#2777=LINE('',#46700,#3355);
#2778=LINE('',#46776,#3356);
#2779=LINE('',#46852,#3357);
#2780=LINE('',#46928,#3358);
#2781=LINE('',#47006,#3359);
#2782=LINE('',#47051,#3360);
#2783=LINE('',#47129,#3361);
#2784=LINE('',#47205,#3362);
#2785=LINE('',#47281,#3363);
#2786=LINE('',#47357,#3364);
#2787=LINE('',#47433,#3365);
#2788=LINE('',#47511,#3366);
#2789=LINE('',#47587,#3367);
#2790=LINE('',#47665,#3368);
#2791=LINE('',#47741,#3369);
#2792=LINE('',#47817,#3370);
#2793=LINE('',#47893,#3371);
#2794=LINE('',#47969,#3372);
#2795=LINE('',#48047,#3373);
#2796=LINE('',#48123,#3374);
#2797=LINE('',#48315,#3375);
#2798=LINE('',#48349,#3376);
#2799=LINE('',#49236,#3377);
#2800=LINE('',#49238,#3378);
#2801=LINE('',#49240,#3379);
#2802=LINE('',#49242,#3380);
#2803=LINE('',#49244,#3381);
#2804=LINE('',#49245,#3382);
#2805=LINE('',#49247,#3383);
#2806=LINE('',#49248,#3384);
#2807=LINE('',#49250,#3385);
#2808=LINE('',#49252,#3386);
#2809=LINE('',#49254,#3387);
#2810=LINE('',#49256,#3388);
#2811=LINE('',#49266,#3389);
#2812=LINE('',#49277,#3390);
#2813=LINE('',#49284,#3391);
#2814=LINE('',#49296,#3392);
#2815=LINE('',#49304,#3393);
#2816=LINE('',#49343,#3394);
#2817=LINE('',#49607,#3395);
#2818=LINE('',#49611,#3396);
#2819=LINE('',#49781,#3397);
#2820=LINE('',#50017,#3398);
#2821=VECTOR('',#11043,0.00125);
#2822=VECTOR('',#11060,0.000375);
#2823=VECTOR('',#11075,0.000375);
#2824=VECTOR('',#11088,0.000375);
#2825=VECTOR('',#11103,0.000375);
#2826=VECTOR('',#11124,1.);
#2827=VECTOR('',#11127,1.);
#2828=VECTOR('',#11130,1.);
#2829=VECTOR('',#11133,1.);
#2830=VECTOR('',#11136,1.);
#2831=VECTOR('',#11139,1.);
#2832=VECTOR('',#11142,1.);
#2833=VECTOR('',#11145,1.);
#2834=VECTOR('',#11148,0.00245);
#2835=VECTOR('',#11159,0.002);
#2836=VECTOR('',#11164,1.);
#2837=VECTOR('',#11167,1.);
#2838=VECTOR('',#11170,1.);
#2839=VECTOR('',#11173,1.);
#2840=VECTOR('',#11180,1.);
#2841=VECTOR('',#11183,1.);
#2842=VECTOR('',#11186,1.);
#2843=VECTOR('',#11189,1.);
#2844=VECTOR('',#11196,1.);
#2845=VECTOR('',#11199,1.);
#2846=VECTOR('',#11202,1.);
#2847=VECTOR('',#11205,1.);
#2848=VECTOR('',#11212,1.);
#2849=VECTOR('',#11215,1.);
#2850=VECTOR('',#11218,1.);
#2851=VECTOR('',#11221,1.);
#2852=VECTOR('',#11232,1.);
#2853=VECTOR('',#11233,1.);
#2854=VECTOR('',#11242,1.);
#2855=VECTOR('',#11245,1.);
#2856=VECTOR('',#11248,1.);
#2857=VECTOR('',#11249,1.);
#2858=VECTOR('',#11252,1.);
#2859=VECTOR('',#11257,1.);
#2860=VECTOR('',#11258,1.);
#2861=VECTOR('',#11263,1.);
#2862=VECTOR('',#11266,1.);
#2863=VECTOR('',#11269,1.);
#2864=VECTOR('',#11270,1.);
#2865=VECTOR('',#11275,1.);
#2866=VECTOR('',#11282,1.);
#2867=VECTOR('',#11289,1.);
#2868=VECTOR('',#11292,1.);
#2869=VECTOR('',#11293,1.);
#2870=VECTOR('',#11296,1.);
#2871=VECTOR('',#11299,1.);
#2872=VECTOR('',#11300,1.);
#2873=VECTOR('',#11305,1.);
#2874=VECTOR('',#11314,1.);
#2875=VECTOR('',#11315,1.);
#2876=VECTOR('',#11316,1.);
#2877=VECTOR('',#11325,1.);
#2878=VECTOR('',#11328,1.);
#2879=VECTOR('',#11329,1.);
#2880=VECTOR('',#11332,1.);
#2881=VECTOR('',#11337,1.);
#2882=VECTOR('',#11338,1.);
#2883=VECTOR('',#11339,1.);
#2884=VECTOR('',#11350,1.);
#2885=VECTOR('',#11353,1.);
#2886=VECTOR('',#11354,1.);
#2887=VECTOR('',#11357,1.);
#2888=VECTOR('',#11360,1.);
#2889=VECTOR('',#11361,1.);
#2890=VECTOR('',#11362,1.);
#2891=VECTOR('',#11371,1.);
#2892=VECTOR('',#11374,1.);
#2893=VECTOR('',#11375,1.);
#2894=VECTOR('',#11378,1.);
#2895=VECTOR('',#11381,1.);
#2896=VECTOR('',#11384,1.);
#2897=VECTOR('',#11387,1.);
#2898=VECTOR('',#11390,1.);
#2899=VECTOR('',#11393,1.);
#2900=VECTOR('',#11396,1.);
#2901=VECTOR('',#11399,1.);
#2902=VECTOR('',#11402,1.);
#2903=VECTOR('',#11413,0.00345);
#2904=VECTOR('',#11416,1.);
#2905=VECTOR('',#11419,1.);
#2906=VECTOR('',#11428,1.);
#2907=VECTOR('',#11433,1.);
#2908=VECTOR('',#11438,1.);
#2909=VECTOR('',#11461,0.0041);
#2910=VECTOR('',#11470,0.004);
#2911=VECTOR('',#11479,0.0079);
#2912=VECTOR('',#11484,0.008);
#2913=VECTOR('',#11493,0.0079);
#2914=VECTOR('',#11498,0.00305);
#2915=VECTOR('',#11503,0.0021);
#2916=VECTOR('',#11512,0.0023);
#2917=VECTOR('',#11607,0.01115);
#2918=VECTOR('',#11610,0.01115);
#2919=VECTOR('',#11613,0.01115);
#2920=VECTOR('',#11616,0.01115);
#2921=VECTOR('',#11619,0.01115);
#2922=VECTOR('',#11622,0.01115);
#2923=VECTOR('',#11625,0.01115);
#2924=VECTOR('',#11628,0.01115);
#2925=VECTOR('',#11631,0.0045);
#2926=VECTOR('',#11636,0.0045);
#2927=VECTOR('',#11639,0.0045);
#2928=VECTOR('',#11642,0.0045);
#2929=VECTOR('',#11645,0.0045);
#2930=VECTOR('',#11648,0.0045);
#2931=VECTOR('',#11651,0.0045);
#2932=VECTOR('',#11658,0.0045);
#2933=VECTOR('',#11665,0.0045);
#2934=VECTOR('',#11672,0.0045);
#2935=VECTOR('',#11679,0.0045);
#2936=VECTOR('',#11684,0.0045);
#2937=VECTOR('',#11693,0.01115);
#2938=VECTOR('',#11704,0.01115);
#2939=VECTOR('',#11715,0.01115);
#2940=VECTOR('',#11726,0.008);
#2941=VECTOR('',#11739,0.008);
#2942=VECTOR('',#11744,0.006);
#2943=VECTOR('',#11749,1.);
#2944=VECTOR('',#11750,1.);
#2945=VECTOR('',#11753,1.);
#2946=VECTOR('',#11756,1.);
#2947=VECTOR('',#11763,1.);
#2948=VECTOR('',#11764,1.);
#2949=VECTOR('',#11765,1.);
#2950=VECTOR('',#11770,1.);
#2951=VECTOR('',#11773,1.);
#2952=VECTOR('',#11776,1.);
#2953=VECTOR('',#11781,1.);
#2954=VECTOR('',#11782,1.);
#2955=VECTOR('',#11783,1.);
#2956=VECTOR('',#11786,1.);
#2957=VECTOR('',#11787,1.);
#2958=VECTOR('',#11788,1.);
#2959=VECTOR('',#11789,1.);
#2960=VECTOR('',#11792,1.);
#2961=VECTOR('',#11793,1.);
#2962=VECTOR('',#11794,1.);
#2963=VECTOR('',#11795,1.);
#2964=VECTOR('',#11798,1.);
#2965=VECTOR('',#11799,1.);
#2966=VECTOR('',#11800,1.);
#2967=VECTOR('',#11801,1.);
#2968=VECTOR('',#11804,1.);
#2969=VECTOR('',#11805,1.);
#2970=VECTOR('',#11816,1.);
#2971=VECTOR('',#11821,1.);
#2972=VECTOR('',#11822,1.);
#2973=VECTOR('',#11825,1.);
#2974=VECTOR('',#11826,1.);
#2975=VECTOR('',#11841,0.00075);
#2976=VECTOR('',#11856,0.00075);
#2977=VECTOR('',#11865,0.000375);
#2978=VECTOR('',#11880,0.000375);
#2979=VECTOR('',#11893,0.000375);
#2980=VECTOR('',#11908,0.000375);
#2981=VECTOR('',#11919,0.001543);
#2982=VECTOR('',#11922,0.001543);
#2983=VECTOR('',#11925,0.001543);
#2984=VECTOR('',#11928,0.001543);
#2985=VECTOR('',#11931,0.001543);
#2986=VECTOR('',#11934,0.001543);
#2987=VECTOR('',#11937,0.001543);
#2988=VECTOR('',#11940,0.001543);
#2989=VECTOR('',#11945,0.001543);
#2990=VECTOR('',#11950,0.001543);
#2991=VECTOR('',#11953,0.001543);
#2992=VECTOR('',#11956,0.001543);
#2993=VECTOR('',#11959,0.001543);
#2994=VECTOR('',#11962,0.001543);
#2995=VECTOR('',#11965,0.001543);
#2996=VECTOR('',#11968,0.001543);
#2997=VECTOR('',#11971,0.001543);
#2998=VECTOR('',#11974,0.001543);
#2999=VECTOR('',#11977,0.001543);
#3000=VECTOR('',#11980,0.001543);
#3001=VECTOR('',#11983,0.001543);
#3002=VECTOR('',#11988,0.0012645);
#3003=VECTOR('',#11991,0.0012645);
#3004=VECTOR('',#11994,0.0012645);
#3005=VECTOR('',#11997,0.0012645);
#3006=VECTOR('',#12000,0.0012645);
#3007=VECTOR('',#12003,0.0012645);
#3008=VECTOR('',#12006,0.0012645);
#3009=VECTOR('',#12011,0.0012645);
#3010=VECTOR('',#12016,0.0012645);
#3011=VECTOR('',#12019,0.0012645);
#3012=VECTOR('',#12022,0.0012645);
#3013=VECTOR('',#12025,0.0012645);
#3014=VECTOR('',#12028,0.0012645);
#3015=VECTOR('',#12031,0.0012645);
#3016=VECTOR('',#12034,0.0012645);
#3017=VECTOR('',#12037,0.0012645);
#3018=VECTOR('',#12040,0.0012645);
#3019=VECTOR('',#12043,0.0012645);
#3020=VECTOR('',#12046,0.0012645);
#3021=VECTOR('',#12055,1.);
#3022=VECTOR('',#12056,1.);
#3023=VECTOR('',#12057,1.);
#3024=VECTOR('',#12058,1.);
#3025=VECTOR('',#12061,1.);
#3026=VECTOR('',#12062,1.);
#3027=VECTOR('',#12063,1.);
#3028=VECTOR('',#12066,1.);
#3029=VECTOR('',#12067,1.);
#3030=VECTOR('',#12068,1.);
#3031=VECTOR('',#12071,1.);
#3032=VECTOR('',#12072,1.);
#3033=VECTOR('',#12073,1.);
#3034=VECTOR('',#12074,1.);
#3035=VECTOR('',#12079,1.);
#3036=VECTOR('',#12080,1.);
#3037=VECTOR('',#12083,1.);
#3038=VECTOR('',#12084,1.);
#3039=VECTOR('',#12085,1.);
#3040=VECTOR('',#12086,1.);
#3041=VECTOR('',#12097,1.);
#3042=VECTOR('',#12100,1.);
#3043=VECTOR('',#12105,1.);
#3044=VECTOR('',#12106,1.);
#3045=VECTOR('',#12109,1.);
#3046=VECTOR('',#12110,1.);
#3047=VECTOR('',#12111,1.);
#3048=VECTOR('',#12112,1.);
#3049=VECTOR('',#12119,0.0015);
#3050=VECTOR('',#12126,1.);
#3051=VECTOR('',#12135,1.);
#3052=VECTOR('',#12136,1.);
#3053=VECTOR('',#12137,1.);
#3054=VECTOR('',#12138,1.);
#3055=VECTOR('',#12139,1.);
#3056=VECTOR('',#12140,1.);
#3057=VECTOR('',#12147,0.0016);
#3058=VECTOR('',#12154,0.0031);
#3059=VECTOR('',#12159,0.0016);
#3060=VECTOR('',#12162,1.);
#3061=VECTOR('',#12163,1.);
#3062=VECTOR('',#12164,1.);
#3063=VECTOR('',#12167,1.);
#3064=VECTOR('',#12170,1.);
#3065=VECTOR('',#12173,1.);
#3066=VECTOR('',#12174,1.);
#3067=VECTOR('',#12175,1.);
#3068=VECTOR('',#12178,1.);
#3069=VECTOR('',#12179,1.);
#3070=VECTOR('',#12180,1.);
#3071=VECTOR('',#12183,1.);
#3072=VECTOR('',#12184,1.);
#3073=VECTOR('',#12185,1.);
#3074=VECTOR('',#12188,1.);
#3075=VECTOR('',#12189,1.);
#3076=VECTOR('',#12194,0.00175);
#3077=VECTOR('',#12197,1.);
#3078=VECTOR('',#12198,1.);
#3079=VECTOR('',#12199,1.);
#3080=VECTOR('',#12202,1.);
#3081=VECTOR('',#12203,1.);
#3082=VECTOR('',#12206,1.);
#3083=VECTOR('',#12207,1.);
#3084=VECTOR('',#12208,1.);
#3085=VECTOR('',#12213,0.00175);
#3086=VECTOR('',#12228,1.);
#3087=VECTOR('',#12233,1.);
#3088=VECTOR('',#12236,1.);
#3089=VECTOR('',#12237,1.);
#3090=VECTOR('',#12244,1.);
#3091=VECTOR('',#12247,1.);
#3092=VECTOR('',#12252,0.00155);
#3093=VECTOR('',#12255,1.);
#3094=VECTOR('',#12260,1.);
#3095=VECTOR('',#12265,1.);
#3096=VECTOR('',#12268,1.);
#3097=VECTOR('',#12273,0.0031);
#3098=VECTOR('',#12288,0.0016);
#3099=VECTOR('',#12321,0.00025);
#3100=VECTOR('',#12336,0.00025);
#3101=VECTOR('',#12377,0.0011);
#3102=VECTOR('',#12384,0.001);
#3103=VECTOR('',#12393,0.0022);
#3104=VECTOR('',#12402,0.0021);
#3105=VECTOR('',#12407,0.00155);
#3106=VECTOR('',#12412,0.00265);
#3107=VECTOR('',#12415,0.00275);
#3108=VECTOR('',#12426,0.0029);
#3109=VECTOR('',#12443,0.0029);
#3110=VECTOR('',#12450,0.001475);
#3111=VECTOR('',#12457,0.0028);
#3112=VECTOR('',#12464,0.003);
#3113=VECTOR('',#12469,0.0028);
#3114=VECTOR('',#12478,0.0025);
#3115=VECTOR('',#12483,0.0025);
#3116=VECTOR('',#12486,0.0025);
#3117=VECTOR('',#12489,0.0025);
#3118=VECTOR('',#12492,0.0025);
#3119=VECTOR('',#12495,0.0025);
#3120=VECTOR('',#12498,0.0025);
#3121=VECTOR('',#12515,1.);
#3122=VECTOR('',#12516,1.);
#3123=VECTOR('',#12517,1.);
#3124=VECTOR('',#12518,1.);
#3125=VECTOR('',#12519,1.);
#3126=VECTOR('',#12520,1.);
#3127=VECTOR('',#12521,1.);
#3128=VECTOR('',#12522,1.);
#3129=VECTOR('',#12523,1.);
#3130=VECTOR('',#12524,1.);
#3131=VECTOR('',#12525,1.);
#3132=VECTOR('',#12526,1.);
#3133=VECTOR('',#12529,0.00125);
#3134=VECTOR('',#12534,1.);
#3135=VECTOR('',#12535,1.);
#3136=VECTOR('',#12536,1.);
#3137=VECTOR('',#12539,1.);
#3138=VECTOR('',#12540,1.);
#3139=VECTOR('',#12541,1.);
#3140=VECTOR('',#12542,1.);
#3141=VECTOR('',#12543,1.);
#3142=VECTOR('',#12544,1.);
#3143=VECTOR('',#12549,1.);
#3144=VECTOR('',#12550,1.);
#3145=VECTOR('',#12551,1.);
#3146=VECTOR('',#12554,1.);
#3147=VECTOR('',#12555,1.);
#3148=VECTOR('',#12556,1.);
#3149=VECTOR('',#12557,1.);
#3150=VECTOR('',#12558,1.);
#3151=VECTOR('',#12559,1.);
#3152=VECTOR('',#12564,1.);
#3153=VECTOR('',#12565,1.);
#3154=VECTOR('',#12568,1.);
#3155=VECTOR('',#12569,1.);
#3156=VECTOR('',#12570,1.);
#3157=VECTOR('',#12573,1.);
#3158=VECTOR('',#12574,1.);
#3159=VECTOR('',#12575,1.);
#3160=VECTOR('',#12576,1.);
#3161=VECTOR('',#12577,1.);
#3162=VECTOR('',#12578,1.);
#3163=VECTOR('',#12581,1.);
#3164=VECTOR('',#12582,1.);
#3165=VECTOR('',#12585,1.);
#3166=VECTOR('',#12586,1.);
#3167=VECTOR('',#12589,1.);
#3168=VECTOR('',#12590,1.);
#3169=VECTOR('',#12591,1.);
#3170=VECTOR('',#12594,1.);
#3171=VECTOR('',#12595,1.);
#3172=VECTOR('',#12596,1.);
#3173=VECTOR('',#12597,1.);
#3174=VECTOR('',#12598,1.);
#3175=VECTOR('',#12599,1.);
#3176=VECTOR('',#12600,1.);
#3177=VECTOR('',#12601,1.);
#3178=VECTOR('',#12606,1.);
#3179=VECTOR('',#12607,1.);
#3180=VECTOR('',#12610,1.);
#3181=VECTOR('',#12611,1.);
#3182=VECTOR('',#12614,1.);
#3183=VECTOR('',#12615,1.);
#3184=VECTOR('',#12618,1.);
#3185=VECTOR('',#12619,1.);
#3186=VECTOR('',#12622,1.);
#3187=VECTOR('',#12623,1.);
#3188=VECTOR('',#12624,1.);
#3189=VECTOR('',#12631,1.);
#3190=VECTOR('',#12634,1.);
#3191=VECTOR('',#12639,1.);
#3192=VECTOR('',#12642,1.);
#3193=VECTOR('',#12647,1.);
#3194=VECTOR('',#12652,0.00075);
#3195=VECTOR('',#12655,0.00075);
#3196=VECTOR('',#12658,0.00075);
#3197=VECTOR('',#12663,0.0006);
#3198=VECTOR('',#12672,0.0002);
#3199=VECTOR('',#12677,0.0012);
#3200=VECTOR('',#12686,0.001);
#3201=VECTOR('',#12691,0.0024);
#3202=VECTOR('',#12790,1.);
#3203=VECTOR('',#12791,1.);
#3204=VECTOR('',#12800,1.);
#3205=VECTOR('',#12801,1.);
#3206=VECTOR('',#12804,1.);
#3207=VECTOR('',#12805,1.);
#3208=VECTOR('',#12814,1.);
#3209=VECTOR('',#12815,1.);
#3210=VECTOR('',#12824,1.);
#3211=VECTOR('',#12825,1.);
#3212=VECTOR('',#12828,1.);
#3213=VECTOR('',#12829,1.);
#3214=VECTOR('',#12832,1.);
#3215=VECTOR('',#12833,1.);
#3216=VECTOR('',#12836,1.);
#3217=VECTOR('',#12837,1.);
#3218=VECTOR('',#12840,1.);
#3219=VECTOR('',#12841,1.);
#3220=VECTOR('',#12844,1.);
#3221=VECTOR('',#12845,1.);
#3222=VECTOR('',#12846,1.);
#3223=VECTOR('',#12849,1.);
#3224=VECTOR('',#12850,1.);
#3225=VECTOR('',#12853,1.);
#3226=VECTOR('',#12854,1.);
#3227=VECTOR('',#12855,1.);
#3228=VECTOR('',#12856,1.);
#3229=VECTOR('',#12857,1.);
#3230=VECTOR('',#12860,1.);
#3231=VECTOR('',#12861,1.);
#3232=VECTOR('',#12862,1.);
#3233=VECTOR('',#12863,1.);
#3234=VECTOR('',#12864,1.);
#3235=VECTOR('',#12865,1.);
#3236=VECTOR('',#12866,1.);
#3237=VECTOR('',#12867,1.);
#3238=VECTOR('',#12870,1.);
#3239=VECTOR('',#12871,1.);
#3240=VECTOR('',#12872,1.);
#3241=VECTOR('',#12873,1.);
#3242=VECTOR('',#12874,1.);
#3243=VECTOR('',#12885,1.);
#3244=VECTOR('',#12888,1.);
#3245=VECTOR('',#12891,1.);
#3246=VECTOR('',#12892,1.);
#3247=VECTOR('',#12895,1.);
#3248=VECTOR('',#12896,1.);
#3249=VECTOR('',#12897,1.);
#3250=VECTOR('',#12902,1.);
#3251=VECTOR('',#12905,1.);
#3252=VECTOR('',#12908,1.);
#3253=VECTOR('',#12909,1.);
#3254=VECTOR('',#12912,1.);
#3255=VECTOR('',#12913,1.);
#3256=VECTOR('',#12918,1.);
#3257=VECTOR('',#12921,1.);
#3258=VECTOR('',#12924,1.);
#3259=VECTOR('',#12925,1.);
#3260=VECTOR('',#12926,1.);
#3261=VECTOR('',#12927,1.);
#3262=VECTOR('',#12928,1.);
#3263=VECTOR('',#12931,1.);
#3264=VECTOR('',#12936,1.);
#3265=VECTOR('',#12939,1.);
#3266=VECTOR('',#12942,1.);
#3267=VECTOR('',#12943,1.);
#3268=VECTOR('',#12944,1.);
#3269=VECTOR('',#12945,1.);
#3270=VECTOR('',#12946,1.);
#3271=VECTOR('',#12947,1.);
#3272=VECTOR('',#12950,1.);
#3273=VECTOR('',#12951,1.);
#3274=VECTOR('',#12956,1.);
#3275=VECTOR('',#12959,1.);
#3276=VECTOR('',#12962,1.);
#3277=VECTOR('',#12963,1.);
#3278=VECTOR('',#12964,1.);
#3279=VECTOR('',#12967,1.);
#3280=VECTOR('',#12968,1.);
#3281=VECTOR('',#12969,1.);
#3282=VECTOR('',#12970,1.);
#3283=VECTOR('',#12973,1.);
#3284=VECTOR('',#12974,1.);
#3285=VECTOR('',#12975,1.);
#3286=VECTOR('',#12978,1.);
#3287=VECTOR('',#12981,1.);
#3288=VECTOR('',#12982,1.);
#3289=VECTOR('',#12985,1.);
#3290=VECTOR('',#12986,1.);
#3291=VECTOR('',#12987,1.);
#3292=VECTOR('',#12988,1.);
#3293=VECTOR('',#12989,1.);
#3294=VECTOR('',#12992,1.);
#3295=VECTOR('',#12993,1.);
#3296=VECTOR('',#12994,1.);
#3297=VECTOR('',#12995,1.);
#3298=VECTOR('',#12998,1.);
#3299=VECTOR('',#12999,1.);
#3300=VECTOR('',#13002,1.);
#3301=VECTOR('',#13005,1.);
#3302=VECTOR('',#13008,1.);
#3303=VECTOR('',#13009,1.);
#3304=VECTOR('',#13012,1.);
#3305=VECTOR('',#13013,1.);
#3306=VECTOR('',#13016,1.);
#3307=VECTOR('',#13017,1.);
#3308=VECTOR('',#13020,1.);
#3309=VECTOR('',#13021,1.);
#3310=VECTOR('',#13022,1.);
#3311=VECTOR('',#13025,1.);
#3312=VECTOR('',#13030,1.);
#3313=VECTOR('',#13031,1.);
#3314=VECTOR('',#13034,1.);
#3315=VECTOR('',#13035,1.);
#3316=VECTOR('',#13046,0.0041);
#3317=VECTOR('',#13055,1.);
#3318=VECTOR('',#13056,1.);
#3319=VECTOR('',#13057,1.);
#3320=VECTOR('',#13058,1.);
#3321=VECTOR('',#13059,1.);
#3322=VECTOR('',#13062,0.0025);
#3323=VECTOR('',#13065,1.);
#3324=VECTOR('',#13066,1.);
#3325=VECTOR('',#13071,1.);
#3326=VECTOR('',#13074,1.);
#3327=VECTOR('',#13075,1.);
#3328=VECTOR('',#13076,1.);
#3329=VECTOR('',#13081,1.);
#3330=VECTOR('',#13086,1.);
#3331=VECTOR('',#13089,1.);
#3332=VECTOR('',#13094,1.);
#3333=VECTOR('',#13101,1.);
#3334=VECTOR('',#13104,1.);
#3335=VECTOR('',#13105,1.);
#3336=VECTOR('',#13108,1.);
#3337=VECTOR('',#13109,1.);
#3338=VECTOR('',#13110,1.);
#3339=VECTOR('',#13117,1.);
#3340=VECTOR('',#13120,1.);
#3341=VECTOR('',#13121,1.);
#3342=VECTOR('',#13132,0.0013);
#3343=VECTOR('',#13139,0.0015);
#3344=VECTOR('',#13148,0.0015);
#3345=VECTOR('',#13153,0.0015);
#3346=VECTOR('',#13156,0.0015);
#3347=VECTOR('',#13159,0.0015);
#3348=VECTOR('',#13162,0.0015);
#3349=VECTOR('',#13165,0.0015);
#3350=VECTOR('',#13168,0.0015);
#3351=VECTOR('',#13171,0.0015);
#3352=VECTOR('',#13174,0.0015);
#3353=VECTOR('',#13177,0.0015);
#3354=VECTOR('',#13180,0.0015);
#3355=VECTOR('',#13183,0.0015);
#3356=VECTOR('',#13186,0.0015);
#3357=VECTOR('',#13189,0.0015);
#3358=VECTOR('',#13192,0.0015);
#3359=VECTOR('',#13195,0.00117524047358083);
#3360=VECTOR('',#13200,0.00117524047358083);
#3361=VECTOR('',#13203,0.00117524047358083);
#3362=VECTOR('',#13206,0.00117524047358083);
#3363=VECTOR('',#13209,0.00117524047358083);
#3364=VECTOR('',#13212,0.00117524047358083);
#3365=VECTOR('',#13215,0.00117524047358083);
#3366=VECTOR('',#13218,0.00117524047358083);
#3367=VECTOR('',#13221,0.00117524047358083);
#3368=VECTOR('',#13224,0.00117524047358083);
#3369=VECTOR('',#13227,0.00117524047358083);
#3370=VECTOR('',#13230,0.00117524047358083);
#3371=VECTOR('',#13233,0.00117524047358083);
#3372=VECTOR('',#13236,0.00117524047358083);
#3373=VECTOR('',#13239,0.00117524047358083);
#3374=VECTOR('',#13242,0.00117524047358083);
#3375=VECTOR('',#13259,0.00285);
#3376=VECTOR('',#13268,0.001125);
#3377=VECTOR('',#13299,0.999999999999998);
#3378=VECTOR('',#13300,1.);
#3379=VECTOR('',#13301,0.999999999999998);
#3380=VECTOR('',#13302,0.999999999999998);
#3381=VECTOR('',#13303,1.);
#3382=VECTOR('',#13304,0.999999999999998);
#3383=VECTOR('',#13307,1.);
#3384=VECTOR('',#13308,1.);
#3385=VECTOR('',#13311,1.);
#3386=VECTOR('',#13314,1.);
#3387=VECTOR('',#13317,1.);
#3388=VECTOR('',#13320,1.);
#3389=VECTOR('',#13333,0.00075);
#3390=VECTOR('',#13348,0.00075);
#3391=VECTOR('',#13357,0.00025);
#3392=VECTOR('',#13372,0.00025);
#3393=VECTOR('',#13383,0.004442);
#3394=VECTOR('',#13388,0.003872);
#3395=VECTOR('',#13403,0.0027);
#3396=VECTOR('',#13408,0.0025);
#3397=VECTOR('',#13415,0.0027);
#3398=VECTOR('',#13430,0.0039);
#3399=CIRCLE('',#10109,0.00125000000001);
#3400=CIRCLE('',#10110,0.00125000000001);
#3401=CIRCLE('',#10115,0.00037500000001);
#3402=CIRCLE('',#10117,0.00037500000001);
#3403=CIRCLE('',#10118,0.00037500000001);
#3404=CIRCLE('',#10119,0.00037500000001);
#3405=CIRCLE('',#10121,0.002625);
#3406=CIRCLE('',#10122,0.00037500000001);
#3407=CIRCLE('',#10123,0.00037500000001);
#3408=CIRCLE('',#10128,0.00037500000001);
#3409=CIRCLE('',#10130,0.00037500000001);
#3410=CIRCLE('',#10131,0.00037500000001);
#3411=CIRCLE('',#10132,0.00037500000001);
#3412=CIRCLE('',#10134,0.002625);
#3413=CIRCLE('',#10135,0.00037500000001);
#3414=CIRCLE('',#10136,0.00037500000001);
#3415=CIRCLE('',#10141,0.0028500000000131);
#3416=CIRCLE('',#10142,0.0004);
#3417=CIRCLE('',#10143,0.00245000000001309);
#3418=CIRCLE('',#10145,0.00345000000001);
#3419=CIRCLE('',#10147,0.00245000000001);
#3420=CIRCLE('',#10148,0.00245000000001);
#3421=CIRCLE('',#10149,0.00245000000001);
#3422=CIRCLE('',#10150,0.00245000000001);
#3423=CIRCLE('',#10151,0.00245000000001);
#3424=CIRCLE('',#10152,0.00245000000001);
#3425=CIRCLE('',#10153,0.00245000000001);
#3426=CIRCLE('',#10154,0.00245000000001);
#3427=CIRCLE('',#10155,0.00245000000001);
#3428=CIRCLE('',#10157,0.00200000000001);
#3429=CIRCLE('',#10158,0.0004);
#3430=CIRCLE('',#10159,0.00240000000001);
#3431=CIRCLE('',#10161,0.00200000000001);
#3432=CIRCLE('',#10164,0.00200000000001);
#3433=CIRCLE('',#10167,0.00200000000001);
#3434=CIRCLE('',#10170,0.00200000000001);
#3435=CIRCLE('',#10173,0.00200000000001);
#3436=CIRCLE('',#10176,0.00200000000001);
#3437=CIRCLE('',#10179,0.00200000000001);
#3438=CIRCLE('',#10182,0.00200000000001);
#3439=CIRCLE('',#10185,0.00200000000001);
#3440=CIRCLE('',#10187,0.00345000000001);
#3441=CIRCLE('',#10190,0.00235000000001);
#3442=CIRCLE('',#10191,0.00285000000001);
#3443=CIRCLE('',#10196,0.00235000000001);
#3444=CIRCLE('',#10199,0.00235000000001);
#3445=CIRCLE('',#10203,0.00235000000001);
#3446=CIRCLE('',#10205,0.00285000000001);
#3447=CIRCLE('',#10208,0.00285000000001);
#3448=CIRCLE('',#10212,0.481704687282423);
#3449=CIRCLE('',#10214,0.00255000000001);
#3450=CIRCLE('',#10216,0.00285000000001);
#3451=CIRCLE('',#10217,0.481704687282423);
#3452=CIRCLE('',#10220,0.00255000000001);
#3453=CIRCLE('',#10221,0.00285000000001);
#3454=CIRCLE('',#10226,0.481704687282423);
#3455=CIRCLE('',#10228,0.00255000000001);
#3456=CIRCLE('',#10229,0.481704687282423);
#3457=CIRCLE('',#10230,0.00285000000001);
#3458=CIRCLE('',#10236,0.00255000000001);
#3459=CIRCLE('',#10237,0.00285000000001);
#3460=CIRCLE('',#10258,0.00285000000001);
#3461=CIRCLE('',#10267,0.00307350000001);
#3462=CIRCLE('',#10268,0.00307350000001);
#3463=CIRCLE('',#10270,0.00251750000001);
#3464=CIRCLE('',#10271,0.00251750000001);
#3465=CIRCLE('',#10272,0.00251750000001);
#3466=CIRCLE('',#10274,0.00400000000001);
#3467=CIRCLE('',#10275,0.00420000000001);
#3468=CIRCLE('',#10277,0.00780000000001);
#3469=CIRCLE('',#10279,0.00400000000001);
#3470=CIRCLE('',#10280,0.00400000000001);
#3471=CIRCLE('',#10282,0.00800000000001);
#3472=CIRCLE('',#10283,0.00780000000001);
#3473=CIRCLE('',#10285,0.00800000000001);
#3474=CIRCLE('',#10287,0.00600000000001);
#3475=CIRCLE('',#10290,0.00210000000001);
#3476=CIRCLE('',#10291,0.00210000000001);
#3477=CIRCLE('',#10293,0.00210000000001);
#3478=CIRCLE('',#10294,0.00210000000001);
#3479=CIRCLE('',#10298,0.01115000000001);
#3480=CIRCLE('',#10299,0.0060198255992182);
#3481=CIRCLE('',#10301,0.01115000000001);
#3482=CIRCLE('',#10302,0.00588880615101059);
#3483=CIRCLE('',#10304,0.01115000000001);
#3484=CIRCLE('',#10305,0.00594121393029363);
#3485=CIRCLE('',#10307,0.01115000000001);
#3486=CIRCLE('',#10308,0.00575778670280299);
#3487=CIRCLE('',#10310,0.01115000000001);
#3488=CIRCLE('',#10311,0.00581019448208603);
#3489=CIRCLE('',#10313,0.01115000000001);
#3490=CIRCLE('',#10314,0.00562676725459539);
#3491=CIRCLE('',#10316,0.01115000000001);
#3492=CIRCLE('',#10317,0.00567917503387843);
#3493=CIRCLE('',#10319,0.01115000000001);
#3494=CIRCLE('',#10320,0.00549574780638778);
#3495=CIRCLE('',#10322,0.01115000000001);
#3496=CIRCLE('',#10323,0.00554815558567082);
#3497=CIRCLE('',#10325,0.01115000000001);
#3498=CIRCLE('',#10326,0.00536472835818018);
#3499=CIRCLE('',#10328,0.01115000000001);
#3500=CIRCLE('',#10329,0.00541713613746322);
#3501=CIRCLE('',#10331,0.01115000000001);
#3502=CIRCLE('',#10332,0.00523370890997258);
#3503=CIRCLE('',#10334,0.01115000000001);
#3504=CIRCLE('',#10335,0.00528611668925562);
#3505=CIRCLE('',#10337,0.01115000000001);
#3506=CIRCLE('',#10338,0.00515509724104802);
#3507=CIRCLE('',#10340,0.01115000000001);
#3508=CIRCLE('',#10341,0.00510268946176497);
#3509=CIRCLE('',#10343,0.01115000000001);
#3510=CIRCLE('',#10352,0.00502407779284041);
#3511=CIRCLE('',#10361,0.00470963111714216);
#3512=CIRCLE('',#10362,0.0046310194482176);
#3513=CIRCLE('',#10364,0.00457861166893456);
#3514=CIRCLE('',#10365,0.00450000000001);
#3515=CIRCLE('',#10367,0.00484065056534977);
#3516=CIRCLE('',#10368,0.00476203889642521);
#3517=CIRCLE('',#10370,0.00497167001355737);
#3518=CIRCLE('',#10371,0.00489305834463281);
#3519=CIRCLE('',#10374,0.01115000000001);
#3520=CIRCLE('',#10376,0.01115000000001);
#3521=CIRCLE('',#10379,0.01115000000001);
#3522=CIRCLE('',#10381,0.01115000000001);
#3523=CIRCLE('',#10384,0.01115000000001);
#3524=CIRCLE('',#10386,0.01115000000001);
#3525=CIRCLE('',#10389,0.00800000000001);
#3526=CIRCLE('',#10391,0.00800000000001);
#3527=CIRCLE('',#10394,0.00800000000001);
#3528=CIRCLE('',#10395,0.00600000000001);
#3529=CIRCLE('',#10397,0.00800000000001);
#3530=CIRCLE('',#10404,0.00387500000001);
#3531=CIRCLE('',#10408,0.00387500000001);
#3532=CIRCLE('',#10410,0.00387500000001);
#3533=CIRCLE('',#10411,0.00387500000001);
#3534=CIRCLE('',#10418,0.00245000000001);
#3535=CIRCLE('',#10419,0.00245000000001);
#3536=CIRCLE('',#10421,0.00387500000001);
#3537=CIRCLE('',#10422,0.00387500000001);
#3538=CIRCLE('',#10429,0.00075000000001);
#3539=CIRCLE('',#10431,0.00075000000001);
#3540=CIRCLE('',#10432,0.00075000000001);
#3541=CIRCLE('',#10433,0.00075000000001);
#3542=CIRCLE('',#10435,0.00225);
#3543=CIRCLE('',#10436,0.00075000000001);
#3544=CIRCLE('',#10437,0.00075000000001);
#3545=CIRCLE('',#10442,0.00037500000001);
#3546=CIRCLE('',#10443,0.00037500000001);
#3547=CIRCLE('',#10444,0.00037500000001);
#3548=CIRCLE('',#10446,0.002625);
#3549=CIRCLE('',#10447,0.00037500000001);
#3550=CIRCLE('',#10448,0.00037500000001);
#3551=CIRCLE('',#10450,0.00037500000001);
#3552=CIRCLE('',#10455,0.00037500000001);
#3553=CIRCLE('',#10456,0.00037500000001);
#3554=CIRCLE('',#10457,0.00037500000001);
#3555=CIRCLE('',#10459,0.002625);
#3556=CIRCLE('',#10460,0.00037500000001);
#3557=CIRCLE('',#10461,0.00037500000001);
#3558=CIRCLE('',#10463,0.00037500000001);
#3559=CIRCLE('',#10475,0.00154300000001001);
#3560=CIRCLE('',#10477,0.00154300000001);
#3561=CIRCLE('',#10490,0.00154300000001);
#3562=CIRCLE('',#10498,0.00126450000001);
#3563=CIRCLE('',#10500,0.00126450000001);
#3564=CIRCLE('',#10512,0.00126450000001);
#3565=CIRCLE('',#10519,0.00150000000001);
#3566=CIRCLE('',#10522,0.00170000000001);
#3567=CIRCLE('',#10523,0.00170000000001);
#3568=CIRCLE('',#10524,0.00320000000001);
#3569=CIRCLE('',#10525,0.00170000000001);
#3570=CIRCLE('',#10529,0.00195000000001);
#3571=CIRCLE('',#10530,0.00340000000001);
#3572=CIRCLE('',#10531,0.00195000000001);
#3573=CIRCLE('',#10533,0.00150000000001);
#3574=CIRCLE('',#10535,0.00300000000001);
#3575=CIRCLE('',#10536,0.00300000000001);
#3576=CIRCLE('',#10538,0.00340000000001);
#3577=CIRCLE('',#10540,0.00195000000001);
#3578=CIRCLE('',#10541,0.00195000000001);
#3579=CIRCLE('',#10545,0.00250000000001);
#3580=CIRCLE('',#10546,0.00250000000001);
#3581=CIRCLE('',#10548,0.00126450000001);
#3582=CIRCLE('',#10557,0.00155000000001);
#3583=CIRCLE('',#10562,0.00155000000001);
#3584=CIRCLE('',#10564,0.00250000000001);
#3585=CIRCLE('',#10566,0.00300000000001);
#3586=CIRCLE('',#10573,0.00320000000001);
#3587=CIRCLE('',#10574,0.00170000000001);
#3588=CIRCLE('',#10586,0.00250000000001);
#3589=CIRCLE('',#10587,0.00250000000001);
#3590=CIRCLE('',#10589,0.00300000000001);
#3591=CIRCLE('',#10593,0.00126450000001);
#3592=CIRCLE('',#10594,0.00126450000001);
#3593=CIRCLE('',#10598,0.00154300000001001);
#3594=CIRCLE('',#10609,0.00025000000001);
#3595=CIRCLE('',#10610,0.00025000000001);
#3596=CIRCLE('',#10611,0.00025000000001);
#3597=CIRCLE('',#10613,0.00275);
#3598=CIRCLE('',#10614,0.00025000000001);
#3599=CIRCLE('',#10615,0.00025000000001);
#3600=CIRCLE('',#10617,0.00025000000001);
#3601=CIRCLE('',#10622,0.00251045773724889);
#3602=CIRCLE('',#10623,0.00250000000001);
#3603=CIRCLE('',#10624,0.00250000000001);
#3604=CIRCLE('',#10626,0.00300000000001);
#3605=CIRCLE('',#10627,0.00300000000001);
#3606=CIRCLE('',#10629,0.00251044841467262);
#3607=CIRCLE('',#10630,0.00250000000001);
#3608=CIRCLE('',#10631,0.00250000000001);
#3609=CIRCLE('',#10633,0.00300000000001);
#3610=CIRCLE('',#10634,0.00300000000001);
#3611=CIRCLE('',#10636,0.00100000000001);
#3612=CIRCLE('',#10637,0.00120000000001);
#3613=CIRCLE('',#10639,0.00100000000001);
#3614=CIRCLE('',#10641,0.00280000000001);
#3615=CIRCLE('',#10643,0.00210000000001);
#3616=CIRCLE('',#10644,0.00230000000001);
#3617=CIRCLE('',#10646,0.00255000000001);
#3618=CIRCLE('',#10648,0.00210000000001);
#3619=CIRCLE('',#10651,0.00275000000001);
#3620=CIRCLE('',#10653,0.00275000000001);
#3621=CIRCLE('',#10655,0.00300000000001);
#3622=CIRCLE('',#10656,0.00300000000001);
#3623=CIRCLE('',#10658,0.00280000000001);
#3624=CIRCLE('',#10661,0.00300000000001);
#3625=CIRCLE('',#10662,0.00300000000001);
#3626=CIRCLE('',#10664,0.00147500000001);
#3627=CIRCLE('',#10667,0.00147500000001);
#3628=CIRCLE('',#10671,0.00300000000001);
#3629=CIRCLE('',#10672,0.00260000000001);
#3630=CIRCLE('',#10674,0.00300000000001);
#3631=CIRCLE('',#10677,0.00260000000001);
#3632=CIRCLE('',#10681,0.00250000000001);
#3633=CIRCLE('',#10687,0.00250000000001);
#3634=CIRCLE('',#10688,0.00250000000001);
#3635=CIRCLE('',#10689,0.00215000000001);
#3636=CIRCLE('',#10692,0.00200000000001);
#3637=CIRCLE('',#10693,0.00200000000001);
#3638=CIRCLE('',#10694,0.00215000000001);
#3639=CIRCLE('',#10697,0.00050000000001);
#3640=CIRCLE('',#10700,0.00075000000001366);
#3641=CIRCLE('',#10703,0.00075000000001);
#3642=CIRCLE('',#10711,0.00270000000001);
#3643=CIRCLE('',#10717,0.00075000000001366);
#3644=CIRCLE('',#10731,0.00020000000001);
#3645=CIRCLE('',#10732,0.00100000000001);
#3646=CIRCLE('',#10733,0.00100000000001);
#3647=CIRCLE('',#10735,0.00020000000001);
#3648=CIRCLE('',#10737,0.00100000000001);
#3649=CIRCLE('',#10738,0.00140000000001);
#3650=CIRCLE('',#10740,0.00230000000001);
#3651=CIRCLE('',#10743,0.00250000000001);
#3652=CIRCLE('',#10744,0.00250000000001);
#3653=CIRCLE('',#10749,0.000749886741462474);
#3654=CIRCLE('',#10750,0.00075000000001);
#3655=CIRCLE('',#10751,0.00075000000001);
#3656=CIRCLE('',#10752,0.000749886741462474);
#3657=CIRCLE('',#10753,0.000749886741462474);
#3658=CIRCLE('',#10754,0.00075000000001);
#3659=CIRCLE('',#10755,0.00075000000001);
#3660=CIRCLE('',#10756,0.000749886741462474);
#3661=CIRCLE('',#10757,0.000749886741462474);
#3662=CIRCLE('',#10758,0.00075000000001);
#3663=CIRCLE('',#10759,0.000749886741462473);
#3664=CIRCLE('',#10760,0.000750000000010001);
#3665=CIRCLE('',#10761,0.00075000000001);
#3666=CIRCLE('',#10762,0.000749886741462473);
#3667=CIRCLE('',#10763,0.000749886741462478);
#3668=CIRCLE('',#10764,0.00075000000001);
#3669=CIRCLE('',#10765,0.000750000000010002);
#3670=CIRCLE('',#10766,0.000749886741462478);
#3671=CIRCLE('',#10767,0.000749886741462476);
#3672=CIRCLE('',#10768,0.000750000000010002);
#3673=CIRCLE('',#10769,0.000749886741462477);
#3674=CIRCLE('',#10770,0.00075000000001);
#3675=CIRCLE('',#10771,0.00075000000001);
#3676=CIRCLE('',#10772,0.000749886741462477);
#3677=CIRCLE('',#10773,0.000749886741462475);
#3678=CIRCLE('',#10774,0.00075000000001);
#3679=CIRCLE('',#10775,0.000750000000010001);
#3680=CIRCLE('',#10776,0.000749886741462475);
#3681=CIRCLE('',#10777,0.000749886741462475);
#3682=CIRCLE('',#10778,0.000750000000010001);
#3683=CIRCLE('',#10779,0.000749886741462475);
#3684=CIRCLE('',#10780,0.000750000000010002);
#3685=CIRCLE('',#10781,0.00075000000001);
#3686=CIRCLE('',#10782,0.000749886741462475);
#3687=CIRCLE('',#10783,0.000749886741462478);
#3688=CIRCLE('',#10784,0.00075000000001);
#3689=CIRCLE('',#10785,0.00075000000001);
#3690=CIRCLE('',#10786,0.000749886741462478);
#3691=CIRCLE('',#10787,0.000749886741462473);
#3692=CIRCLE('',#10788,0.00075000000001);
#3693=CIRCLE('',#10789,0.000750000000010002);
#3694=CIRCLE('',#10790,0.000749886741462473);
#3695=CIRCLE('',#10792,0.000750000000014142);
#3696=CIRCLE('',#10793,0.00075000000001);
#3697=CIRCLE('',#10794,0.000749886741462475);
#3698=CIRCLE('',#10796,0.000750000000014142);
#3699=CIRCLE('',#10798,0.000750000000010001);
#3700=CIRCLE('',#10799,0.000749886741462476);
#3701=CIRCLE('',#10801,0.000750000000014142);
#3702=CIRCLE('',#10802,0.00075000000001);
#3703=CIRCLE('',#10803,0.000749886741462474);
#3704=CIRCLE('',#10805,0.000750000000014142);
#3705=CIRCLE('',#10810,0.00300000000001);
#3706=CIRCLE('',#10811,0.00155000000001);
#3707=CIRCLE('',#10816,0.00685000000001);
#3708=CIRCLE('',#10817,0.00250000000001);
#3709=CIRCLE('',#10819,0.00100000000001414);
#3710=CIRCLE('',#10820,0.00100000000001414);
#3711=CIRCLE('',#10824,0.00100000000001414);
#3712=CIRCLE('',#10825,0.00100000000001414);
#3713=CIRCLE('',#10829,0.00100000000001414);
#3714=CIRCLE('',#10830,0.00100000000001414);
#3715=CIRCLE('',#10834,0.00100000000001414);
#3716=CIRCLE('',#10835,0.00100000000001414);
#3717=CIRCLE('',#10839,0.00100000000001414);
#3718=CIRCLE('',#10840,0.00100000000001414);
#3719=CIRCLE('',#10860,0.0016);
#3720=CIRCLE('',#10861,0.00525000000001);
#3721=CIRCLE('',#10863,0.00410000000001);
#3722=CIRCLE('',#10864,0.00410000000001);
#3723=CIRCLE('',#10867,0.00250000000001);
#3724=CIRCLE('',#10872,0.00300000000001);
#3725=CIRCLE('',#10873,0.00155000000001);
#3726=CIRCLE('',#10881,0.00155000000001);
#3727=CIRCLE('',#10882,0.00155000000001);
#3728=CIRCLE('',#10886,0.00300000000001);
#3729=CIRCLE('',#10887,0.00300000000001);
#3730=CIRCLE('',#10893,0.00150000000001);
#3731=CIRCLE('',#10894,0.00110000000001);
#3732=CIRCLE('',#10896,0.00150000000001);
#3733=CIRCLE('',#10901,0.00150000000001);
#3734=CIRCLE('',#10917,0.00117524047359083);
#3735=CIRCLE('',#10934,0.00117524047359083);
#3736=CIRCLE('',#10936,0.00150000000001);
#3737=CIRCLE('',#10938,0.00115470053838925);
#3738=CIRCLE('',#10940,0.00285000000001);
#3739=CIRCLE('',#10941,0.00285000000001);
#3740=CIRCLE('',#10943,0.00150000000001);
#3741=CIRCLE('',#10945,0.00112500000001);
#3742=CIRCLE('',#10948,0.00115470053838925);
#3743=CIRCLE('',#10949,0.00115470053838925);
#3744=CIRCLE('',#10950,0.00115470053838925);
#3745=CIRCLE('',#10951,0.00115470053838925);
#3746=CIRCLE('',#10952,0.00115470053838925);
#3747=CIRCLE('',#10968,0.00075000000001);
#3748=CIRCLE('',#10970,0.00075000000001);
#3749=CIRCLE('',#10971,0.00075000000001);
#3750=CIRCLE('',#10972,0.00075000000001);
#3751=CIRCLE('',#10974,0.00225);
#3752=CIRCLE('',#10975,0.00075000000001);
#3753=CIRCLE('',#10976,0.00075000000001);
#3754=CIRCLE('',#10981,0.00025000000001);
#3755=CIRCLE('',#10982,0.00025000000001);
#3756=CIRCLE('',#10983,0.00025000000001);
#3757=CIRCLE('',#10985,0.00275);
#3758=CIRCLE('',#10986,0.00025000000001);
#3759=CIRCLE('',#10987,0.00025000000001);
#3760=CIRCLE('',#10989,0.00025000000001);
#3761=CIRCLE('',#10994,0.00444200000001);
#3762=CIRCLE('',#10996,0.00387200000001);
#3763=CIRCLE('',#10998,0.00387200000001);
#3764=CIRCLE('',#11000,0.00444200000001);
#3765=CIRCLE('',#11002,0.00250000000001);
#3766=CIRCLE('',#11003,0.00290000000001);
#3767=CIRCLE('',#11005,0.00250000000001);
#3768=CIRCLE('',#11008,0.00290000000001);
#3769=CIRCLE('',#11010,0.00380000000001);
#3770=CIRCLE('',#11012,0.00444200000001);
#3771=CIRCLE('',#11013,0.00444200000001);
#3772=VERTEX_POINT('',#13474);
#3773=VERTEX_POINT('',#13476);
#3774=VERTEX_POINT('',#13483);
#3775=VERTEX_POINT('',#13486);
#3776=VERTEX_POINT('',#13488);
#3777=VERTEX_POINT('',#13490);
#3778=VERTEX_POINT('',#13494);
#3779=VERTEX_POINT('',#13496);
#3780=VERTEX_POINT('',#13504);
#3781=VERTEX_POINT('',#13507);
#3782=VERTEX_POINT('',#13509);
#3783=VERTEX_POINT('',#13511);
#3784=VERTEX_POINT('',#13515);
#3785=VERTEX_POINT('',#13517);
#3786=VERTEX_POINT('',#13525);
#3787=VERTEX_POINT('',#13527);
#3788=VERTEX_POINT('',#13531);
#3789=VERTEX_POINT('',#13534);
#3790=VERTEX_POINT('',#13535);
#3791=VERTEX_POINT('',#13537);
#3792=VERTEX_POINT('',#13539);
#3793=VERTEX_POINT('',#13541);
#3794=VERTEX_POINT('',#13543);
#3795=VERTEX_POINT('',#13545);
#3796=VERTEX_POINT('',#13547);
#3797=VERTEX_POINT('',#13549);
#3798=VERTEX_POINT('',#13551);
#3799=VERTEX_POINT('',#13553);
#3800=VERTEX_POINT('',#13555);
#3801=VERTEX_POINT('',#13557);
#3802=VERTEX_POINT('',#13559);
#3803=VERTEX_POINT('',#13561);
#3804=VERTEX_POINT('',#13563);
#3805=VERTEX_POINT('',#13565);
#3806=VERTEX_POINT('',#13570);
#3807=VERTEX_POINT('',#13572);
#3808=VERTEX_POINT('',#13576);
#3809=VERTEX_POINT('',#13578);
#3810=VERTEX_POINT('',#13580);
#3811=VERTEX_POINT('',#13582);
#3812=VERTEX_POINT('',#13584);
#3813=VERTEX_POINT('',#13586);
#3814=VERTEX_POINT('',#13588);
#3815=VERTEX_POINT('',#13590);
#3816=VERTEX_POINT('',#13592);
#3817=VERTEX_POINT('',#13594);
#3818=VERTEX_POINT('',#13596);
#3819=VERTEX_POINT('',#13598);
#3820=VERTEX_POINT('',#13600);
#3821=VERTEX_POINT('',#13602);
#3822=VERTEX_POINT('',#13604);
#3823=VERTEX_POINT('',#13606);
#3824=VERTEX_POINT('',#13608);
#3825=VERTEX_POINT('',#13610);
#3826=VERTEX_POINT('',#13612);
#3827=VERTEX_POINT('',#13614);
#3828=VERTEX_POINT('',#13616);
#3829=VERTEX_POINT('',#13618);
#3830=VERTEX_POINT('',#13620);
#3831=VERTEX_POINT('',#13622);
#3832=VERTEX_POINT('',#13624);
#3833=VERTEX_POINT('',#13626);
#3834=VERTEX_POINT('',#13628);
#3835=VERTEX_POINT('',#13630);
#3836=VERTEX_POINT('',#13632);
#3837=VERTEX_POINT('',#13634);
#3838=VERTEX_POINT('',#13636);
#3839=VERTEX_POINT('',#13638);
#3840=VERTEX_POINT('',#13640);
#3841=VERTEX_POINT('',#13642);
#3842=VERTEX_POINT('',#13644);
#3843=VERTEX_POINT('',#13646);
#3844=VERTEX_POINT('',#13648);
#3845=VERTEX_POINT('',#13650);
#3846=VERTEX_POINT('',#13652);
#3847=VERTEX_POINT('',#13654);
#3848=VERTEX_POINT('',#13656);
#3849=VERTEX_POINT('',#13660);
#3850=VERTEX_POINT('',#13663);
#3851=VERTEX_POINT('',#13665);
#3852=VERTEX_POINT('',#13671);
#3853=VERTEX_POINT('',#13673);
#3854=VERTEX_POINT('',#13683);
#3855=VERTEX_POINT('',#13685);
#3856=VERTEX_POINT('',#13691);
#3857=VERTEX_POINT('',#13695);
#3858=VERTEX_POINT('',#13696);
#3859=VERTEX_POINT('',#13703);
#3860=VERTEX_POINT('',#13707);
#3861=VERTEX_POINT('',#13713);
#3862=VERTEX_POINT('',#13714);
#3863=VERTEX_POINT('',#13721);
#3864=VERTEX_POINT('',#13725);
#3865=VERTEX_POINT('',#13731);
#3866=VERTEX_POINT('',#13741);
#3867=VERTEX_POINT('',#13745);
#3868=VERTEX_POINT('',#13747);
#3869=VERTEX_POINT('',#13752);
#3870=VERTEX_POINT('',#13756);
#3871=VERTEX_POINT('',#13760);
#3872=VERTEX_POINT('',#13761);
#3873=VERTEX_POINT('',#13769);
#3874=VERTEX_POINT('',#13771);
#3875=VERTEX_POINT('',#13784);
#3876=VERTEX_POINT('',#13785);
#3877=VERTEX_POINT('',#13791);
#3878=VERTEX_POINT('',#13793);
#3879=VERTEX_POINT('',#13804);
#3880=VERTEX_POINT('',#13805);
#3881=VERTEX_POINT('',#13813);
#3882=VERTEX_POINT('',#13866);
#3883=VERTEX_POINT('',#13867);
#3884=VERTEX_POINT('',#13935);
#3885=VERTEX_POINT('',#13985);
#3886=VERTEX_POINT('',#14035);
#3887=VERTEX_POINT('',#14085);
#3888=VERTEX_POINT('',#14135);
#3889=VERTEX_POINT('',#14185);
#3890=VERTEX_POINT('',#14235);
#3891=VERTEX_POINT('',#14285);
#3892=VERTEX_POINT('',#14335);
#3893=VERTEX_POINT('',#14385);
#3894=VERTEX_POINT('',#14393);
#3895=VERTEX_POINT('',#14395);
#3896=VERTEX_POINT('',#14433);
#3897=VERTEX_POINT('',#14483);
#3898=VERTEX_POINT('',#14533);
#3899=VERTEX_POINT('',#14583);
#3900=VERTEX_POINT('',#14633);
#3901=VERTEX_POINT('',#14710);
#3902=VERTEX_POINT('',#14760);
#3903=VERTEX_POINT('',#14810);
#3904=VERTEX_POINT('',#14860);
#3905=VERTEX_POINT('',#14910);
#3906=VERTEX_POINT('',#14960);
#3907=VERTEX_POINT('',#15010);
#3908=VERTEX_POINT('',#15084);
#3909=VERTEX_POINT('',#15134);
#3910=VERTEX_POINT('',#15154);
#3911=VERTEX_POINT('',#15156);
#3912=VERTEX_POINT('',#15191);
#3913=VERTEX_POINT('',#15241);
#3914=VERTEX_POINT('',#15341);
#3915=VERTEX_POINT('',#15342);
#3916=VERTEX_POINT('',#15419);
#3917=VERTEX_POINT('',#15469);
#3918=VERTEX_POINT('',#15519);
#3919=VERTEX_POINT('',#15554);
#3920=VERTEX_POINT('',#15604);
#3921=VERTEX_POINT('',#15654);
#3922=VERTEX_POINT('',#15704);
#3923=VERTEX_POINT('',#15781);
#3924=VERTEX_POINT('',#15831);
#3925=VERTEX_POINT('',#15833);
#3926=VERTEX_POINT('',#15841);
#3927=VERTEX_POINT('',#15891);
#3928=VERTEX_POINT('',#15941);
#3929=VERTEX_POINT('',#15994);
#3930=VERTEX_POINT('',#16044);
#3931=VERTEX_POINT('',#16094);
#3932=VERTEX_POINT('',#16144);
#3933=VERTEX_POINT('',#16194);
#3934=VERTEX_POINT('',#16244);
#3935=VERTEX_POINT('',#16294);
#3936=VERTEX_POINT('',#16341);
#3937=VERTEX_POINT('',#16391);
#3938=VERTEX_POINT('',#16441);
#3939=VERTEX_POINT('',#16491);
#3940=VERTEX_POINT('',#16541);
#3941=VERTEX_POINT('',#16543);
#3942=VERTEX_POINT('',#16593);
#3943=VERTEX_POINT('',#16628);
#3944=VERTEX_POINT('',#16678);
#3945=VERTEX_POINT('',#16777);
#3946=VERTEX_POINT('',#16780);
#3947=VERTEX_POINT('',#16782);
#3948=VERTEX_POINT('',#16786);
#3949=VERTEX_POINT('',#16789);
#3950=VERTEX_POINT('',#16791);
#3951=VERTEX_POINT('',#16795);
#3952=VERTEX_POINT('',#16797);
#3953=VERTEX_POINT('',#16801);
#3954=VERTEX_POINT('',#16805);
#3955=VERTEX_POINT('',#16810);
#3956=VERTEX_POINT('',#16811);
#3957=VERTEX_POINT('',#16816);
#3958=VERTEX_POINT('',#16818);
#3959=VERTEX_POINT('',#17810);
#3960=VERTEX_POINT('',#17812);
#3961=VERTEX_POINT('',#17815);
#3962=VERTEX_POINT('',#17817);
#3963=VERTEX_POINT('',#17820);
#3964=VERTEX_POINT('',#17822);
#3965=VERTEX_POINT('',#17825);
#3966=VERTEX_POINT('',#17827);
#3967=VERTEX_POINT('',#17830);
#3968=VERTEX_POINT('',#17832);
#3969=VERTEX_POINT('',#17835);
#3970=VERTEX_POINT('',#17837);
#3971=VERTEX_POINT('',#17840);
#3972=VERTEX_POINT('',#17842);
#3973=VERTEX_POINT('',#17845);
#3974=VERTEX_POINT('',#17847);
#3975=VERTEX_POINT('',#17850);
#3976=VERTEX_POINT('',#17852);
#3977=VERTEX_POINT('',#17855);
#3978=VERTEX_POINT('',#17857);
#3979=VERTEX_POINT('',#17860);
#3980=VERTEX_POINT('',#17862);
#3981=VERTEX_POINT('',#17865);
#3982=VERTEX_POINT('',#17867);
#3983=VERTEX_POINT('',#17870);
#3984=VERTEX_POINT('',#17872);
#3985=VERTEX_POINT('',#17875);
#3986=VERTEX_POINT('',#17877);
#3987=VERTEX_POINT('',#17880);
#3988=VERTEX_POINT('',#17882);
#3989=VERTEX_POINT('',#17885);
#3990=VERTEX_POINT('',#17903);
#3991=VERTEX_POINT('',#17920);
#3992=VERTEX_POINT('',#17922);
#3993=VERTEX_POINT('',#17926);
#3994=VERTEX_POINT('',#17928);
#3995=VERTEX_POINT('',#17932);
#3996=VERTEX_POINT('',#17934);
#3997=VERTEX_POINT('',#17938);
#3998=VERTEX_POINT('',#17940);
#3999=VERTEX_POINT('',#17946);
#4000=VERTEX_POINT('',#17949);
#4001=VERTEX_POINT('',#17954);
#4002=VERTEX_POINT('',#17957);
#4003=VERTEX_POINT('',#17962);
#4004=VERTEX_POINT('',#17965);
#4005=VERTEX_POINT('',#17970);
#4006=VERTEX_POINT('',#17973);
#4007=VERTEX_POINT('',#17978);
#4008=VERTEX_POINT('',#17980);
#4009=VERTEX_POINT('',#17983);
#4010=VERTEX_POINT('',#17991);
#4011=VERTEX_POINT('',#17992);
#4012=VERTEX_POINT('',#17994);
#4013=VERTEX_POINT('',#17996);
#4014=VERTEX_POINT('',#18000);
#4015=VERTEX_POINT('',#18004);
#4016=VERTEX_POINT('',#18005);
#4017=VERTEX_POINT('',#18007);
#4018=VERTEX_POINT('',#18009);
#4019=VERTEX_POINT('',#18013);
#4020=VERTEX_POINT('',#18017);
#4021=VERTEX_POINT('',#18019);
#4022=VERTEX_POINT('',#18021);
#4023=VERTEX_POINT('',#18025);
#4024=VERTEX_POINT('',#18027);
#4025=VERTEX_POINT('',#18031);
#4026=VERTEX_POINT('',#18033);
#4027=VERTEX_POINT('',#18035);
#4028=VERTEX_POINT('',#18039);
#4029=VERTEX_POINT('',#18040);
#4030=VERTEX_POINT('',#18042);
#4031=VERTEX_POINT('',#18044);
#4032=VERTEX_POINT('',#18048);
#4033=VERTEX_POINT('',#18049);
#4034=VERTEX_POINT('',#18051);
#4035=VERTEX_POINT('',#18053);
#4036=VERTEX_POINT('',#18063);
#4037=VERTEX_POINT('',#18065);
#4038=VERTEX_POINT('',#18078);
#4039=VERTEX_POINT('',#18081);
#4040=VERTEX_POINT('',#18083);
#4041=VERTEX_POINT('',#18085);
#4042=VERTEX_POINT('',#18089);
#4043=VERTEX_POINT('',#18091);
#4044=VERTEX_POINT('',#18099);
#4045=VERTEX_POINT('',#18101);
#4046=VERTEX_POINT('',#18103);
#4047=VERTEX_POINT('',#18107);
#4048=VERTEX_POINT('',#18109);
#4049=VERTEX_POINT('',#18113);
#4050=VERTEX_POINT('',#18120);
#4051=VERTEX_POINT('',#18122);
#4052=VERTEX_POINT('',#18124);
#4053=VERTEX_POINT('',#18128);
#4054=VERTEX_POINT('',#18130);
#4055=VERTEX_POINT('',#18134);
#4056=VERTEX_POINT('',#18141);
#4057=VERTEX_POINT('',#18142);
#4058=VERTEX_POINT('',#18144);
#4059=VERTEX_POINT('',#18149);
#4060=VERTEX_POINT('',#18160);
#4061=VERTEX_POINT('',#18167);
#4062=VERTEX_POINT('',#18221);
#4063=VERTEX_POINT('',#18222);
#4064=VERTEX_POINT('',#18224);
#4065=VERTEX_POINT('',#18590);
#4066=VERTEX_POINT('',#18591);
#4067=VERTEX_POINT('',#18769);
#4068=VERTEX_POINT('',#18955);
#4069=VERTEX_POINT('',#18956);
#4070=VERTEX_POINT('',#19315);
#4071=VERTEX_POINT('',#19316);
#4072=VERTEX_POINT('',#19675);
#4073=VERTEX_POINT('',#19676);
#4074=VERTEX_POINT('',#20037);
#4075=VERTEX_POINT('',#20038);
#4076=VERTEX_POINT('',#20040);
#4077=VERTEX_POINT('',#20410);
#4078=VERTEX_POINT('',#20411);
#4079=VERTEX_POINT('',#20413);
#4080=VERTEX_POINT('',#20433);
#4081=VERTEX_POINT('',#20534);
#4082=VERTEX_POINT('',#20535);
#4083=VERTEX_POINT('',#20537);
#4084=VERTEX_POINT('',#20542);
#4085=VERTEX_POINT('',#20553);
#4086=VERTEX_POINT('',#20644);
#4087=VERTEX_POINT('',#20645);
#4088=VERTEX_POINT('',#20647);
#4089=VERTEX_POINT('',#20844);
#4090=VERTEX_POINT('',#21042);
#4091=VERTEX_POINT('',#21043);
#4092=VERTEX_POINT('',#21464);
#4093=VERTEX_POINT('',#21465);
#4094=VERTEX_POINT('',#21856);
#4095=VERTEX_POINT('',#21857);
#4096=VERTEX_POINT('',#22278);
#4097=VERTEX_POINT('',#22279);
#4098=VERTEX_POINT('',#22281);
#4099=VERTEX_POINT('',#22492);
#4100=VERTEX_POINT('',#22702);
#4101=VERTEX_POINT('',#22703);
#4102=VERTEX_POINT('',#23108);
#4103=VERTEX_POINT('',#23109);
#4104=VERTEX_POINT('',#23526);
#4105=VERTEX_POINT('',#23527);
#4106=VERTEX_POINT('',#23928);
#4107=VERTEX_POINT('',#23929);
#4108=VERTEX_POINT('',#24344);
#4109=VERTEX_POINT('',#24345);
#4110=VERTEX_POINT('',#24545);
#4111=VERTEX_POINT('',#24743);
#4112=VERTEX_POINT('',#24744);
#4113=VERTEX_POINT('',#24746);
#4114=VERTEX_POINT('',#25166);
#4115=VERTEX_POINT('',#25167);
#4116=VERTEX_POINT('',#25169);
#4117=VERTEX_POINT('',#25189);
#4118=VERTEX_POINT('',#25302);
#4119=VERTEX_POINT('',#25303);
#4120=VERTEX_POINT('',#25305);
#4121=VERTEX_POINT('',#25331);
#4122=VERTEX_POINT('',#25355);
#4123=VERTEX_POINT('',#25356);
#4124=VERTEX_POINT('',#25442);
#4125=VERTEX_POINT('',#25443);
#4126=VERTEX_POINT('',#25657);
#4127=VERTEX_POINT('',#25658);
#4128=VERTEX_POINT('',#25864);
#4129=VERTEX_POINT('',#25865);
#4130=VERTEX_POINT('',#26071);
#4131=VERTEX_POINT('',#26072);
#4132=VERTEX_POINT('',#26296);
#4133=VERTEX_POINT('',#26297);
#4134=VERTEX_POINT('',#26299);
#4135=VERTEX_POINT('',#26325);
#4136=VERTEX_POINT('',#26377);
#4137=VERTEX_POINT('',#26378);
#4138=VERTEX_POINT('',#26380);
#4139=VERTEX_POINT('',#26406);
#4140=VERTEX_POINT('',#26434);
#4141=VERTEX_POINT('',#26435);
#4142=VERTEX_POINT('',#26536);
#4143=VERTEX_POINT('',#26537);
#4144=VERTEX_POINT('',#26638);
#4145=VERTEX_POINT('',#26639);
#4146=VERTEX_POINT('',#26740);
#4147=VERTEX_POINT('',#26741);
#4148=VERTEX_POINT('',#26848);
#4149=VERTEX_POINT('',#26849);
#4150=VERTEX_POINT('',#26950);
#4151=VERTEX_POINT('',#26951);
#4152=VERTEX_POINT('',#27052);
#4153=VERTEX_POINT('',#27053);
#4154=VERTEX_POINT('',#27166);
#4155=VERTEX_POINT('',#27167);
#4156=VERTEX_POINT('',#27265);
#4157=VERTEX_POINT('',#27266);
#4158=VERTEX_POINT('',#27367);
#4159=VERTEX_POINT('',#27368);
#4160=VERTEX_POINT('',#27469);
#4161=VERTEX_POINT('',#27470);
#4162=VERTEX_POINT('',#27472);
#4163=VERTEX_POINT('',#27498);
#4164=VERTEX_POINT('',#27856);
#4165=VERTEX_POINT('',#27857);
#4166=VERTEX_POINT('',#27859);
#4167=VERTEX_POINT('',#27861);
#4168=VERTEX_POINT('',#27865);
#4169=VERTEX_POINT('',#27867);
#4170=VERTEX_POINT('',#27871);
#4171=VERTEX_POINT('',#27873);
#4172=VERTEX_POINT('',#27877);
#4173=VERTEX_POINT('',#27878);
#4174=VERTEX_POINT('',#27883);
#4175=VERTEX_POINT('',#27885);
#4176=VERTEX_POINT('',#27887);
#4177=VERTEX_POINT('',#27892);
#4178=VERTEX_POINT('',#27895);
#4179=VERTEX_POINT('',#27899);
#4180=VERTEX_POINT('',#27900);
#4181=VERTEX_POINT('',#27903);
#4182=VERTEX_POINT('',#27905);
#4183=VERTEX_POINT('',#27907);
#4184=VERTEX_POINT('',#27910);
#4185=VERTEX_POINT('',#27912);
#4186=VERTEX_POINT('',#27919);
#4187=VERTEX_POINT('',#27920);
#4188=VERTEX_POINT('',#27922);
#4189=VERTEX_POINT('',#27925);
#4190=VERTEX_POINT('',#27927);
#4191=VERTEX_POINT('',#27929);
#4192=VERTEX_POINT('',#27931);
#4193=VERTEX_POINT('',#27933);
#4194=VERTEX_POINT('',#27937);
#4195=VERTEX_POINT('',#27941);
#4196=VERTEX_POINT('',#27943);
#4197=VERTEX_POINT('',#27947);
#4198=VERTEX_POINT('',#27953);
#4199=VERTEX_POINT('',#27954);
#4200=VERTEX_POINT('',#27956);
#4201=VERTEX_POINT('',#27958);
#4202=VERTEX_POINT('',#27960);
#4203=VERTEX_POINT('',#27963);
#4204=VERTEX_POINT('',#27965);
#4205=VERTEX_POINT('',#27975);
#4206=VERTEX_POINT('',#27976);
#4207=VERTEX_POINT('',#27987);
#4208=VERTEX_POINT('',#27989);
#4209=VERTEX_POINT('',#28001);
#4210=VERTEX_POINT('',#28006);
#4211=VERTEX_POINT('',#28008);
#4212=VERTEX_POINT('',#28012);
#4213=VERTEX_POINT('',#28014);
#4214=VERTEX_POINT('',#28018);
#4215=VERTEX_POINT('',#28075);
#4216=VERTEX_POINT('',#28084);
#4217=VERTEX_POINT('',#28088);
#4218=VERTEX_POINT('',#28092);
#4219=VERTEX_POINT('',#28094);
#4220=VERTEX_POINT('',#28098);
#4221=VERTEX_POINT('',#28102);
#4222=VERTEX_POINT('',#28103);
#4223=VERTEX_POINT('',#28153);
#4224=VERTEX_POINT('',#28203);
#4225=VERTEX_POINT('',#28253);
#4226=VERTEX_POINT('',#28378);
#4227=VERTEX_POINT('',#28428);
#4228=VERTEX_POINT('',#28478);
#4229=VERTEX_POINT('',#28513);
#4230=VERTEX_POINT('',#28563);
#4231=VERTEX_POINT('',#28613);
#4232=VERTEX_POINT('',#28651);
#4233=VERTEX_POINT('',#28653);
#4234=VERTEX_POINT('',#28667);
#4235=VERTEX_POINT('',#28717);
#4236=VERTEX_POINT('',#28767);
#4237=VERTEX_POINT('',#28817);
#4238=VERTEX_POINT('',#28867);
#4239=VERTEX_POINT('',#28917);
#4240=VERTEX_POINT('',#28967);
#4241=VERTEX_POINT('',#29068);
#4242=VERTEX_POINT('',#29118);
#4243=VERTEX_POINT('',#29267);
#4244=VERTEX_POINT('',#29268);
#4245=VERTEX_POINT('',#29362);
#4246=VERTEX_POINT('',#29364);
#4247=VERTEX_POINT('',#29371);
#4248=VERTEX_POINT('',#30513);
#4249=VERTEX_POINT('',#30514);
#4250=VERTEX_POINT('',#30522);
#4251=VERTEX_POINT('',#30527);
#4252=VERTEX_POINT('',#30534);
#4253=VERTEX_POINT('',#30565);
#4254=VERTEX_POINT('',#30572);
#4255=VERTEX_POINT('',#30579);
#4256=VERTEX_POINT('',#30587);
#4257=VERTEX_POINT('',#30589);
#4258=VERTEX_POINT('',#30596);
#4259=VERTEX_POINT('',#30598);
#4260=VERTEX_POINT('',#30607);
#4261=VERTEX_POINT('',#30609);
#4262=VERTEX_POINT('',#30617);
#4263=VERTEX_POINT('',#30650);
#4264=VERTEX_POINT('',#30658);
#4265=VERTEX_POINT('',#30660);
#4266=VERTEX_POINT('',#30668);
#4267=VERTEX_POINT('',#30673);
#4268=VERTEX_POINT('',#30681);
#4269=VERTEX_POINT('',#30964);
#4270=VERTEX_POINT('',#31014);
#4271=VERTEX_POINT('',#31028);
#4272=VERTEX_POINT('',#31078);
#4273=VERTEX_POINT('',#31128);
#4274=VERTEX_POINT('',#31178);
#4275=VERTEX_POINT('',#31228);
#4276=VERTEX_POINT('',#31278);
#4277=VERTEX_POINT('',#31328);
#4278=VERTEX_POINT('',#31378);
#4279=VERTEX_POINT('',#31458);
#4280=VERTEX_POINT('',#31833);
#4281=VERTEX_POINT('',#31883);
#4282=VERTEX_POINT('',#31909);
#4283=VERTEX_POINT('',#32112);
#4284=VERTEX_POINT('',#33069);
#4285=VERTEX_POINT('',#33777);
#4286=VERTEX_POINT('',#34388);
#4287=VERTEX_POINT('',#34591);
#4288=VERTEX_POINT('',#34598);
#4289=VERTEX_POINT('',#34767);
#4290=VERTEX_POINT('',#34769);
#4291=VERTEX_POINT('',#34771);
#4292=VERTEX_POINT('',#34775);
#4293=VERTEX_POINT('',#34777);
#4294=VERTEX_POINT('',#34781);
#4295=VERTEX_POINT('',#34788);
#4296=VERTEX_POINT('',#34789);
#4297=VERTEX_POINT('',#34839);
#4298=VERTEX_POINT('',#34895);
#4299=VERTEX_POINT('',#34945);
#4300=VERTEX_POINT('',#34995);
#4301=VERTEX_POINT('',#35072);
#4302=VERTEX_POINT('',#35122);
#4303=VERTEX_POINT('',#35172);
#4304=VERTEX_POINT('',#35222);
#4305=VERTEX_POINT('',#35272);
#4306=VERTEX_POINT('',#35274);
#4307=VERTEX_POINT('',#35276);
#4308=VERTEX_POINT('',#35302);
#4309=VERTEX_POINT('',#35352);
#4310=VERTEX_POINT('',#35402);
#4311=VERTEX_POINT('',#35455);
#4312=VERTEX_POINT('',#35505);
#4313=VERTEX_POINT('',#35555);
#4314=VERTEX_POINT('',#35644);
#4315=VERTEX_POINT('',#35694);
#4316=VERTEX_POINT('',#35744);
#4317=VERTEX_POINT('',#35779);
#4318=VERTEX_POINT('',#35784);
#4319=VERTEX_POINT('',#35836);
#4320=VERTEX_POINT('',#35837);
#4321=VERTEX_POINT('',#35887);
#4322=VERTEX_POINT('',#36834);
#4323=VERTEX_POINT('',#37225);
#4324=VERTEX_POINT('',#37328);
#4325=VERTEX_POINT('',#37330);
#4326=VERTEX_POINT('',#37338);
#4327=VERTEX_POINT('',#37430);
#4328=VERTEX_POINT('',#37480);
#4329=VERTEX_POINT('',#37530);
#4330=VERTEX_POINT('',#37580);
#4331=VERTEX_POINT('',#37630);
#4332=VERTEX_POINT('',#37680);
#4333=VERTEX_POINT('',#37730);
#4334=VERTEX_POINT('',#37780);
#4335=VERTEX_POINT('',#37830);
#4336=VERTEX_POINT('',#37853);
#4337=VERTEX_POINT('',#37855);
#4338=VERTEX_POINT('',#38202);
#4339=VERTEX_POINT('',#38210);
#4340=VERTEX_POINT('',#38211);
#4341=VERTEX_POINT('',#38261);
#4342=VERTEX_POINT('',#38371);
#4343=VERTEX_POINT('',#38421);
#4344=VERTEX_POINT('',#38456);
#4345=VERTEX_POINT('',#38458);
#4346=VERTEX_POINT('',#38460);
#4347=VERTEX_POINT('',#38486);
#4348=VERTEX_POINT('',#38536);
#4349=VERTEX_POINT('',#38586);
#4350=VERTEX_POINT('',#38636);
#4351=VERTEX_POINT('',#38686);
#4352=VERTEX_POINT('',#38691);
#4353=VERTEX_POINT('',#38743);
#4354=VERTEX_POINT('',#38744);
#4355=VERTEX_POINT('',#38794);
#4356=VERTEX_POINT('',#38844);
#4357=VERTEX_POINT('',#38870);
#4358=VERTEX_POINT('',#38872);
#4359=VERTEX_POINT('',#38883);
#4360=VERTEX_POINT('',#38933);
#4361=VERTEX_POINT('',#38983);
#4362=VERTEX_POINT('',#39033);
#4363=VERTEX_POINT('',#39083);
#4364=VERTEX_POINT('',#39109);
#4365=VERTEX_POINT('',#39111);
#4366=VERTEX_POINT('',#39119);
#4367=VERTEX_POINT('',#39237);
#4368=VERTEX_POINT('',#39239);
#4369=VERTEX_POINT('',#39243);
#4370=VERTEX_POINT('',#39247);
#4371=VERTEX_POINT('',#39250);
#4372=VERTEX_POINT('',#39252);
#4373=VERTEX_POINT('',#39256);
#4374=VERTEX_POINT('',#39259);
#4375=VERTEX_POINT('',#39265);
#4376=VERTEX_POINT('',#39269);
#4377=VERTEX_POINT('',#39273);
#4378=VERTEX_POINT('',#39274);
#4379=VERTEX_POINT('',#40001);
#4380=VERTEX_POINT('',#40235);
#4381=VERTEX_POINT('',#40465);
#4382=VERTEX_POINT('',#40470);
#4383=VERTEX_POINT('',#40476);
#4384=VERTEX_POINT('',#40478);
#4385=VERTEX_POINT('',#40482);
#4386=VERTEX_POINT('',#40487);
#4387=VERTEX_POINT('',#40493);
#4388=VERTEX_POINT('',#40494);
#4389=VERTEX_POINT('',#40496);
#4390=VERTEX_POINT('',#40547);
#4391=VERTEX_POINT('',#40580);
#4392=VERTEX_POINT('',#40581);
#4393=VERTEX_POINT('',#40583);
#4394=VERTEX_POINT('',#40903);
#4395=VERTEX_POINT('',#40904);
#4396=VERTEX_POINT('',#41221);
#4397=VERTEX_POINT('',#41222);
#4398=VERTEX_POINT('',#41541);
#4399=VERTEX_POINT('',#41542);
#4400=VERTEX_POINT('',#41859);
#4401=VERTEX_POINT('',#41890);
#4402=VERTEX_POINT('',#41892);
#4403=VERTEX_POINT('',#41894);
#4404=VERTEX_POINT('',#41920);
#4405=VERTEX_POINT('',#41922);
#4406=VERTEX_POINT('',#42094);
#4407=VERTEX_POINT('',#42095);
#4408=VERTEX_POINT('',#42103);
#4409=VERTEX_POINT('',#42105);
#4410=VERTEX_POINT('',#42455);
#4411=VERTEX_POINT('',#42456);
#4412=VERTEX_POINT('',#43013);
#4413=VERTEX_POINT('',#43027);
#4414=VERTEX_POINT('',#43029);
#4415=VERTEX_POINT('',#43094);
#4416=VERTEX_POINT('',#43144);
#4417=VERTEX_POINT('',#43194);
#4418=VERTEX_POINT('',#43244);
#4419=VERTEX_POINT('',#43294);
#4420=VERTEX_POINT('',#43344);
#4421=VERTEX_POINT('',#43346);
#4422=VERTEX_POINT('',#43611);
#4423=VERTEX_POINT('',#43612);
#4424=VERTEX_POINT('',#43614);
#4425=VERTEX_POINT('',#43616);
#4426=VERTEX_POINT('',#43618);
#4427=VERTEX_POINT('',#43620);
#4428=VERTEX_POINT('',#43622);
#4429=VERTEX_POINT('',#43624);
#4430=VERTEX_POINT('',#43626);
#4431=VERTEX_POINT('',#43628);
#4432=VERTEX_POINT('',#43630);
#4433=VERTEX_POINT('',#43632);
#4434=VERTEX_POINT('',#43636);
#4435=VERTEX_POINT('',#43640);
#4436=VERTEX_POINT('',#43642);
#4437=VERTEX_POINT('',#43646);
#4438=VERTEX_POINT('',#43648);
#4439=VERTEX_POINT('',#43650);
#4440=VERTEX_POINT('',#43652);
#4441=VERTEX_POINT('',#43654);
#4442=VERTEX_POINT('',#43657);
#4443=VERTEX_POINT('',#43660);
#4444=VERTEX_POINT('',#43662);
#4445=VERTEX_POINT('',#43666);
#4446=VERTEX_POINT('',#43668);
#4447=VERTEX_POINT('',#43670);
#4448=VERTEX_POINT('',#43672);
#4449=VERTEX_POINT('',#43674);
#4450=VERTEX_POINT('',#43677);
#4451=VERTEX_POINT('',#43680);
#4452=VERTEX_POINT('',#43684);
#4453=VERTEX_POINT('',#43686);
#4454=VERTEX_POINT('',#43690);
#4455=VERTEX_POINT('',#43692);
#4456=VERTEX_POINT('',#43694);
#4457=VERTEX_POINT('',#43696);
#4458=VERTEX_POINT('',#43698);
#4459=VERTEX_POINT('',#43702);
#4460=VERTEX_POINT('',#43706);
#4461=VERTEX_POINT('',#43710);
#4462=VERTEX_POINT('',#43712);
#4463=VERTEX_POINT('',#43716);
#4464=VERTEX_POINT('',#43719);
#4465=VERTEX_POINT('',#43721);
#4466=VERTEX_POINT('',#43724);
#4467=VERTEX_POINT('',#43726);
#4468=VERTEX_POINT('',#43729);
#4469=VERTEX_POINT('',#43732);
#4470=VERTEX_POINT('',#43736);
#4471=VERTEX_POINT('',#43740);
#4472=VERTEX_POINT('',#43744);
#4473=VERTEX_POINT('',#43748);
#4474=VERTEX_POINT('',#43752);
#4475=VERTEX_POINT('',#43846);
#4476=VERTEX_POINT('',#43849);
#4477=VERTEX_POINT('',#43852);
#4478=VERTEX_POINT('',#43855);
#4479=VERTEX_POINT('',#43857);
#4480=VERTEX_POINT('',#43859);
#4481=VERTEX_POINT('',#43863);
#4482=VERTEX_POINT('',#43867);
#4483=VERTEX_POINT('',#43869);
#4484=VERTEX_POINT('',#43873);
#4485=VERTEX_POINT('',#43878);
#4486=VERTEX_POINT('',#43879);
#4487=VERTEX_POINT('',#44464);
#4488=VERTEX_POINT('',#44465);
#4489=VERTEX_POINT('',#44472);
#4490=VERTEX_POINT('',#44479);
#4491=VERTEX_POINT('',#44518);
#4492=VERTEX_POINT('',#44525);
#4493=VERTEX_POINT('',#44564);
#4494=VERTEX_POINT('',#44571);
#4495=VERTEX_POINT('',#44610);
#4496=VERTEX_POINT('',#44617);
#4497=VERTEX_POINT('',#44656);
#4498=VERTEX_POINT('',#44663);
#4499=VERTEX_POINT('',#44702);
#4500=VERTEX_POINT('',#44703);
#4501=VERTEX_POINT('',#44710);
#4502=VERTEX_POINT('',#44717);
#4503=VERTEX_POINT('',#44756);
#4504=VERTEX_POINT('',#44763);
#4505=VERTEX_POINT('',#44802);
#4506=VERTEX_POINT('',#44809);
#4507=VERTEX_POINT('',#44848);
#4508=VERTEX_POINT('',#44855);
#4509=VERTEX_POINT('',#44894);
#4510=VERTEX_POINT('',#44901);
#4511=VERTEX_POINT('',#44940);
#4512=VERTEX_POINT('',#44941);
#4513=VERTEX_POINT('',#44948);
#4514=VERTEX_POINT('',#44955);
#4515=VERTEX_POINT('',#44994);
#4516=VERTEX_POINT('',#45001);
#4517=VERTEX_POINT('',#45040);
#4518=VERTEX_POINT('',#45047);
#4519=VERTEX_POINT('',#45086);
#4520=VERTEX_POINT('',#45093);
#4521=VERTEX_POINT('',#45132);
#4522=VERTEX_POINT('',#45139);
#4523=VERTEX_POINT('',#45178);
#4524=VERTEX_POINT('',#45179);
#4525=VERTEX_POINT('',#45186);
#4526=VERTEX_POINT('',#45193);
#4527=VERTEX_POINT('',#45232);
#4528=VERTEX_POINT('',#45239);
#4529=VERTEX_POINT('',#45278);
#4530=VERTEX_POINT('',#45285);
#4531=VERTEX_POINT('',#45324);
#4532=VERTEX_POINT('',#45331);
#4533=VERTEX_POINT('',#45370);
#4534=VERTEX_POINT('',#45377);
#4535=VERTEX_POINT('',#45416);
#4536=VERTEX_POINT('',#45420);
#4537=VERTEX_POINT('',#45421);
#4538=VERTEX_POINT('',#45461);
#4539=VERTEX_POINT('',#45465);
#4540=VERTEX_POINT('',#45466);
#4541=VERTEX_POINT('',#45509);
#4542=VERTEX_POINT('',#45513);
#4543=VERTEX_POINT('',#45514);
#4544=VERTEX_POINT('',#45554);
#4545=VERTEX_POINT('',#45558);
#4546=VERTEX_POINT('',#45559);
#4547=VERTEX_POINT('',#45573);
#4548=VERTEX_POINT('',#45575);
#4549=VERTEX_POINT('',#45577);
#4550=VERTEX_POINT('',#45579);
#4551=VERTEX_POINT('',#45581);
#4552=VERTEX_POINT('',#45583);
#4553=VERTEX_POINT('',#45585);
#4554=VERTEX_POINT('',#45587);
#4555=VERTEX_POINT('',#45591);
#4556=VERTEX_POINT('',#45593);
#4557=VERTEX_POINT('',#45595);
#4558=VERTEX_POINT('',#45597);
#4559=VERTEX_POINT('',#45601);
#4560=VERTEX_POINT('',#45603);
#4561=VERTEX_POINT('',#45605);
#4562=VERTEX_POINT('',#45607);
#4563=VERTEX_POINT('',#45609);
#4564=VERTEX_POINT('',#45611);
#4565=VERTEX_POINT('',#45613);
#4566=VERTEX_POINT('',#45617);
#4567=VERTEX_POINT('',#45619);
#4568=VERTEX_POINT('',#45621);
#4569=VERTEX_POINT('',#45623);
#4570=VERTEX_POINT('',#45627);
#4571=VERTEX_POINT('',#45629);
#4572=VERTEX_POINT('',#45632);
#4573=VERTEX_POINT('',#45633);
#4574=VERTEX_POINT('',#45635);
#4575=VERTEX_POINT('',#45637);
#4576=VERTEX_POINT('',#45644);
#4577=VERTEX_POINT('',#45646);
#4578=VERTEX_POINT('',#45650);
#4579=VERTEX_POINT('',#45651);
#4580=VERTEX_POINT('',#45653);
#4581=VERTEX_POINT('',#45655);
#4582=VERTEX_POINT('',#45662);
#4583=VERTEX_POINT('',#45666);
#4584=VERTEX_POINT('',#45667);
#4585=VERTEX_POINT('',#45669);
#4586=VERTEX_POINT('',#45671);
#4587=VERTEX_POINT('',#45676);
#4588=VERTEX_POINT('',#45678);
#4589=VERTEX_POINT('',#45680);
#4590=VERTEX_POINT('',#45686);
#4591=VERTEX_POINT('',#45687);
#4592=VERTEX_POINT('',#45689);
#4593=VERTEX_POINT('',#45691);
#4594=VERTEX_POINT('',#45695);
#4595=VERTEX_POINT('',#45697);
#4596=VERTEX_POINT('',#45699);
#4597=VERTEX_POINT('',#45701);
#4598=VERTEX_POINT('',#45703);
#4599=VERTEX_POINT('',#45707);
#4600=VERTEX_POINT('',#45711);
#4601=VERTEX_POINT('',#45712);
#4602=VERTEX_POINT('',#45714);
#4603=VERTEX_POINT('',#45716);
#4604=VERTEX_POINT('',#45720);
#4605=VERTEX_POINT('',#45722);
#4606=VERTEX_POINT('',#45726);
#4607=VERTEX_POINT('',#45728);
#4608=VERTEX_POINT('',#45730);
#4609=VERTEX_POINT('',#45734);
#4610=VERTEX_POINT('',#45736);
#4611=VERTEX_POINT('',#45742);
#4612=VERTEX_POINT('',#45747);
#4613=VERTEX_POINT('',#45749);
#4614=VERTEX_POINT('',#45751);
#4615=VERTEX_POINT('',#45755);
#4616=VERTEX_POINT('',#45757);
#4617=VERTEX_POINT('',#45762);
#4618=VERTEX_POINT('',#45770);
#4619=VERTEX_POINT('',#45774);
#4620=VERTEX_POINT('',#45778);
#4621=VERTEX_POINT('',#45783);
#4622=VERTEX_POINT('',#45790);
#4623=VERTEX_POINT('',#45794);
#4624=VERTEX_POINT('',#45798);
#4625=VERTEX_POINT('',#45802);
#4626=VERTEX_POINT('',#45804);
#4627=VERTEX_POINT('',#45809);
#4628=VERTEX_POINT('',#45811);
#4629=VERTEX_POINT('',#45813);
#4630=VERTEX_POINT('',#45815);
#4631=VERTEX_POINT('',#45817);
#4632=VERTEX_POINT('',#45827);
#4633=VERTEX_POINT('',#45829);
#4634=VERTEX_POINT('',#45833);
#4635=VERTEX_POINT('',#45847);
#4636=VERTEX_POINT('',#45849);
#4637=VERTEX_POINT('',#45856);
#4638=VERTEX_POINT('',#45858);
#4639=VERTEX_POINT('',#45862);
#4640=VERTEX_POINT('',#45864);
#4641=VERTEX_POINT('',#45874);
#4642=VERTEX_POINT('',#45876);
#4643=VERTEX_POINT('',#45880);
#4644=VERTEX_POINT('',#45887);
#4645=VERTEX_POINT('',#45888);
#4646=VERTEX_POINT('',#45890);
#4647=VERTEX_POINT('',#45911);
#4648=VERTEX_POINT('',#45930);
#4649=VERTEX_POINT('',#45931);
#4650=VERTEX_POINT('',#46010);
#4651=VERTEX_POINT('',#46011);
#4652=VERTEX_POINT('',#46086);
#4653=VERTEX_POINT('',#46087);
#4654=VERTEX_POINT('',#46162);
#4655=VERTEX_POINT('',#46163);
#4656=VERTEX_POINT('',#46238);
#4657=VERTEX_POINT('',#46239);
#4658=VERTEX_POINT('',#46314);
#4659=VERTEX_POINT('',#46315);
#4660=VERTEX_POINT('',#46390);
#4661=VERTEX_POINT('',#46391);
#4662=VERTEX_POINT('',#46466);
#4663=VERTEX_POINT('',#46467);
#4664=VERTEX_POINT('',#46546);
#4665=VERTEX_POINT('',#46547);
#4666=VERTEX_POINT('',#46622);
#4667=VERTEX_POINT('',#46623);
#4668=VERTEX_POINT('',#46698);
#4669=VERTEX_POINT('',#46699);
#4670=VERTEX_POINT('',#46774);
#4671=VERTEX_POINT('',#46775);
#4672=VERTEX_POINT('',#46850);
#4673=VERTEX_POINT('',#46851);
#4674=VERTEX_POINT('',#46926);
#4675=VERTEX_POINT('',#46927);
#4676=VERTEX_POINT('',#47004);
#4677=VERTEX_POINT('',#47005);
#4678=VERTEX_POINT('',#47007);
#4679=VERTEX_POINT('',#47028);
#4680=VERTEX_POINT('',#47049);
#4681=VERTEX_POINT('',#47050);
#4682=VERTEX_POINT('',#47127);
#4683=VERTEX_POINT('',#47128);
#4684=VERTEX_POINT('',#47203);
#4685=VERTEX_POINT('',#47204);
#4686=VERTEX_POINT('',#47279);
#4687=VERTEX_POINT('',#47280);
#4688=VERTEX_POINT('',#47355);
#4689=VERTEX_POINT('',#47356);
#4690=VERTEX_POINT('',#47431);
#4691=VERTEX_POINT('',#47432);
#4692=VERTEX_POINT('',#47509);
#4693=VERTEX_POINT('',#47510);
#4694=VERTEX_POINT('',#47585);
#4695=VERTEX_POINT('',#47586);
#4696=VERTEX_POINT('',#47663);
#4697=VERTEX_POINT('',#47664);
#4698=VERTEX_POINT('',#47739);
#4699=VERTEX_POINT('',#47740);
#4700=VERTEX_POINT('',#47815);
#4701=VERTEX_POINT('',#47816);
#4702=VERTEX_POINT('',#47891);
#4703=VERTEX_POINT('',#47892);
#4704=VERTEX_POINT('',#47967);
#4705=VERTEX_POINT('',#47968);
#4706=VERTEX_POINT('',#48045);
#4707=VERTEX_POINT('',#48046);
#4708=VERTEX_POINT('',#48121);
#4709=VERTEX_POINT('',#48122);
#4710=VERTEX_POINT('',#48197);
#4711=VERTEX_POINT('',#48218);
#4712=VERTEX_POINT('',#48239);
#4713=VERTEX_POINT('',#48272);
#4714=VERTEX_POINT('',#48305);
#4715=VERTEX_POINT('',#48306);
#4716=VERTEX_POINT('',#48312);
#4717=VERTEX_POINT('',#48314);
#4718=VERTEX_POINT('',#48318);
#4719=VERTEX_POINT('',#48321);
#4720=VERTEX_POINT('',#48348);
#4721=VERTEX_POINT('',#49203);
#4722=VERTEX_POINT('',#49204);
#4723=VERTEX_POINT('',#49206);
#4724=VERTEX_POINT('',#49209);
#4725=VERTEX_POINT('',#49234);
#4726=VERTEX_POINT('',#49235);
#4727=VERTEX_POINT('',#49237);
#4728=VERTEX_POINT('',#49239);
#4729=VERTEX_POINT('',#49241);
#4730=VERTEX_POINT('',#49243);
#4731=VERTEX_POINT('',#49260);
#4732=VERTEX_POINT('',#49263);
#4733=VERTEX_POINT('',#49265);
#4734=VERTEX_POINT('',#49267);
#4735=VERTEX_POINT('',#49271);
#4736=VERTEX_POINT('',#49273);
#4737=VERTEX_POINT('',#49281);
#4738=VERTEX_POINT('',#49283);
#4739=VERTEX_POINT('',#49285);
#4740=VERTEX_POINT('',#49289);
#4741=VERTEX_POINT('',#49291);
#4742=VERTEX_POINT('',#49295);
#4743=VERTEX_POINT('',#49302);
#4744=VERTEX_POINT('',#49303);
#4745=VERTEX_POINT('',#49305);
#4746=VERTEX_POINT('',#49331);
#4747=VERTEX_POINT('',#49341);
#4748=VERTEX_POINT('',#49342);
#4749=VERTEX_POINT('',#49344);
#4750=VERTEX_POINT('',#49385);
#4751=VERTEX_POINT('',#49390);
#4752=VERTEX_POINT('',#49417);
#4753=VERTEX_POINT('',#49434);
#4754=VERTEX_POINT('',#49460);
#4755=VERTEX_POINT('',#49462);
#4756=VERTEX_POINT('',#49493);
#4757=VERTEX_POINT('',#49590);
#4758=VERTEX_POINT('',#49604);
#4759=VERTEX_POINT('',#49606);
#4760=VERTEX_POINT('',#49610);
#4761=VERTEX_POINT('',#49614);
#4762=VERTEX_POINT('',#49780);
#4763=VERTEX_POINT('',#49784);
#4764=VERTEX_POINT('',#49787);
#4765=VERTEX_POINT('',#49788);
#4766=EDGE_CURVE('',#3772,#3772,#3399,.T.);
#4767=EDGE_CURVE('',#3772,#3773,#2243,.T.);
#4768=EDGE_CURVE('',#3773,#3773,#3400,.T.);
#4769=EDGE_CURVE('',#3774,#3774,#3401,.T.);
#4770=EDGE_CURVE('',#3775,#3775,#3402,.T.);
#4771=EDGE_CURVE('',#3775,#3776,#2244,.T.);
#4772=EDGE_CURVE('',#3776,#3777,#3403,.T.);
#4773=EDGE_CURVE('',#3777,#3776,#3404,.T.);
#4774=EDGE_CURVE('',#3777,#3778,#3405,.T.);
#4775=EDGE_CURVE('',#3778,#3779,#3406,.T.);
#4776=EDGE_CURVE('',#3779,#3778,#3407,.T.);
#4777=EDGE_CURVE('',#3779,#3774,#2245,.T.);
#4778=EDGE_CURVE('',#3780,#3780,#3408,.T.);
#4779=EDGE_CURVE('',#3781,#3781,#3409,.T.);
#4780=EDGE_CURVE('',#3781,#3782,#2246,.T.);
#4781=EDGE_CURVE('',#3782,#3783,#3410,.T.);
#4782=EDGE_CURVE('',#3783,#3782,#3411,.T.);
#4783=EDGE_CURVE('',#3783,#3784,#3412,.T.);
#4784=EDGE_CURVE('',#3784,#3785,#3413,.T.);
#4785=EDGE_CURVE('',#3785,#3784,#3414,.T.);
#4786=EDGE_CURVE('',#3785,#3780,#2247,.T.);
#4787=EDGE_CURVE('',#3786,#3786,#3415,.T.);
#4788=EDGE_CURVE('',#3786,#3787,#3416,.T.);
#4789=EDGE_CURVE('',#3787,#3787,#3417,.T.);
#4790=EDGE_CURVE('',#3788,#3788,#3418,.T.);
#4791=EDGE_CURVE('',#3789,#3790,#3419,.T.);
#4792=EDGE_CURVE('',#3791,#3789,#2248,.T.);
#4793=EDGE_CURVE('',#3792,#3791,#3420,.T.);
#4794=EDGE_CURVE('',#3792,#3793,#2249,.T.);
#4795=EDGE_CURVE('',#3794,#3793,#3421,.T.);
#4796=EDGE_CURVE('',#3795,#3794,#2250,.T.);
#4797=EDGE_CURVE('',#3796,#3795,#3422,.T.);
#4798=EDGE_CURVE('',#3796,#3797,#2251,.T.);
#4799=EDGE_CURVE('',#3798,#3797,#3423,.T.);
#4800=EDGE_CURVE('',#3799,#3798,#2252,.T.);
#4801=EDGE_CURVE('',#3800,#3799,#3424,.T.);
#4802=EDGE_CURVE('',#3800,#3801,#2253,.T.);
#4803=EDGE_CURVE('',#3802,#3801,#3425,.T.);
#4804=EDGE_CURVE('',#3803,#3802,#2254,.T.);
#4805=EDGE_CURVE('',#3804,#3803,#3426,.T.);
#4806=EDGE_CURVE('',#3804,#3805,#2255,.T.);
#4807=EDGE_CURVE('',#3790,#3805,#3427,.T.);
#4808=EDGE_CURVE('',#3790,#3787,#2256,.T.);
#4809=EDGE_CURVE('',#3806,#3806,#3428,.T.);
#4810=EDGE_CURVE('',#3806,#3807,#3429,.T.);
#4811=EDGE_CURVE('',#3807,#3807,#3430,.T.);
#4812=EDGE_CURVE('',#3806,#3808,#2257,.T.);
#4813=EDGE_CURVE('',#3809,#3808,#3431,.T.);
#4814=EDGE_CURVE('',#3810,#3809,#687,.T.);
#4815=EDGE_CURVE('',#3811,#3810,#2258,.T.);
#4816=EDGE_CURVE('',#3812,#3811,#688,.T.);
#4817=EDGE_CURVE('',#3813,#3812,#2259,.T.);
#4818=EDGE_CURVE('',#3814,#3813,#3432,.T.);
#4819=EDGE_CURVE('',#3814,#3815,#2260,.T.);
#4820=EDGE_CURVE('',#3816,#3815,#689,.T.);
#4821=EDGE_CURVE('',#3816,#3817,#2261,.T.);
#4822=EDGE_CURVE('',#3818,#3817,#690,.T.);
#4823=EDGE_CURVE('',#3819,#3818,#3433,.T.);
#4824=EDGE_CURVE('',#3820,#3819,#691,.T.);
#4825=EDGE_CURVE('',#3821,#3820,#2262,.T.);
#4826=EDGE_CURVE('',#3822,#3821,#692,.T.);
#4827=EDGE_CURVE('',#3823,#3822,#2263,.T.);
#4828=EDGE_CURVE('',#3824,#3823,#3434,.T.);
#4829=EDGE_CURVE('',#3824,#3825,#2264,.T.);
#4830=EDGE_CURVE('',#3826,#3825,#693,.T.);
#4831=EDGE_CURVE('',#3826,#3827,#2265,.T.);
#4832=EDGE_CURVE('',#3828,#3827,#694,.T.);
#4833=EDGE_CURVE('',#3829,#3828,#3435,.T.);
#4834=EDGE_CURVE('',#3830,#3829,#695,.T.);
#4835=EDGE_CURVE('',#3831,#3830,#2266,.T.);
#4836=EDGE_CURVE('',#3832,#3831,#696,.T.);
#4837=EDGE_CURVE('',#3833,#3832,#2267,.T.);
#4838=EDGE_CURVE('',#3834,#3833,#3436,.T.);
#4839=EDGE_CURVE('',#3834,#3835,#2268,.T.);
#4840=EDGE_CURVE('',#3836,#3835,#697,.T.);
#4841=EDGE_CURVE('',#3836,#3837,#2269,.T.);
#4842=EDGE_CURVE('',#3838,#3837,#698,.T.);
#4843=EDGE_CURVE('',#3839,#3838,#3437,.T.);
#4844=EDGE_CURVE('',#3840,#3839,#699,.T.);
#4845=EDGE_CURVE('',#3841,#3840,#2270,.T.);
#4846=EDGE_CURVE('',#3842,#3841,#700,.T.);
#4847=EDGE_CURVE('',#3843,#3842,#2271,.T.);
#4848=EDGE_CURVE('',#3844,#3843,#3438,.T.);
#4849=EDGE_CURVE('',#3844,#3845,#2272,.T.);
#4850=EDGE_CURVE('',#3846,#3845,#701,.T.);
#4851=EDGE_CURVE('',#3846,#3847,#2273,.T.);
#4852=EDGE_CURVE('',#3848,#3847,#702,.T.);
#4853=EDGE_CURVE('',#3808,#3848,#3439,.T.);
#4854=EDGE_CURVE('',#3849,#3849,#3440,.T.);
#4855=EDGE_CURVE('',#3839,#3850,#2274,.T.);
#4856=EDGE_CURVE('',#3850,#3851,#665,.T.);
#4857=EDGE_CURVE('',#3851,#3840,#2275,.T.);
#4858=EDGE_CURVE('',#3850,#3852,#3441,.T.);
#4859=EDGE_CURVE('',#3853,#3852,#666,.T.);
#4860=EDGE_CURVE('',#3853,#3851,#3442,.T.);
#4861=EDGE_CURVE('',#3852,#3838,#2276,.T.);
#4862=EDGE_CURVE('',#3837,#3853,#2277,.T.);
#4863=EDGE_CURVE('',#3829,#3854,#2278,.T.);
#4864=EDGE_CURVE('',#3854,#3855,#667,.T.);
#4865=EDGE_CURVE('',#3855,#3830,#2279,.T.);
#4866=EDGE_CURVE('',#3856,#3828,#2280,.T.);
#4867=EDGE_CURVE('',#3854,#3856,#3443,.T.);
#4868=EDGE_CURVE('',#3857,#3858,#668,.T.);
#4869=EDGE_CURVE('',#3858,#3848,#2281,.T.);
#4870=EDGE_CURVE('',#3847,#3857,#2282,.T.);
#4871=EDGE_CURVE('',#3859,#3858,#3444,.T.);
#4872=EDGE_CURVE('',#3809,#3859,#2283,.T.);
#4873=EDGE_CURVE('',#3859,#3860,#669,.T.);
#4874=EDGE_CURVE('',#3860,#3810,#2284,.T.);
#4875=EDGE_CURVE('',#3861,#3862,#670,.T.);
#4876=EDGE_CURVE('',#3862,#3818,#2285,.T.);
#4877=EDGE_CURVE('',#3817,#3861,#2286,.T.);
#4878=EDGE_CURVE('',#3863,#3862,#3445,.T.);
#4879=EDGE_CURVE('',#3819,#3863,#2287,.T.);
#4880=EDGE_CURVE('',#3861,#3864,#3446,.T.);
#4881=EDGE_CURVE('',#3863,#3864,#671,.T.);
#4882=EDGE_CURVE('',#3865,#3856,#672,.T.);
#4883=EDGE_CURVE('',#3827,#3865,#2288,.T.);
#4884=EDGE_CURVE('',#3865,#3855,#3447,.T.);
#4885=EDGE_CURVE('',#3864,#3820,#2289,.T.);
#4886=EDGE_CURVE('',#3866,#3864,#2290,.T.);
#4887=EDGE_CURVE('',#3821,#3866,#2291,.T.);
#4888=EDGE_CURVE('',#3831,#3867,#2292,.T.);
#4889=EDGE_CURVE('',#3867,#3868,#3448,.T.);
#4890=EDGE_CURVE('',#3868,#3797,#2293,.T.);
#4891=EDGE_CURVE('',#3797,#3832,#2294,.T.);
#4892=EDGE_CURVE('',#3869,#3868,#3449,.T.);
#4893=EDGE_CURVE('',#3798,#3869,#2295,.T.);
#4894=EDGE_CURVE('',#3867,#3870,#3450,.T.);
#4895=EDGE_CURVE('',#3869,#3870,#3451,.T.);
#4896=EDGE_CURVE('',#3871,#3872,#673,.T.);
#4897=EDGE_CURVE('',#3872,#3836,#2296,.T.);
#4898=EDGE_CURVE('',#3835,#3794,#2297,.T.);
#4899=EDGE_CURVE('',#3794,#3871,#2298,.T.);
#4900=EDGE_CURVE('',#3871,#3873,#3452,.T.);
#4901=EDGE_CURVE('',#3874,#3873,#674,.T.);
#4902=EDGE_CURVE('',#3874,#3872,#3453,.T.);
#4903=EDGE_CURVE('',#3873,#3793,#2299,.T.);
#4904=EDGE_CURVE('',#3841,#3874,#2300,.T.);
#4905=EDGE_CURVE('',#3793,#3842,#2301,.T.);
#4906=EDGE_CURVE('',#3874,#3851,#2302,.T.);
#4907=EDGE_CURVE('',#3875,#3876,#3454,.T.);
#4908=EDGE_CURVE('',#3876,#3846,#2303,.T.);
#4909=EDGE_CURVE('',#3845,#3789,#2304,.T.);
#4910=EDGE_CURVE('',#3789,#3875,#2305,.T.);
#4911=EDGE_CURVE('',#3875,#3877,#3455,.T.);
#4912=EDGE_CURVE('',#3878,#3877,#3456,.T.);
#4913=EDGE_CURVE('',#3878,#3876,#3457,.T.);
#4914=EDGE_CURVE('',#3877,#3805,#2306,.T.);
#4915=EDGE_CURVE('',#3811,#3878,#2307,.T.);
#4916=EDGE_CURVE('',#3805,#3812,#2308,.T.);
#4917=EDGE_CURVE('',#3878,#3860,#2309,.T.);
#4918=EDGE_CURVE('',#3879,#3880,#675,.T.);
#4919=EDGE_CURVE('',#3880,#3816,#2310,.T.);
#4920=EDGE_CURVE('',#3815,#3802,#2311,.T.);
#4921=EDGE_CURVE('',#3802,#3879,#2312,.T.);
#4922=EDGE_CURVE('',#3879,#3881,#3458,.T.);
#4923=EDGE_CURVE('',#3866,#3881,#676,.T.);
#4924=EDGE_CURVE('',#3866,#3880,#3459,.T.);
#4925=EDGE_CURVE('',#3881,#3801,#2313,.T.);
#4926=EDGE_CURVE('',#3870,#3826,#2314,.T.);
#4927=EDGE_CURVE('',#3825,#3798,#2315,.T.);
#4928=EDGE_CURVE('',#3801,#3822,#2316,.T.);
#4929=EDGE_CURVE('',#3795,#3834,#2317,.T.);
#4930=EDGE_CURVE('',#3843,#3792,#2318,.T.);
#4931=EDGE_CURVE('',#3799,#3824,#2319,.T.);
#4932=EDGE_CURVE('',#3833,#3796,#2320,.T.);
#4933=EDGE_CURVE('',#3791,#3844,#2321,.T.);
#4934=EDGE_CURVE('',#3813,#3804,#2322,.T.);
#4935=EDGE_CURVE('',#3803,#3814,#2323,.T.);
#4936=EDGE_CURVE('',#3823,#3800,#2324,.T.);
#4937=EDGE_CURVE('',#3788,#3849,#2325,.T.);
#4938=EDGE_CURVE('',#3867,#3855,#2326,.T.);
#4939=EDGE_CURVE('',#3870,#3865,#2327,.T.);
#4940=EDGE_CURVE('',#3857,#3860,#3460,.T.);
#4941=EDGE_CURVE('',#3876,#3857,#2328,.T.);
#4942=EDGE_CURVE('',#3880,#3861,#2329,.T.);
#4943=EDGE_CURVE('',#3872,#3853,#2330,.T.);
#4944=EDGE_CURVE('',#3882,#3883,#141,.T.);
#4945=EDGE_CURVE('',#3883,#3884,#142,.T.);
#4946=EDGE_CURVE('',#3884,#3885,#143,.T.);
#4947=EDGE_CURVE('',#3885,#3886,#144,.T.);
#4948=EDGE_CURVE('',#3886,#3887,#145,.T.);
#4949=EDGE_CURVE('',#3887,#3888,#146,.T.);
#4950=EDGE_CURVE('',#3888,#3889,#147,.T.);
#4951=EDGE_CURVE('',#3889,#3890,#148,.T.);
#4952=EDGE_CURVE('',#3890,#3891,#149,.T.);
#4953=EDGE_CURVE('',#3891,#3892,#150,.T.);
#4954=EDGE_CURVE('',#3892,#3893,#151,.T.);
#4955=EDGE_CURVE('',#3894,#3893,#3461,.T.);
#4956=EDGE_CURVE('',#3895,#3894,#152,.F.);
#4957=EDGE_CURVE('',#3896,#3895,#153,.F.);
#4958=EDGE_CURVE('',#3897,#3896,#154,.F.);
#4959=EDGE_CURVE('',#3898,#3897,#155,.F.);
#4960=EDGE_CURVE('',#3899,#3898,#156,.F.);
#4961=EDGE_CURVE('',#3900,#3899,#157,.F.);
#4962=EDGE_CURVE('',#3901,#3900,#158,.F.);
#4963=EDGE_CURVE('',#3902,#3901,#159,.F.);
#4964=EDGE_CURVE('',#3903,#3902,#160,.F.);
#4965=EDGE_CURVE('',#3904,#3903,#161,.F.);
#4966=EDGE_CURVE('',#3905,#3904,#162,.F.);
#4967=EDGE_CURVE('',#3906,#3905,#163,.F.);
#4968=EDGE_CURVE('',#3907,#3906,#164,.F.);
#4969=EDGE_CURVE('',#3908,#3907,#165,.F.);
#4970=EDGE_CURVE('',#3909,#3908,#166,.F.);
#4971=EDGE_CURVE('',#3910,#3909,#3462,.T.);
#4972=EDGE_CURVE('',#3910,#3911,#167,.T.);
#4973=EDGE_CURVE('',#3911,#3912,#168,.T.);
#4974=EDGE_CURVE('',#3912,#3913,#169,.T.);
#4975=EDGE_CURVE('',#3913,#3882,#170,.T.);
#4976=EDGE_CURVE('',#3914,#3915,#171,.T.);
#4977=EDGE_CURVE('',#3915,#3916,#172,.T.);
#4978=EDGE_CURVE('',#3916,#3917,#173,.T.);
#4979=EDGE_CURVE('',#3917,#3918,#174,.T.);
#4980=EDGE_CURVE('',#3918,#3919,#175,.T.);
#4981=EDGE_CURVE('',#3919,#3920,#176,.T.);
#4982=EDGE_CURVE('',#3920,#3921,#177,.T.);
#4983=EDGE_CURVE('',#3921,#3922,#178,.T.);
#4984=EDGE_CURVE('',#3922,#3923,#179,.T.);
#4985=EDGE_CURVE('',#3923,#3924,#3463,.T.);
#4986=EDGE_CURVE('',#3924,#3925,#180,.T.);
#4987=EDGE_CURVE('',#3925,#3926,#181,.T.);
#4988=EDGE_CURVE('',#3926,#3927,#182,.T.);
#4989=EDGE_CURVE('',#3927,#3928,#183,.T.);
#4990=EDGE_CURVE('',#3928,#3929,#184,.T.);
#4991=EDGE_CURVE('',#3929,#3930,#185,.T.);
#4992=EDGE_CURVE('',#3930,#3931,#186,.T.);
#4993=EDGE_CURVE('',#3931,#3932,#187,.T.);
#4994=EDGE_CURVE('',#3932,#3933,#188,.T.);
#4995=EDGE_CURVE('',#3933,#3934,#189,.T.);
#4996=EDGE_CURVE('',#3934,#3935,#190,.T.);
#4997=EDGE_CURVE('',#3935,#3936,#191,.T.);
#4998=EDGE_CURVE('',#3936,#3937,#192,.T.);
#4999=EDGE_CURVE('',#3937,#3938,#193,.T.);
#5000=EDGE_CURVE('',#3938,#3939,#194,.T.);
#5001=EDGE_CURVE('',#3940,#3939,#3464,.T.);
#5002=EDGE_CURVE('',#3940,#3941,#195,.T.);
#5003=EDGE_CURVE('',#3941,#3942,#196,.T.);
#5004=EDGE_CURVE('',#3942,#3943,#197,.T.);
#5005=EDGE_CURVE('',#3943,#3944,#198,.T.);
#5006=EDGE_CURVE('',#3944,#3914,#199,.T.);
#5007=EDGE_CURVE('',#3945,#3945,#3465,.T.);
#5008=EDGE_CURVE('',#3946,#3946,#3466,.T.);
#5009=EDGE_CURVE('',#3946,#3947,#2331,.T.);
#5010=EDGE_CURVE('',#3947,#3947,#3467,.T.);
#5011=EDGE_CURVE('',#3948,#3948,#3468,.T.);
#5012=EDGE_CURVE('',#3946,#3949,#2332,.T.);
#5013=EDGE_CURVE('',#3949,#3950,#3469,.T.);
#5014=EDGE_CURVE('',#3950,#3949,#3470,.T.);
#5015=EDGE_CURVE('',#3951,#3951,#3471,.T.);
#5016=EDGE_CURVE('',#3951,#3952,#2333,.T.);
#5017=EDGE_CURVE('',#3952,#3952,#3472,.T.);
#5018=EDGE_CURVE('',#3951,#3953,#2334,.T.);
#5019=EDGE_CURVE('',#3953,#3953,#3473,.T.);
#5020=EDGE_CURVE('',#3954,#3954,#3474,.T.);
#5021=EDGE_CURVE('',#3953,#3948,#2335,.T.);
#5022=EDGE_CURVE('',#3955,#3956,#3475,.T.);
#5023=EDGE_CURVE('',#3956,#3950,#2336,.T.);
#5024=EDGE_CURVE('',#3956,#3955,#3476,.T.);
#5025=EDGE_CURVE('',#3955,#3957,#2337,.T.);
#5026=EDGE_CURVE('',#3958,#3957,#3477,.T.);
#5027=EDGE_CURVE('',#3957,#3958,#3478,.T.);
#5028=EDGE_CURVE('',#3923,#3894,#200,.T.);
#5029=EDGE_CURVE('',#3893,#3924,#201,.T.);
#5030=EDGE_CURVE('',#3939,#3910,#202,.T.);
#5031=EDGE_CURVE('',#3909,#3940,#203,.T.);
#5032=EDGE_CURVE('',#3958,#3945,#2338,.T.);
#5033=EDGE_CURVE('',#3959,#3959,#3479,.T.);
#5034=EDGE_CURVE('',#3960,#3960,#3480,.T.);
#5035=EDGE_CURVE('',#3961,#3961,#3481,.T.);
#5036=EDGE_CURVE('',#3962,#3962,#3482,.T.);
#5037=EDGE_CURVE('',#3963,#3963,#3483,.T.);
#5038=EDGE_CURVE('',#3964,#3964,#3484,.T.);
#5039=EDGE_CURVE('',#3965,#3965,#3485,.T.);
#5040=EDGE_CURVE('',#3966,#3966,#3486,.T.);
#5041=EDGE_CURVE('',#3967,#3967,#3487,.T.);
#5042=EDGE_CURVE('',#3968,#3968,#3488,.T.);
#5043=EDGE_CURVE('',#3969,#3969,#3489,.T.);
#5044=EDGE_CURVE('',#3970,#3970,#3490,.T.);
#5045=EDGE_CURVE('',#3971,#3971,#3491,.T.);
#5046=EDGE_CURVE('',#3972,#3972,#3492,.T.);
#5047=EDGE_CURVE('',#3973,#3973,#3493,.T.);
#5048=EDGE_CURVE('',#3974,#3974,#3494,.T.);
#5049=EDGE_CURVE('',#3975,#3975,#3495,.T.);
#5050=EDGE_CURVE('',#3976,#3976,#3496,.T.);
#5051=EDGE_CURVE('',#3977,#3977,#3497,.T.);
#5052=EDGE_CURVE('',#3978,#3978,#3498,.T.);
#5053=EDGE_CURVE('',#3979,#3979,#3499,.T.);
#5054=EDGE_CURVE('',#3980,#3980,#3500,.T.);
#5055=EDGE_CURVE('',#3981,#3981,#3501,.T.);
#5056=EDGE_CURVE('',#3982,#3982,#3502,.T.);
#5057=EDGE_CURVE('',#3983,#3983,#3503,.T.);
#5058=EDGE_CURVE('',#3984,#3984,#3504,.T.);
#5059=EDGE_CURVE('',#3985,#3985,#3505,.T.);
#5060=EDGE_CURVE('',#3986,#3986,#3506,.T.);
#5061=EDGE_CURVE('',#3987,#3987,#3507,.T.);
#5062=EDGE_CURVE('',#3988,#3988,#3508,.T.);
#5063=EDGE_CURVE('',#3989,#3989,#3509,.T.);
#5064=EDGE_CURVE('',#3989,#3959,#2339,.T.);
#5065=EDGE_CURVE('',#3963,#3961,#2340,.T.);
#5066=EDGE_CURVE('',#3967,#3965,#2341,.T.);
#5067=EDGE_CURVE('',#3971,#3969,#2342,.T.);
#5068=EDGE_CURVE('',#3975,#3973,#2343,.T.);
#5069=EDGE_CURVE('',#3979,#3977,#2344,.T.);
#5070=EDGE_CURVE('',#3983,#3981,#2345,.T.);
#5071=EDGE_CURVE('',#3985,#3987,#2346,.T.);
#5072=EDGE_CURVE('',#3988,#3990,#2347,.T.);
#5073=EDGE_CURVE('',#3990,#3990,#3510,.T.);
#5074=EDGE_CURVE('',#3978,#3984,#2348,.T.);
#5075=EDGE_CURVE('',#3974,#3980,#2349,.T.);
#5076=EDGE_CURVE('',#3970,#3976,#2350,.T.);
#5077=EDGE_CURVE('',#3966,#3972,#2351,.T.);
#5078=EDGE_CURVE('',#3962,#3968,#2352,.T.);
#5079=EDGE_CURVE('',#3960,#3964,#2353,.T.);
#5080=EDGE_CURVE('',#3991,#3991,#3511,.T.);
#5081=EDGE_CURVE('',#3991,#3992,#2354,.T.);
#5082=EDGE_CURVE('',#3992,#3992,#3512,.T.);
#5083=EDGE_CURVE('',#3993,#3993,#3513,.T.);
#5084=EDGE_CURVE('',#3993,#3994,#2355,.T.);
#5085=EDGE_CURVE('',#3994,#3994,#3514,.T.);
#5086=EDGE_CURVE('',#3995,#3995,#3515,.T.);
#5087=EDGE_CURVE('',#3995,#3996,#2356,.T.);
#5088=EDGE_CURVE('',#3996,#3996,#3516,.T.);
#5089=EDGE_CURVE('',#3997,#3997,#3517,.T.);
#5090=EDGE_CURVE('',#3997,#3998,#2357,.T.);
#5091=EDGE_CURVE('',#3998,#3998,#3518,.T.);
#5092=EDGE_CURVE('',#3982,#3986,#2358,.T.);
#5093=EDGE_CURVE('',#3999,#3999,#3519,.T.);
#5094=EDGE_CURVE('',#4000,#4000,#3520,.T.);
#5095=EDGE_CURVE('',#4000,#3999,#2359,.T.);
#5096=EDGE_CURVE('',#4001,#4001,#3521,.T.);
#5097=EDGE_CURVE('',#4002,#4002,#3522,.T.);
#5098=EDGE_CURVE('',#4002,#4001,#2360,.T.);
#5099=EDGE_CURVE('',#4003,#4003,#3523,.T.);
#5100=EDGE_CURVE('',#4004,#4004,#3524,.T.);
#5101=EDGE_CURVE('',#4004,#4003,#2361,.T.);
#5102=EDGE_CURVE('',#4005,#4005,#3525,.T.);
#5103=EDGE_CURVE('',#4006,#4006,#3526,.T.);
#5104=EDGE_CURVE('',#4006,#4005,#2362,.T.);
#5105=EDGE_CURVE('',#4007,#4007,#3527,.T.);
#5106=EDGE_CURVE('',#4008,#4008,#3528,.T.);
#5107=EDGE_CURVE('',#4009,#4009,#3529,.T.);
#5108=EDGE_CURVE('',#4009,#4007,#2363,.T.);
#5109=EDGE_CURVE('',#4008,#3954,#2364,.T.);
#5110=EDGE_CURVE('',#4010,#4011,#2365,.T.);
#5111=EDGE_CURVE('',#4011,#4012,#2366,.T.);
#5112=EDGE_CURVE('',#4012,#4013,#703,.T.);
#5113=EDGE_CURVE('',#4010,#4013,#2367,.T.);
#5114=EDGE_CURVE('',#4014,#4011,#2368,.T.);
#5115=EDGE_CURVE('',#4012,#4014,#3530,.T.);
#5116=EDGE_CURVE('',#4015,#4016,#704,.T.);
#5117=EDGE_CURVE('',#4016,#4017,#2369,.T.);
#5118=EDGE_CURVE('',#4017,#4018,#2370,.T.);
#5119=EDGE_CURVE('',#4015,#4018,#2371,.T.);
#5120=EDGE_CURVE('',#4019,#4016,#3531,.T.);
#5121=EDGE_CURVE('',#4017,#4019,#2372,.T.);
#5122=EDGE_CURVE('',#4020,#4014,#2373,.T.);
#5123=EDGE_CURVE('',#4020,#4021,#3532,.T.);
#5124=EDGE_CURVE('',#4021,#4022,#2374,.T.);
#5125=EDGE_CURVE('',#4013,#4022,#3533,.T.);
#5126=EDGE_CURVE('',#4023,#4010,#2375,.T.);
#5127=EDGE_CURVE('',#4024,#4023,#2376,.T.);
#5128=EDGE_CURVE('',#4024,#4020,#2377,.T.);
#5129=EDGE_CURVE('',#4025,#4019,#2378,.T.);
#5130=EDGE_CURVE('',#4026,#4025,#2379,.T.);
#5131=EDGE_CURVE('',#4026,#4027,#2380,.T.);
#5132=EDGE_CURVE('',#4018,#4027,#2381,.T.);
#5133=EDGE_CURVE('',#4028,#4029,#2382,.T.);
#5134=EDGE_CURVE('',#4028,#4030,#2383,.T.);
#5135=EDGE_CURVE('',#4031,#4030,#2384,.T.);
#5136=EDGE_CURVE('',#4029,#4031,#2385,.T.);
#5137=EDGE_CURVE('',#4032,#4033,#2386,.T.);
#5138=EDGE_CURVE('',#4032,#4034,#2387,.T.);
#5139=EDGE_CURVE('',#4035,#4034,#2388,.T.);
#5140=EDGE_CURVE('',#4033,#4035,#2389,.T.);
#5141=EDGE_CURVE('',#4030,#4035,#2390,.T.);
#5142=EDGE_CURVE('',#4034,#4031,#2391,.T.);
#5143=EDGE_CURVE('',#4024,#4026,#3534,.T.);
#5144=EDGE_CURVE('',#4027,#4023,#3535,.T.);
#5145=EDGE_CURVE('',#4036,#4015,#3536,.T.);
#5146=EDGE_CURVE('',#4037,#4036,#2392,.T.);
#5147=EDGE_CURVE('',#4037,#4025,#3537,.T.);
#5148=EDGE_CURVE('',#4037,#4028,#2393,.T.);
#5149=EDGE_CURVE('',#4033,#4036,#2394,.T.);
#5150=EDGE_CURVE('',#4029,#4021,#2395,.T.);
#5151=EDGE_CURVE('',#4022,#4032,#2396,.T.);
#5152=EDGE_CURVE('',#4038,#4038,#3538,.T.);
#5153=EDGE_CURVE('',#4039,#4039,#3539,.T.);
#5154=EDGE_CURVE('',#4039,#4040,#2397,.T.);
#5155=EDGE_CURVE('',#4040,#4041,#3540,.T.);
#5156=EDGE_CURVE('',#4041,#4040,#3541,.T.);
#5157=EDGE_CURVE('',#4041,#4042,#3542,.T.);
#5158=EDGE_CURVE('',#4042,#4043,#3543,.T.);
#5159=EDGE_CURVE('',#4043,#4042,#3544,.T.);
#5160=EDGE_CURVE('',#4043,#4038,#2398,.T.);
#5161=EDGE_CURVE('',#4044,#4044,#3545,.T.);
#5162=EDGE_CURVE('',#4044,#4045,#2399,.T.);
#5163=EDGE_CURVE('',#4045,#4046,#3546,.T.);
#5164=EDGE_CURVE('',#4046,#4045,#3547,.T.);
#5165=EDGE_CURVE('',#4046,#4047,#3548,.T.);
#5166=EDGE_CURVE('',#4047,#4048,#3549,.T.);
#5167=EDGE_CURVE('',#4048,#4047,#3550,.T.);
#5168=EDGE_CURVE('',#4048,#4049,#2400,.T.);
#5169=EDGE_CURVE('',#4049,#4049,#3551,.T.);
#5170=EDGE_CURVE('',#4050,#4050,#3552,.T.);
#5171=EDGE_CURVE('',#4050,#4051,#2401,.T.);
#5172=EDGE_CURVE('',#4051,#4052,#3553,.T.);
#5173=EDGE_CURVE('',#4052,#4051,#3554,.T.);
#5174=EDGE_CURVE('',#4052,#4053,#3555,.T.);
#5175=EDGE_CURVE('',#4053,#4054,#3556,.T.);
#5176=EDGE_CURVE('',#4054,#4053,#3557,.T.);
#5177=EDGE_CURVE('',#4054,#4055,#2402,.T.);
#5178=EDGE_CURVE('',#4055,#4055,#3558,.T.);
#5179=EDGE_CURVE('',#4056,#4057,#2403,.T.);
#5180=EDGE_CURVE('',#4057,#4058,#204,.T.);
#5181=EDGE_CURVE('',#4058,#4059,#205,.T.);
#5182=EDGE_CURVE('',#4060,#4059,#206,.T.);
#5183=EDGE_CURVE('',#4061,#4060,#207,.F.);
#5184=EDGE_CURVE('',#4056,#4061,#208,.T.);
#5185=EDGE_CURVE('',#4062,#4063,#2404,.T.);
#5186=EDGE_CURVE('',#4063,#4064,#209,.F.);
#5187=EDGE_CURVE('',#4064,#4057,#210,.T.);
#5188=EDGE_CURVE('',#4062,#4056,#211,.T.);
#5189=EDGE_CURVE('',#4065,#4066,#2405,.T.);
#5190=EDGE_CURVE('',#4066,#4063,#212,.F.);
#5191=EDGE_CURVE('',#4067,#4062,#213,.T.);
#5192=EDGE_CURVE('',#4065,#4067,#214,.T.);
#5193=EDGE_CURVE('',#4068,#4069,#2406,.T.);
#5194=EDGE_CURVE('',#4069,#4066,#215,.F.);
#5195=EDGE_CURVE('',#4068,#4065,#216,.T.);
#5196=EDGE_CURVE('',#4070,#4071,#2407,.T.);
#5197=EDGE_CURVE('',#4071,#4069,#217,.F.);
#5198=EDGE_CURVE('',#4070,#4068,#218,.T.);
#5199=EDGE_CURVE('',#4072,#4073,#2408,.T.);
#5200=EDGE_CURVE('',#4073,#4071,#219,.F.);
#5201=EDGE_CURVE('',#4072,#4070,#220,.T.);
#5202=EDGE_CURVE('',#4074,#4075,#2409,.T.);
#5203=EDGE_CURVE('',#4075,#4076,#221,.T.);
#5204=EDGE_CURVE('',#4076,#4073,#222,.F.);
#5205=EDGE_CURVE('',#4074,#4072,#223,.T.);
#5206=EDGE_CURVE('',#4077,#4078,#2410,.T.);
#5207=EDGE_CURVE('',#4079,#4077,#224,.F.);
#5208=EDGE_CURVE('',#4080,#4079,#3559,.T.);
#5209=EDGE_CURVE('',#4080,#4078,#225,.T.);
#5210=EDGE_CURVE('',#4081,#4082,#2411,.T.);
#5211=EDGE_CURVE('',#4082,#4083,#226,.T.);
#5212=EDGE_CURVE('',#4083,#4084,#227,.T.);
#5213=EDGE_CURVE('',#4085,#4084,#3560,.T.);
#5214=EDGE_CURVE('',#4081,#4085,#228,.F.);
#5215=EDGE_CURVE('',#4086,#4087,#2412,.T.);
#5216=EDGE_CURVE('',#4087,#4088,#229,.T.);
#5217=EDGE_CURVE('',#4088,#4082,#230,.T.);
#5218=EDGE_CURVE('',#4089,#4081,#231,.F.);
#5219=EDGE_CURVE('',#4086,#4089,#232,.F.);
#5220=EDGE_CURVE('',#4090,#4091,#2413,.T.);
#5221=EDGE_CURVE('',#4091,#4087,#233,.T.);
#5222=EDGE_CURVE('',#4090,#4086,#234,.F.);
#5223=EDGE_CURVE('',#4092,#4093,#2414,.T.);
#5224=EDGE_CURVE('',#4093,#4091,#235,.T.);
#5225=EDGE_CURVE('',#4092,#4090,#236,.F.);
#5226=EDGE_CURVE('',#4094,#4095,#2415,.T.);
#5227=EDGE_CURVE('',#4095,#4093,#237,.T.);
#5228=EDGE_CURVE('',#4094,#4092,#238,.F.);
#5229=EDGE_CURVE('',#4096,#4097,#2416,.T.);
#5230=EDGE_CURVE('',#4097,#4098,#239,.T.);
#5231=EDGE_CURVE('',#4098,#4095,#240,.T.);
#5232=EDGE_CURVE('',#4099,#4094,#241,.F.);
#5233=EDGE_CURVE('',#4096,#4099,#242,.F.);
#5234=EDGE_CURVE('',#4100,#4101,#2417,.T.);
#5235=EDGE_CURVE('',#4101,#4097,#243,.T.);
#5236=EDGE_CURVE('',#4100,#4096,#244,.F.);
#5237=EDGE_CURVE('',#4102,#4103,#2418,.T.);
#5238=EDGE_CURVE('',#4103,#4101,#245,.T.);
#5239=EDGE_CURVE('',#4102,#4100,#246,.F.);
#5240=EDGE_CURVE('',#4104,#4105,#2419,.T.);
#5241=EDGE_CURVE('',#4105,#4103,#247,.T.);
#5242=EDGE_CURVE('',#4104,#4102,#248,.F.);
#5243=EDGE_CURVE('',#4106,#4107,#2420,.T.);
#5244=EDGE_CURVE('',#4107,#4105,#249,.T.);
#5245=EDGE_CURVE('',#4106,#4104,#250,.F.);
#5246=EDGE_CURVE('',#4108,#4109,#2421,.T.);
#5247=EDGE_CURVE('',#4109,#4107,#251,.T.);
#5248=EDGE_CURVE('',#4110,#4106,#252,.F.);
#5249=EDGE_CURVE('',#4108,#4110,#253,.F.);
#5250=EDGE_CURVE('',#4111,#4112,#2422,.T.);
#5251=EDGE_CURVE('',#4112,#4113,#254,.T.);
#5252=EDGE_CURVE('',#4113,#4109,#255,.T.);
#5253=EDGE_CURVE('',#4111,#4108,#256,.F.);
#5254=EDGE_CURVE('',#4114,#4115,#2423,.T.);
#5255=EDGE_CURVE('',#4116,#4114,#257,.F.);
#5256=EDGE_CURVE('',#4117,#4116,#3561,.T.);
#5257=EDGE_CURVE('',#4117,#4115,#258,.T.);
#5258=EDGE_CURVE('',#4118,#4119,#2424,.T.);
#5259=EDGE_CURVE('',#4119,#4120,#259,.T.);
#5260=EDGE_CURVE('',#4121,#4120,#260,.F.);
#5261=EDGE_CURVE('',#4121,#4118,#261,.T.);
#5262=EDGE_CURVE('',#4122,#4123,#2425,.T.);
#5263=EDGE_CURVE('',#4123,#4119,#262,.T.);
#5264=EDGE_CURVE('',#4118,#4122,#263,.T.);
#5265=EDGE_CURVE('',#4124,#4125,#2426,.T.);
#5266=EDGE_CURVE('',#4125,#4123,#264,.T.);
#5267=EDGE_CURVE('',#4122,#4124,#265,.T.);
#5268=EDGE_CURVE('',#4126,#4127,#2427,.T.);
#5269=EDGE_CURVE('',#4127,#4125,#266,.T.);
#5270=EDGE_CURVE('',#4124,#4126,#267,.T.);
#5271=EDGE_CURVE('',#4128,#4129,#2428,.T.);
#5272=EDGE_CURVE('',#4129,#4127,#268,.T.);
#5273=EDGE_CURVE('',#4126,#4128,#269,.T.);
#5274=EDGE_CURVE('',#4130,#4131,#2429,.T.);
#5275=EDGE_CURVE('',#4131,#4129,#270,.T.);
#5276=EDGE_CURVE('',#4128,#4130,#271,.T.);
#5277=EDGE_CURVE('',#4132,#4133,#2430,.T.);
#5278=EDGE_CURVE('',#4132,#4134,#272,.T.);
#5279=EDGE_CURVE('',#4135,#4134,#3562,.T.);
#5280=EDGE_CURVE('',#4135,#4133,#273,.T.);
#5281=EDGE_CURVE('',#4136,#4137,#2431,.T.);
#5282=EDGE_CURVE('',#4137,#4138,#274,.T.);
#5283=EDGE_CURVE('',#4139,#4138,#3563,.T.);
#5284=EDGE_CURVE('',#4139,#4136,#275,.T.);
#5285=EDGE_CURVE('',#4140,#4141,#2432,.T.);
#5286=EDGE_CURVE('',#4141,#4137,#276,.T.);
#5287=EDGE_CURVE('',#4136,#4140,#277,.T.);
#5288=EDGE_CURVE('',#4142,#4143,#2433,.T.);
#5289=EDGE_CURVE('',#4143,#4141,#278,.T.);
#5290=EDGE_CURVE('',#4140,#4142,#279,.T.);
#5291=EDGE_CURVE('',#4144,#4145,#2434,.T.);
#5292=EDGE_CURVE('',#4145,#4143,#280,.T.);
#5293=EDGE_CURVE('',#4142,#4144,#281,.T.);
#5294=EDGE_CURVE('',#4146,#4147,#2435,.T.);
#5295=EDGE_CURVE('',#4147,#4145,#282,.T.);
#5296=EDGE_CURVE('',#4144,#4146,#283,.T.);
#5297=EDGE_CURVE('',#4148,#4149,#2436,.T.);
#5298=EDGE_CURVE('',#4149,#4147,#284,.T.);
#5299=EDGE_CURVE('',#4146,#4148,#285,.T.);
#5300=EDGE_CURVE('',#4150,#4151,#2437,.T.);
#5301=EDGE_CURVE('',#4151,#4149,#286,.T.);
#5302=EDGE_CURVE('',#4148,#4150,#287,.T.);
#5303=EDGE_CURVE('',#4152,#4153,#2438,.T.);
#5304=EDGE_CURVE('',#4153,#4151,#288,.T.);
#5305=EDGE_CURVE('',#4150,#4152,#289,.T.);
#5306=EDGE_CURVE('',#4154,#4155,#2439,.T.);
#5307=EDGE_CURVE('',#4155,#4153,#290,.T.);
#5308=EDGE_CURVE('',#4152,#4154,#291,.T.);
#5309=EDGE_CURVE('',#4156,#4157,#2440,.T.);
#5310=EDGE_CURVE('',#4157,#4155,#292,.T.);
#5311=EDGE_CURVE('',#4154,#4156,#293,.T.);
#5312=EDGE_CURVE('',#4158,#4159,#2441,.T.);
#5313=EDGE_CURVE('',#4159,#4157,#294,.T.);
#5314=EDGE_CURVE('',#4156,#4158,#295,.T.);
#5315=EDGE_CURVE('',#4160,#4161,#2442,.T.);
#5316=EDGE_CURVE('',#4160,#4162,#296,.T.);
#5317=EDGE_CURVE('',#4163,#4162,#3564,.T.);
#5318=EDGE_CURVE('',#4163,#4161,#297,.T.);
#5319=EDGE_CURVE('',#4161,#4159,#298,.T.);
#5320=EDGE_CURVE('',#4158,#4160,#299,.T.);
#5321=EDGE_CURVE('',#4133,#4131,#300,.T.);
#5322=EDGE_CURVE('',#4130,#4132,#301,.T.);
#5323=EDGE_CURVE('',#4164,#4165,#2443,.T.);
#5324=EDGE_CURVE('',#4164,#4166,#2444,.T.);
#5325=EDGE_CURVE('',#4167,#4166,#2445,.T.);
#5326=EDGE_CURVE('',#4165,#4167,#2446,.T.);
#5327=EDGE_CURVE('',#4168,#4165,#2447,.T.);
#5328=EDGE_CURVE('',#4167,#4169,#2448,.T.);
#5329=EDGE_CURVE('',#4169,#4168,#2449,.T.);
#5330=EDGE_CURVE('',#4166,#4170,#2450,.T.);
#5331=EDGE_CURVE('',#4170,#4171,#2451,.T.);
#5332=EDGE_CURVE('',#4171,#4167,#2452,.T.);
#5333=EDGE_CURVE('',#4172,#4173,#677,.F.);
#5334=EDGE_CURVE('',#4170,#4172,#2453,.T.);
#5335=EDGE_CURVE('',#4174,#4164,#2454,.T.);
#5336=EDGE_CURVE('',#4175,#4174,#2455,.T.);
#5337=EDGE_CURVE('',#4176,#4175,#678,.F.);
#5338=EDGE_CURVE('',#4176,#4173,#2456,.T.);
#5339=EDGE_CURVE('',#4177,#4177,#3565,.T.);
#5340=EDGE_CURVE('',#4165,#4178,#2457,.T.);
#5341=EDGE_CURVE('',#4178,#4174,#2458,.T.);
#5342=EDGE_CURVE('',#4179,#4180,#2459,.T.);
#5343=EDGE_CURVE('',#4168,#4179,#2460,.T.);
#5344=EDGE_CURVE('',#4181,#4169,#2461,.T.);
#5345=EDGE_CURVE('',#4182,#4181,#2462,.T.);
#5346=EDGE_CURVE('',#4183,#4182,#3566,.T.);
#5347=EDGE_CURVE('',#4180,#4183,#3567,.T.);
#5348=EDGE_CURVE('',#4184,#4184,#3568,.T.);
#5349=EDGE_CURVE('',#4185,#4185,#3569,.T.);
#5350=EDGE_CURVE('',#4169,#4171,#2463,.T.);
#5351=EDGE_CURVE('',#4178,#4168,#2464,.T.);
#5352=EDGE_CURVE('',#4186,#4187,#3570,.T.);
#5353=EDGE_CURVE('',#4188,#4186,#2465,.T.);
#5354=EDGE_CURVE('',#4171,#4188,#2466,.T.);
#5355=EDGE_CURVE('',#4189,#4172,#3571,.T.);
#5356=EDGE_CURVE('',#4189,#4190,#2467,.T.);
#5357=EDGE_CURVE('',#4191,#4190,#2468,.T.);
#5358=EDGE_CURVE('',#4192,#4191,#2469,.T.);
#5359=EDGE_CURVE('',#4193,#4192,#2470,.T.);
#5360=EDGE_CURVE('',#4187,#4193,#3572,.T.);
#5361=EDGE_CURVE('',#4194,#4194,#3573,.T.);
#5362=EDGE_CURVE('',#4194,#4177,#2471,.T.);
#5363=EDGE_CURVE('',#4173,#4195,#3574,.T.);
#5364=EDGE_CURVE('',#4196,#4176,#3575,.T.);
#5365=EDGE_CURVE('',#4196,#4195,#2472,.T.);
#5366=EDGE_CURVE('',#4175,#4197,#3576,.T.);
#5367=EDGE_CURVE('',#4197,#4196,#679,.T.);
#5368=EDGE_CURVE('',#4198,#4199,#3577,.T.);
#5369=EDGE_CURVE('',#4200,#4198,#2473,.T.);
#5370=EDGE_CURVE('',#4201,#4200,#2474,.T.);
#5371=EDGE_CURVE('',#4202,#4201,#2475,.T.);
#5372=EDGE_CURVE('',#4202,#4197,#2476,.T.);
#5373=EDGE_CURVE('',#4203,#4178,#2477,.T.);
#5374=EDGE_CURVE('',#4204,#4203,#2478,.T.);
#5375=EDGE_CURVE('',#4199,#4204,#3578,.T.);
#5376=EDGE_CURVE('',#4195,#4189,#680,.T.);
#5377=EDGE_CURVE('',#4194,#4185,#2479,.T.);
#5378=EDGE_CURVE('',#4205,#4206,#3579,.T.);
#5379=EDGE_CURVE('',#4206,#4205,#3580,.T.);
#5380=EDGE_CURVE('',#4205,#4184,#2480,.T.);
#5381=EDGE_CURVE('',#4134,#4135,#3581,.T.);
#5382=EDGE_CURVE('',#4135,#4183,#2481,.T.);
#5383=EDGE_CURVE('',#4180,#4182,#302,.T.);
#5384=EDGE_CURVE('',#4181,#4207,#2482,.T.);
#5385=EDGE_CURVE('',#4207,#4208,#2483,.T.);
#5386=EDGE_CURVE('',#4208,#4179,#2484,.T.);
#5387=EDGE_CURVE('',#4188,#4181,#2485,.T.);
#5388=EDGE_CURVE('',#4179,#4203,#2486,.T.);
#5389=EDGE_CURVE('',#4193,#4186,#303,.F.);
#5390=EDGE_CURVE('',#4192,#4209,#2487,.T.);
#5391=EDGE_CURVE('',#4209,#4207,#2488,.T.);
#5392=EDGE_CURVE('',#4207,#4188,#2489,.T.);
#5393=EDGE_CURVE('',#4191,#4210,#2490,.T.);
#5394=EDGE_CURVE('',#4210,#4211,#2491,.T.);
#5395=EDGE_CURVE('',#4211,#4192,#2492,.T.);
#5396=EDGE_CURVE('',#4190,#4212,#2493,.T.);
#5397=EDGE_CURVE('',#4212,#4213,#2494,.T.);
#5398=EDGE_CURVE('',#4213,#4191,#2495,.T.);
#5399=EDGE_CURVE('',#4214,#4202,#2496,.T.);
#5400=EDGE_CURVE('',#4212,#4214,#2497,.T.);
#5401=EDGE_CURVE('',#4116,#4163,#304,.T.);
#5402=EDGE_CURVE('',#4162,#4117,#305,.T.);
#5403=EDGE_CURVE('',#4215,#4215,#3582,.T.);
#5404=EDGE_CURVE('',#4215,#4187,#2498,.T.);
#5405=EDGE_CURVE('',#4204,#4198,#306,.F.);
#5406=EDGE_CURVE('',#4203,#4208,#2499,.T.);
#5407=EDGE_CURVE('',#4208,#4216,#2500,.T.);
#5408=EDGE_CURVE('',#4216,#4200,#2501,.T.);
#5409=EDGE_CURVE('',#4201,#4217,#2502,.T.);
#5410=EDGE_CURVE('',#4217,#4214,#2503,.T.);
#5411=EDGE_CURVE('',#4200,#4218,#2504,.T.);
#5412=EDGE_CURVE('',#4218,#4219,#2505,.T.);
#5413=EDGE_CURVE('',#4219,#4201,#2506,.T.);
#5414=EDGE_CURVE('',#4220,#4220,#3583,.T.);
#5415=EDGE_CURVE('',#4220,#4199,#2507,.T.);
#5416=EDGE_CURVE('',#4221,#4222,#307,.T.);
#5417=EDGE_CURVE('',#4222,#4223,#308,.T.);
#5418=EDGE_CURVE('',#4223,#4224,#309,.T.);
#5419=EDGE_CURVE('',#4224,#4225,#310,.T.);
#5420=EDGE_CURVE('',#4225,#4226,#311,.T.);
#5421=EDGE_CURVE('',#4226,#4227,#312,.T.);
#5422=EDGE_CURVE('',#4227,#4228,#313,.T.);
#5423=EDGE_CURVE('',#4228,#4229,#314,.T.);
#5424=EDGE_CURVE('',#4229,#4230,#315,.T.);
#5425=EDGE_CURVE('',#4230,#4231,#316,.T.);
#5426=EDGE_CURVE('',#4232,#4231,#3584,.T.);
#5427=EDGE_CURVE('',#4232,#4233,#317,.T.);
#5428=EDGE_CURVE('',#4233,#4234,#318,.T.);
#5429=EDGE_CURVE('',#4234,#4235,#319,.T.);
#5430=EDGE_CURVE('',#4235,#4236,#320,.T.);
#5431=EDGE_CURVE('',#4236,#4237,#321,.T.);
#5432=EDGE_CURVE('',#4237,#4238,#322,.T.);
#5433=EDGE_CURVE('',#4238,#4239,#323,.T.);
#5434=EDGE_CURVE('',#4239,#4240,#324,.T.);
#5435=EDGE_CURVE('',#4240,#4241,#325,.T.);
#5436=EDGE_CURVE('',#4241,#4242,#326,.T.);
#5437=EDGE_CURVE('',#4242,#4206,#327,.T.);
#5438=EDGE_CURVE('',#4205,#4221,#328,.T.);
#5439=EDGE_CURVE('',#4243,#4244,#3585,.T.);
#5440=EDGE_CURVE('',#4244,#4205,#329,.T.);
#5441=EDGE_CURVE('',#4206,#4243,#330,.T.);
#5442=EDGE_CURVE('',#4079,#4135,#331,.T.);
#5443=EDGE_CURVE('',#4134,#4080,#332,.T.);
#5444=EDGE_CURVE('',#4216,#4209,#2508,.T.);
#5445=EDGE_CURVE('',#4209,#4211,#2509,.T.);
#5446=EDGE_CURVE('',#4211,#4218,#2510,.T.);
#5447=EDGE_CURVE('',#4219,#4210,#2511,.T.);
#5448=EDGE_CURVE('',#4245,#4245,#3586,.T.);
#5449=EDGE_CURVE('',#4246,#4246,#3587,.T.);
#5450=EDGE_CURVE('',#4210,#4213,#2512,.T.);
#5451=EDGE_CURVE('',#4213,#4217,#2513,.T.);
#5452=EDGE_CURVE('',#4115,#4247,#333,.T.);
#5453=EDGE_CURVE('',#4247,#4112,#334,.T.);
#5454=EDGE_CURVE('',#4114,#4111,#335,.F.);
#5455=EDGE_CURVE('',#4084,#4139,#336,.T.);
#5456=EDGE_CURVE('',#4138,#4085,#337,.T.);
#5457=EDGE_CURVE('',#4220,#4215,#2514,.T.);
#5458=EDGE_CURVE('',#4248,#4249,#338,.T.);
#5459=EDGE_CURVE('',#4249,#4250,#339,.T.);
#5460=EDGE_CURVE('',#4250,#4251,#340,.T.);
#5461=EDGE_CURVE('',#4251,#4252,#341,.T.);
#5462=EDGE_CURVE('',#4252,#4060,#342,.T.);
#5463=EDGE_CURVE('',#4059,#4253,#343,.T.);
#5464=EDGE_CURVE('',#4253,#4254,#344,.T.);
#5465=EDGE_CURVE('',#4254,#4255,#345,.T.);
#5466=EDGE_CURVE('',#4255,#4256,#705,.T.);
#5467=EDGE_CURVE('',#4256,#4257,#346,.T.);
#5468=EDGE_CURVE('',#4257,#4258,#2515,.T.);
#5469=EDGE_CURVE('',#4258,#4259,#347,.T.);
#5470=EDGE_CURVE('',#4259,#4260,#706,.T.);
#5471=EDGE_CURVE('',#4260,#4261,#348,.T.);
#5472=EDGE_CURVE('',#4261,#4262,#349,.T.);
#5473=EDGE_CURVE('',#4262,#4121,#350,.T.);
#5474=EDGE_CURVE('',#4120,#4263,#351,.T.);
#5475=EDGE_CURVE('',#4263,#4264,#707,.T.);
#5476=EDGE_CURVE('',#4264,#4265,#352,.T.);
#5477=EDGE_CURVE('',#4265,#4266,#353,.T.);
#5478=EDGE_CURVE('',#4266,#4267,#354,.T.);
#5479=EDGE_CURVE('',#4267,#4268,#2516,.T.);
#5480=EDGE_CURVE('',#4268,#4248,#708,.T.);
#5481=EDGE_CURVE('',#4218,#4216,#2517,.T.);
#5482=EDGE_CURVE('',#4217,#4219,#2518,.T.);
#5483=EDGE_CURVE('',#4231,#4269,#355,.T.);
#5484=EDGE_CURVE('',#4244,#4270,#356,.F.);
#5485=EDGE_CURVE('',#4270,#4271,#357,.F.);
#5486=EDGE_CURVE('',#4271,#4272,#358,.F.);
#5487=EDGE_CURVE('',#4272,#4273,#359,.F.);
#5488=EDGE_CURVE('',#4273,#4274,#360,.F.);
#5489=EDGE_CURVE('',#4274,#4275,#361,.F.);
#5490=EDGE_CURVE('',#4275,#4276,#362,.F.);
#5491=EDGE_CURVE('',#4276,#4277,#363,.F.);
#5492=EDGE_CURVE('',#4277,#4278,#364,.F.);
#5493=EDGE_CURVE('',#4278,#4279,#365,.F.);
#5494=EDGE_CURVE('',#4279,#4269,#366,.F.);
#5495=EDGE_CURVE('',#4280,#4232,#367,.T.);
#5496=EDGE_CURVE('',#4281,#4280,#368,.T.);
#5497=EDGE_CURVE('',#4282,#4281,#369,.T.);
#5498=EDGE_CURVE('',#4283,#4282,#370,.F.);
#5499=EDGE_CURVE('',#4284,#4283,#371,.F.);
#5500=EDGE_CURVE('',#4243,#4284,#372,.T.);
#5501=EDGE_CURVE('',#4231,#4285,#3588,.T.);
#5502=EDGE_CURVE('',#4285,#4245,#2519,.T.);
#5503=EDGE_CURVE('',#4285,#4232,#3589,.T.);
#5504=EDGE_CURVE('',#4269,#4280,#3590,.T.);
#5505=EDGE_CURVE('',#4252,#4263,#373,.F.);
#5506=EDGE_CURVE('',#4077,#4074,#374,.T.);
#5507=EDGE_CURVE('',#4286,#4075,#375,.T.);
#5508=EDGE_CURVE('',#4078,#4286,#376,.T.);
#5509=EDGE_CURVE('',#4253,#4262,#377,.T.);
#5510=EDGE_CURVE('',#4138,#4287,#3591,.T.);
#5511=EDGE_CURVE('',#4287,#4246,#2520,.T.);
#5512=EDGE_CURVE('',#4287,#4139,#3592,.T.);
#5513=EDGE_CURVE('',#4288,#4268,#3593,.T.);
#5514=EDGE_CURVE('',#4248,#4288,#378,.F.);
#5515=EDGE_CURVE('',#4267,#4288,#709,.T.);
#5516=EDGE_CURVE('',#4249,#4266,#379,.T.);
#5517=EDGE_CURVE('',#4265,#4250,#380,.T.);
#5518=EDGE_CURVE('',#4251,#4264,#381,.T.);
#5519=EDGE_CURVE('',#4261,#4254,#382,.T.);
#5520=EDGE_CURVE('',#4260,#4255,#383,.F.);
#5521=EDGE_CURVE('',#4259,#4256,#384,.T.);
#5522=EDGE_CURVE('',#4257,#4258,#385,.T.);
#5523=EDGE_CURVE('',#4289,#4289,#3594,.T.);
#5524=EDGE_CURVE('',#4289,#4290,#2521,.T.);
#5525=EDGE_CURVE('',#4290,#4291,#3595,.T.);
#5526=EDGE_CURVE('',#4291,#4290,#3596,.T.);
#5527=EDGE_CURVE('',#4291,#4292,#3597,.T.);
#5528=EDGE_CURVE('',#4292,#4293,#3598,.T.);
#5529=EDGE_CURVE('',#4293,#4292,#3599,.T.);
#5530=EDGE_CURVE('',#4293,#4294,#2522,.T.);
#5531=EDGE_CURVE('',#4294,#4294,#3600,.T.);
#5532=EDGE_CURVE('',#4295,#4296,#386,.T.);
#5533=EDGE_CURVE('',#4296,#4297,#387,.T.);
#5534=EDGE_CURVE('',#4297,#4298,#388,.T.);
#5535=EDGE_CURVE('',#4298,#4299,#389,.T.);
#5536=EDGE_CURVE('',#4299,#4300,#390,.T.);
#5537=EDGE_CURVE('',#4300,#4301,#391,.T.);
#5538=EDGE_CURVE('',#4301,#4302,#392,.T.);
#5539=EDGE_CURVE('',#4302,#4303,#393,.T.);
#5540=EDGE_CURVE('',#4303,#4304,#394,.T.);
#5541=EDGE_CURVE('',#4304,#4305,#3601,.T.);
#5542=EDGE_CURVE('',#4306,#4305,#3602,.T.);
#5543=EDGE_CURVE('',#4307,#4306,#395,.F.);
#5544=EDGE_CURVE('',#4308,#4307,#396,.F.);
#5545=EDGE_CURVE('',#4309,#4308,#397,.F.);
#5546=EDGE_CURVE('',#4310,#4309,#398,.F.);
#5547=EDGE_CURVE('',#4311,#4310,#399,.F.);
#5548=EDGE_CURVE('',#4312,#4311,#400,.F.);
#5549=EDGE_CURVE('',#4313,#4312,#401,.F.);
#5550=EDGE_CURVE('',#4314,#4313,#402,.F.);
#5551=EDGE_CURVE('',#4315,#4314,#403,.F.);
#5552=EDGE_CURVE('',#4316,#4315,#404,.F.);
#5553=EDGE_CURVE('',#4317,#4316,#405,.F.);
#5554=EDGE_CURVE('',#4318,#4317,#3603,.T.);
#5555=EDGE_CURVE('',#4318,#4295,#406,.T.);
#5556=EDGE_CURVE('',#4319,#4320,#407,.T.);
#5557=EDGE_CURVE('',#4320,#4321,#408,.T.);
#5558=EDGE_CURVE('',#4321,#4322,#409,.T.);
#5559=EDGE_CURVE('',#4322,#4323,#410,.T.);
#5560=EDGE_CURVE('',#4323,#4324,#3604,.T.);
#5561=EDGE_CURVE('',#4324,#4325,#411,.T.);
#5562=EDGE_CURVE('',#4325,#4326,#412,.T.);
#5563=EDGE_CURVE('',#4326,#4327,#413,.T.);
#5564=EDGE_CURVE('',#4327,#4328,#414,.T.);
#5565=EDGE_CURVE('',#4328,#4329,#415,.T.);
#5566=EDGE_CURVE('',#4329,#4330,#416,.T.);
#5567=EDGE_CURVE('',#4330,#4331,#417,.T.);
#5568=EDGE_CURVE('',#4331,#4332,#418,.T.);
#5569=EDGE_CURVE('',#4332,#4333,#419,.T.);
#5570=EDGE_CURVE('',#4333,#4334,#420,.T.);
#5571=EDGE_CURVE('',#4334,#4335,#421,.T.);
#5572=EDGE_CURVE('',#4336,#4335,#3605,.T.);
#5573=EDGE_CURVE('',#4336,#4337,#422,.T.);
#5574=EDGE_CURVE('',#4337,#4319,#423,.T.);
#5575=EDGE_CURVE('',#4319,#4338,#424,.T.);
#5576=EDGE_CURVE('',#4339,#4340,#425,.T.);
#5577=EDGE_CURVE('',#4340,#4341,#426,.T.);
#5578=EDGE_CURVE('',#4341,#4342,#427,.T.);
#5579=EDGE_CURVE('',#4342,#4343,#428,.T.);
#5580=EDGE_CURVE('',#4343,#4344,#3606,.T.);
#5581=EDGE_CURVE('',#4345,#4344,#3607,.T.);
#5582=EDGE_CURVE('',#4346,#4345,#429,.F.);
#5583=EDGE_CURVE('',#4347,#4346,#430,.F.);
#5584=EDGE_CURVE('',#4348,#4347,#431,.F.);
#5585=EDGE_CURVE('',#4349,#4348,#432,.F.);
#5586=EDGE_CURVE('',#4350,#4349,#433,.F.);
#5587=EDGE_CURVE('',#4351,#4350,#434,.F.);
#5588=EDGE_CURVE('',#4352,#4351,#3608,.T.);
#5589=EDGE_CURVE('',#4352,#4339,#435,.T.);
#5590=EDGE_CURVE('',#4353,#4354,#436,.T.);
#5591=EDGE_CURVE('',#4354,#4355,#437,.T.);
#5592=EDGE_CURVE('',#4355,#4356,#438,.T.);
#5593=EDGE_CURVE('',#4357,#4356,#3609,.T.);
#5594=EDGE_CURVE('',#4357,#4358,#439,.T.);
#5595=EDGE_CURVE('',#4358,#4359,#440,.T.);
#5596=EDGE_CURVE('',#4359,#4360,#441,.T.);
#5597=EDGE_CURVE('',#4360,#4361,#442,.T.);
#5598=EDGE_CURVE('',#4361,#4362,#443,.T.);
#5599=EDGE_CURVE('',#4362,#4363,#444,.T.);
#5600=EDGE_CURVE('',#4364,#4363,#3610,.T.);
#5601=EDGE_CURVE('',#4364,#4365,#445,.T.);
#5602=EDGE_CURVE('',#4365,#4366,#446,.T.);
#5603=EDGE_CURVE('',#4366,#4353,#447,.T.);
#5604=EDGE_CURVE('',#4367,#4367,#3611,.T.);
#5605=EDGE_CURVE('',#4367,#4368,#2523,.T.);
#5606=EDGE_CURVE('',#4368,#4368,#3612,.T.);
#5607=EDGE_CURVE('',#4369,#4369,#3613,.T.);
#5608=EDGE_CURVE('',#4369,#4367,#2524,.T.);
#5609=EDGE_CURVE('',#4370,#4370,#3614,.T.);
#5610=EDGE_CURVE('',#4371,#4371,#3615,.T.);
#5611=EDGE_CURVE('',#4371,#4372,#2525,.T.);
#5612=EDGE_CURVE('',#4372,#4372,#3616,.T.);
#5613=EDGE_CURVE('',#4373,#4373,#3617,.T.);
#5614=EDGE_CURVE('',#4371,#4374,#2526,.T.);
#5615=EDGE_CURVE('',#4374,#4374,#3618,.T.);
#5616=EDGE_CURVE('',#4369,#4374,#2527,.T.);
#5617=EDGE_CURVE('',#4375,#4375,#3619,.T.);
#5618=EDGE_CURVE('',#4375,#4373,#2528,.T.);
#5619=EDGE_CURVE('',#4375,#4376,#2529,.T.);
#5620=EDGE_CURVE('',#4376,#4376,#3620,.T.);
#5621=EDGE_CURVE('',#4377,#4378,#3621,.T.);
#5622=EDGE_CURVE('',#4377,#4306,#448,.T.);
#5623=EDGE_CURVE('',#4305,#4336,#449,.T.);
#5624=EDGE_CURVE('',#4378,#4336,#3622,.T.);
#5625=EDGE_CURVE('',#4335,#4377,#450,.T.);
#5626=EDGE_CURVE('',#4317,#4324,#451,.T.);
#5627=EDGE_CURVE('',#4323,#4318,#452,.T.);
#5628=EDGE_CURVE('',#4378,#4379,#2530,.T.);
#5629=EDGE_CURVE('',#4379,#4379,#3623,.T.);
#5630=EDGE_CURVE('',#4356,#4345,#453,.T.);
#5631=EDGE_CURVE('',#4351,#4364,#454,.T.);
#5632=EDGE_CURVE('',#4363,#4380,#3624,.T.);
#5633=EDGE_CURVE('',#4363,#4352,#455,.T.);
#5634=EDGE_CURVE('',#4380,#4364,#3625,.T.);
#5635=EDGE_CURVE('',#4344,#4357,#456,.T.);
#5636=EDGE_CURVE('',#4381,#4381,#3626,.T.);
#5637=EDGE_CURVE('',#4380,#4370,#2531,.T.);
#5638=EDGE_CURVE('',#4382,#4382,#3627,.T.);
#5639=EDGE_CURVE('',#4382,#4381,#2532,.T.);
#5640=EDGE_CURVE('',#4383,#4383,#3628,.T.);
#5641=EDGE_CURVE('',#4383,#4384,#2533,.T.);
#5642=EDGE_CURVE('',#4384,#4384,#3629,.T.);
#5643=EDGE_CURVE('',#4385,#4385,#3630,.T.);
#5644=EDGE_CURVE('',#4385,#4383,#2534,.T.);
#5645=EDGE_CURVE('',#4385,#4386,#2535,.T.);
#5646=EDGE_CURVE('',#4386,#4386,#3631,.T.);
#5647=EDGE_CURVE('',#4387,#4388,#2536,.T.);
#5648=EDGE_CURVE('',#4387,#4389,#457,.T.);
#5649=EDGE_CURVE('',#4390,#4389,#3632,.T.);
#5650=EDGE_CURVE('',#4390,#4388,#458,.T.);
#5651=EDGE_CURVE('',#4391,#4392,#2537,.T.);
#5652=EDGE_CURVE('',#4391,#4393,#459,.T.);
#5653=EDGE_CURVE('',#4393,#4387,#460,.T.);
#5654=EDGE_CURVE('',#4388,#4392,#461,.T.);
#5655=EDGE_CURVE('',#4394,#4395,#2538,.T.);
#5656=EDGE_CURVE('',#4394,#4391,#462,.T.);
#5657=EDGE_CURVE('',#4392,#4395,#463,.T.);
#5658=EDGE_CURVE('',#4396,#4397,#2539,.T.);
#5659=EDGE_CURVE('',#4396,#4394,#464,.T.);
#5660=EDGE_CURVE('',#4395,#4397,#465,.T.);
#5661=EDGE_CURVE('',#4398,#4399,#2540,.T.);
#5662=EDGE_CURVE('',#4398,#4396,#466,.T.);
#5663=EDGE_CURVE('',#4397,#4399,#467,.T.);
#5664=EDGE_CURVE('',#4400,#4400,#468,.F.);
#5665=EDGE_CURVE('',#4400,#4401,#2541,.T.);
#5666=EDGE_CURVE('',#4401,#4402,#3633,.T.);
#5667=EDGE_CURVE('',#4402,#4403,#469,.T.);
#5668=EDGE_CURVE('',#4403,#4404,#2542,.T.);
#5669=EDGE_CURVE('',#4404,#4405,#470,.T.);
#5670=EDGE_CURVE('',#4405,#4401,#3634,.T.);
#5671=EDGE_CURVE('',#4406,#4407,#471,.T.);
#5672=EDGE_CURVE('',#4406,#4408,#3635,.T.);
#5673=EDGE_CURVE('',#4408,#4409,#472,.T.);
#5674=EDGE_CURVE('',#4409,#4407,#473,.F.);
#5675=EDGE_CURVE('',#4403,#4398,#474,.T.);
#5676=EDGE_CURVE('',#4399,#4404,#475,.T.);
#5677=EDGE_CURVE('',#4410,#4411,#476,.T.);
#5678=EDGE_CURVE('',#4411,#4412,#477,.T.);
#5679=EDGE_CURVE('',#4413,#4412,#3636,.T.);
#5680=EDGE_CURVE('',#4414,#4413,#478,.F.);
#5681=EDGE_CURVE('',#4415,#4414,#479,.F.);
#5682=EDGE_CURVE('',#4416,#4415,#480,.F.);
#5683=EDGE_CURVE('',#4417,#4416,#481,.F.);
#5684=EDGE_CURVE('',#4418,#4417,#482,.F.);
#5685=EDGE_CURVE('',#4419,#4418,#483,.F.);
#5686=EDGE_CURVE('',#4420,#4419,#3637,.T.);
#5687=EDGE_CURVE('',#4420,#4421,#484,.T.);
#5688=EDGE_CURVE('',#4421,#4410,#485,.T.);
#5689=EDGE_CURVE('',#4407,#4409,#486,.F.);
#5690=EDGE_CURVE('',#4408,#4406,#3638,.T.);
#5691=EDGE_CURVE('',#4422,#4423,#2543,.T.);
#5692=EDGE_CURVE('',#4422,#4424,#2544,.T.);
#5693=EDGE_CURVE('',#4425,#4424,#2545,.T.);
#5694=EDGE_CURVE('',#4425,#4426,#2546,.T.);
#5695=EDGE_CURVE('',#4427,#4426,#2547,.T.);
#5696=EDGE_CURVE('',#4427,#4428,#2548,.T.);
#5697=EDGE_CURVE('',#4429,#4428,#2549,.T.);
#5698=EDGE_CURVE('',#4429,#4430,#2550,.T.);
#5699=EDGE_CURVE('',#4431,#4430,#2551,.T.);
#5700=EDGE_CURVE('',#4431,#4432,#2552,.T.);
#5701=EDGE_CURVE('',#4433,#4432,#2553,.T.);
#5702=EDGE_CURVE('',#4433,#4423,#2554,.T.);
#5703=EDGE_CURVE('',#4407,#4434,#2555,.T.);
#5704=EDGE_CURVE('',#4434,#4434,#3639,.T.);
#5705=EDGE_CURVE('',#4423,#4435,#2556,.T.);
#5706=EDGE_CURVE('',#4435,#4436,#2557,.T.);
#5707=EDGE_CURVE('',#4436,#4422,#2558,.T.);
#5708=EDGE_CURVE('',#4437,#4433,#2559,.T.);
#5709=EDGE_CURVE('',#4438,#4437,#2560,.T.);
#5710=EDGE_CURVE('',#4439,#4438,#2561,.T.);
#5711=EDGE_CURVE('',#4439,#4440,#2562,.T.);
#5712=EDGE_CURVE('',#4441,#4440,#2563,.T.);
#5713=EDGE_CURVE('',#4435,#4441,#2564,.T.);
#5714=EDGE_CURVE('',#4442,#4442,#3640,.T.);
#5715=EDGE_CURVE('',#4424,#4443,#2565,.T.);
#5716=EDGE_CURVE('',#4443,#4444,#2566,.T.);
#5717=EDGE_CURVE('',#4444,#4425,#2567,.T.);
#5718=EDGE_CURVE('',#4445,#4444,#2568,.T.);
#5719=EDGE_CURVE('',#4446,#4445,#2569,.T.);
#5720=EDGE_CURVE('',#4446,#4447,#2570,.T.);
#5721=EDGE_CURVE('',#4448,#4447,#2571,.T.);
#5722=EDGE_CURVE('',#4449,#4448,#2572,.T.);
#5723=EDGE_CURVE('',#4426,#4449,#2573,.T.);
#5724=EDGE_CURVE('',#4450,#4450,#3641,.T.);
#5725=EDGE_CURVE('',#4449,#4451,#2574,.T.);
#5726=EDGE_CURVE('',#4451,#4427,#2575,.T.);
#5727=EDGE_CURVE('',#4428,#4452,#2576,.T.);
#5728=EDGE_CURVE('',#4452,#4453,#2577,.T.);
#5729=EDGE_CURVE('',#4453,#4429,#2578,.T.);
#5730=EDGE_CURVE('',#4454,#4453,#2579,.T.);
#5731=EDGE_CURVE('',#4455,#4454,#2580,.T.);
#5732=EDGE_CURVE('',#4455,#4456,#2581,.T.);
#5733=EDGE_CURVE('',#4457,#4456,#2582,.T.);
#5734=EDGE_CURVE('',#4458,#4457,#2583,.T.);
#5735=EDGE_CURVE('',#4430,#4458,#2584,.T.);
#5736=EDGE_CURVE('',#4458,#4459,#2585,.T.);
#5737=EDGE_CURVE('',#4459,#4431,#2586,.T.);
#5738=EDGE_CURVE('',#4432,#4460,#2587,.T.);
#5739=EDGE_CURVE('',#4460,#4437,#2588,.T.);
#5740=EDGE_CURVE('',#4438,#4461,#2589,.T.);
#5741=EDGE_CURVE('',#4461,#4462,#2590,.T.);
#5742=EDGE_CURVE('',#4462,#4439,#2591,.T.);
#5743=EDGE_CURVE('',#4463,#4462,#2592,.T.);
#5744=EDGE_CURVE('',#4456,#4463,#2593,.T.);
#5745=EDGE_CURVE('',#4464,#4455,#2594,.T.);
#5746=EDGE_CURVE('',#4465,#4464,#2595,.T.);
#5747=EDGE_CURVE('',#4447,#4465,#2596,.T.);
#5748=EDGE_CURVE('',#4466,#4446,#2597,.T.);
#5749=EDGE_CURVE('',#4467,#4466,#2598,.T.);
#5750=EDGE_CURVE('',#4440,#4467,#2599,.T.);
#5751=EDGE_CURVE('',#4468,#4468,#3642,.T.);
#5752=EDGE_CURVE('',#4463,#4469,#2600,.T.);
#5753=EDGE_CURVE('',#4469,#4457,#2601,.T.);
#5754=EDGE_CURVE('',#4454,#4470,#2602,.T.);
#5755=EDGE_CURVE('',#4470,#4464,#2603,.T.);
#5756=EDGE_CURVE('',#4465,#4471,#2604,.T.);
#5757=EDGE_CURVE('',#4471,#4448,#2605,.T.);
#5758=EDGE_CURVE('',#4445,#4472,#2606,.T.);
#5759=EDGE_CURVE('',#4472,#4466,#2607,.T.);
#5760=EDGE_CURVE('',#4473,#4436,#2608,.T.);
#5761=EDGE_CURVE('',#4467,#4473,#2609,.T.);
#5762=EDGE_CURVE('',#4443,#4472,#2610,.T.);
#5763=EDGE_CURVE('',#4474,#4474,#3643,.T.);
#5764=EDGE_CURVE('',#4471,#4451,#2611,.T.);
#5765=EDGE_CURVE('',#4452,#4470,#2612,.T.);
#5766=EDGE_CURVE('',#4469,#4459,#2613,.T.);
#5767=EDGE_CURVE('',#4460,#4461,#2614,.T.);
#5768=EDGE_CURVE('',#4473,#4441,#2615,.T.);
#5769=EDGE_CURVE('',#4400,#4468,#487,.T.);
#5770=EDGE_CURVE('',#4475,#4450,#2616,.T.);
#5771=EDGE_CURVE('',#4476,#4474,#2617,.T.);
#5772=EDGE_CURVE('',#4477,#4442,#2618,.T.);
#5773=EDGE_CURVE('',#4478,#4478,#3644,.T.);
#5774=EDGE_CURVE('',#4478,#4479,#2619,.T.);
#5775=EDGE_CURVE('',#4480,#4479,#3645,.T.);
#5776=EDGE_CURVE('',#4479,#4480,#3646,.T.);
#5777=EDGE_CURVE('',#4481,#4481,#3647,.T.);
#5778=EDGE_CURVE('',#4481,#4478,#2620,.T.);
#5779=EDGE_CURVE('',#4482,#4482,#3648,.T.);
#5780=EDGE_CURVE('',#4482,#4483,#2621,.T.);
#5781=EDGE_CURVE('',#4483,#4483,#3649,.T.);
#5782=EDGE_CURVE('',#4484,#4484,#3650,.T.);
#5783=EDGE_CURVE('',#4482,#4480,#2622,.T.);
#5784=EDGE_CURVE('',#4485,#4486,#3651,.T.);
#5785=EDGE_CURVE('',#4486,#4484,#2623,.T.);
#5786=EDGE_CURVE('',#4486,#4390,#3652,.T.);
#5787=EDGE_CURVE('',#4389,#4485,#488,.T.);
#5788=EDGE_CURVE('',#4405,#4413,#489,.T.);
#5789=EDGE_CURVE('',#4412,#4402,#490,.T.);
#5790=EDGE_CURVE('',#4419,#4390,#491,.T.);
#5791=EDGE_CURVE('',#4485,#4420,#492,.T.);
#5792=EDGE_CURVE('',#4487,#4488,#493,.T.);
#5793=EDGE_CURVE('',#4487,#4489,#494,.T.);
#5794=EDGE_CURVE('',#4489,#4490,#3653,.T.);
#5795=EDGE_CURVE('',#4488,#4490,#3654,.T.);
#5796=EDGE_CURVE('',#4487,#4491,#495,.T.);
#5797=EDGE_CURVE('',#4492,#4491,#3655,.T.);
#5798=EDGE_CURVE('',#4492,#4489,#3656,.T.);
#5799=EDGE_CURVE('',#4487,#4493,#496,.T.);
#5800=EDGE_CURVE('',#4493,#4494,#3657,.T.);
#5801=EDGE_CURVE('',#4491,#4494,#3658,.T.);
#5802=EDGE_CURVE('',#4487,#4495,#497,.T.);
#5803=EDGE_CURVE('',#4496,#4495,#3659,.T.);
#5804=EDGE_CURVE('',#4496,#4493,#3660,.T.);
#5805=EDGE_CURVE('',#4487,#4497,#498,.T.);
#5806=EDGE_CURVE('',#4497,#4498,#3661,.T.);
#5807=EDGE_CURVE('',#4495,#4498,#3662,.T.);
#5808=EDGE_CURVE('',#4499,#4500,#499,.T.);
#5809=EDGE_CURVE('',#4499,#4501,#500,.T.);
#5810=EDGE_CURVE('',#4501,#4502,#3663,.T.);
#5811=EDGE_CURVE('',#4500,#4502,#3664,.T.);
#5812=EDGE_CURVE('',#4499,#4503,#501,.T.);
#5813=EDGE_CURVE('',#4504,#4503,#3665,.T.);
#5814=EDGE_CURVE('',#4504,#4501,#3666,.T.);
#5815=EDGE_CURVE('',#4499,#4505,#502,.T.);
#5816=EDGE_CURVE('',#4505,#4506,#3667,.T.);
#5817=EDGE_CURVE('',#4503,#4506,#3668,.T.);
#5818=EDGE_CURVE('',#4499,#4507,#503,.T.);
#5819=EDGE_CURVE('',#4508,#4507,#3669,.T.);
#5820=EDGE_CURVE('',#4508,#4505,#3670,.T.);
#5821=EDGE_CURVE('',#4499,#4509,#504,.T.);
#5822=EDGE_CURVE('',#4509,#4510,#3671,.T.);
#5823=EDGE_CURVE('',#4507,#4510,#3672,.T.);
#5824=EDGE_CURVE('',#4511,#4512,#505,.T.);
#5825=EDGE_CURVE('',#4511,#4513,#506,.T.);
#5826=EDGE_CURVE('',#4513,#4514,#3673,.T.);
#5827=EDGE_CURVE('',#4512,#4514,#3674,.T.);
#5828=EDGE_CURVE('',#4511,#4515,#507,.T.);
#5829=EDGE_CURVE('',#4516,#4515,#3675,.T.);
#5830=EDGE_CURVE('',#4516,#4513,#3676,.T.);
#5831=EDGE_CURVE('',#4511,#4517,#508,.T.);
#5832=EDGE_CURVE('',#4517,#4518,#3677,.T.);
#5833=EDGE_CURVE('',#4515,#4518,#3678,.T.);
#5834=EDGE_CURVE('',#4511,#4519,#509,.T.);
#5835=EDGE_CURVE('',#4520,#4519,#3679,.T.);
#5836=EDGE_CURVE('',#4520,#4517,#3680,.T.);
#5837=EDGE_CURVE('',#4511,#4521,#510,.T.);
#5838=EDGE_CURVE('',#4521,#4522,#3681,.T.);
#5839=EDGE_CURVE('',#4519,#4522,#3682,.T.);
#5840=EDGE_CURVE('',#4523,#4524,#511,.T.);
#5841=EDGE_CURVE('',#4523,#4525,#512,.T.);
#5842=EDGE_CURVE('',#4525,#4526,#3683,.T.);
#5843=EDGE_CURVE('',#4524,#4526,#3684,.T.);
#5844=EDGE_CURVE('',#4523,#4527,#513,.T.);
#5845=EDGE_CURVE('',#4528,#4527,#3685,.T.);
#5846=EDGE_CURVE('',#4528,#4525,#3686,.T.);
#5847=EDGE_CURVE('',#4523,#4529,#514,.T.);
#5848=EDGE_CURVE('',#4529,#4530,#3687,.T.);
#5849=EDGE_CURVE('',#4527,#4530,#3688,.T.);
#5850=EDGE_CURVE('',#4523,#4531,#515,.T.);
#5851=EDGE_CURVE('',#4532,#4531,#3689,.T.);
#5852=EDGE_CURVE('',#4532,#4529,#3690,.T.);
#5853=EDGE_CURVE('',#4523,#4533,#516,.T.);
#5854=EDGE_CURVE('',#4533,#4534,#3691,.T.);
#5855=EDGE_CURVE('',#4531,#4534,#3692,.T.);
#5856=EDGE_CURVE('',#4535,#4524,#3693,.T.);
#5857=EDGE_CURVE('',#4535,#4533,#3694,.T.);
#5858=EDGE_CURVE('',#4536,#4537,#3695,.T.);
#5859=EDGE_CURVE('',#4537,#4535,#2624,.T.);
#5860=EDGE_CURVE('',#4526,#4536,#2625,.T.);
#5861=EDGE_CURVE('',#4538,#4512,#3696,.T.);
#5862=EDGE_CURVE('',#4538,#4521,#3697,.T.);
#5863=EDGE_CURVE('',#4539,#4540,#3698,.T.);
#5864=EDGE_CURVE('',#4540,#4538,#2626,.T.);
#5865=EDGE_CURVE('',#4514,#4539,#2627,.T.);
#5866=EDGE_CURVE('',#4530,#4520,#2628,.T.);
#5867=EDGE_CURVE('',#4522,#4528,#2629,.T.);
#5868=EDGE_CURVE('',#4541,#4500,#3699,.T.);
#5869=EDGE_CURVE('',#4541,#4509,#3700,.T.);
#5870=EDGE_CURVE('',#4542,#4543,#3701,.T.);
#5871=EDGE_CURVE('',#4543,#4504,#2630,.T.);
#5872=EDGE_CURVE('',#4506,#4542,#2631,.T.);
#5873=EDGE_CURVE('',#4544,#4488,#3702,.T.);
#5874=EDGE_CURVE('',#4544,#4497,#3703,.T.);
#5875=EDGE_CURVE('',#4545,#4546,#3704,.T.);
#5876=EDGE_CURVE('',#4546,#4496,#2632,.T.);
#5877=EDGE_CURVE('',#4498,#4545,#2633,.T.);
#5878=EDGE_CURVE('',#4518,#4492,#2634,.T.);
#5879=EDGE_CURVE('',#4494,#4516,#2635,.T.);
#5880=EDGE_CURVE('',#4490,#4541,#2636,.T.);
#5881=EDGE_CURVE('',#4502,#4544,#2637,.T.);
#5882=EDGE_CURVE('',#4510,#4532,#2638,.T.);
#5883=EDGE_CURVE('',#4534,#4508,#2639,.T.);
#5884=EDGE_CURVE('',#4547,#4540,#2640,.T.);
#5885=EDGE_CURVE('',#4547,#4548,#2641,.T.);
#5886=EDGE_CURVE('',#4548,#4549,#3705,.T.);
#5887=EDGE_CURVE('',#4549,#4550,#2642,.T.);
#5888=EDGE_CURVE('',#4551,#4550,#2643,.T.);
#5889=EDGE_CURVE('',#4552,#4551,#2644,.T.);
#5890=EDGE_CURVE('',#4552,#4553,#3706,.T.);
#5891=EDGE_CURVE('',#4553,#4554,#2645,.T.);
#5892=EDGE_CURVE('',#4554,#4536,#2646,.T.);
#5893=EDGE_CURVE('',#4555,#4539,#2647,.T.);
#5894=EDGE_CURVE('',#4555,#4556,#2648,.T.);
#5895=EDGE_CURVE('',#4557,#4556,#2649,.T.);
#5896=EDGE_CURVE('',#4557,#4558,#2650,.T.);
#5897=EDGE_CURVE('',#4558,#4547,#2651,.T.);
#5898=EDGE_CURVE('',#4546,#4559,#2652,.T.);
#5899=EDGE_CURVE('',#4559,#4560,#2653,.T.);
#5900=EDGE_CURVE('',#4561,#4560,#2654,.T.);
#5901=EDGE_CURVE('',#4562,#4561,#2655,.T.);
#5902=EDGE_CURVE('',#4562,#4563,#2656,.T.);
#5903=EDGE_CURVE('',#4563,#4564,#2657,.T.);
#5904=EDGE_CURVE('',#4565,#4564,#2658,.T.);
#5905=EDGE_CURVE('',#4555,#4565,#2659,.T.);
#5906=EDGE_CURVE('',#4566,#4545,#2660,.T.);
#5907=EDGE_CURVE('',#4567,#4566,#2661,.T.);
#5908=EDGE_CURVE('',#4568,#4567,#2662,.T.);
#5909=EDGE_CURVE('',#4569,#4568,#2663,.T.);
#5910=EDGE_CURVE('',#4569,#4559,#2664,.T.);
#5911=EDGE_CURVE('',#4570,#4570,#3707,.T.);
#5912=EDGE_CURVE('',#4571,#4571,#3708,.T.);
#5913=EDGE_CURVE('',#4572,#4573,#3709,.T.);
#5914=EDGE_CURVE('',#4573,#4574,#2665,.T.);
#5915=EDGE_CURVE('',#4574,#4575,#3710,.T.);
#5916=EDGE_CURVE('',#4575,#4572,#2666,.T.);
#5917=EDGE_CURVE('',#4573,#4561,#2667,.T.);
#5918=EDGE_CURVE('',#4560,#4574,#2668,.T.);
#5919=EDGE_CURVE('',#4576,#4572,#2669,.T.);
#5920=EDGE_CURVE('',#4576,#4577,#2670,.T.);
#5921=EDGE_CURVE('',#4562,#4577,#2671,.T.);
#5922=EDGE_CURVE('',#4578,#4579,#3711,.T.);
#5923=EDGE_CURVE('',#4579,#4580,#2672,.T.);
#5924=EDGE_CURVE('',#4580,#4581,#3712,.T.);
#5925=EDGE_CURVE('',#4581,#4578,#2673,.T.);
#5926=EDGE_CURVE('',#4579,#4565,#2674,.T.);
#5927=EDGE_CURVE('',#4564,#4580,#2675,.T.);
#5928=EDGE_CURVE('',#4582,#4578,#2676,.T.);
#5929=EDGE_CURVE('',#4556,#4582,#2677,.T.);
#5930=EDGE_CURVE('',#4583,#4584,#3713,.T.);
#5931=EDGE_CURVE('',#4584,#4585,#2678,.T.);
#5932=EDGE_CURVE('',#4585,#4586,#3714,.T.);
#5933=EDGE_CURVE('',#4586,#4583,#2679,.T.);
#5934=EDGE_CURVE('',#4550,#4585,#2680,.T.);
#5935=EDGE_CURVE('',#4587,#4549,#2681,.T.);
#5936=EDGE_CURVE('',#4587,#4588,#2682,.T.);
#5937=EDGE_CURVE('',#4588,#4589,#2683,.T.);
#5938=EDGE_CURVE('',#4589,#4586,#2684,.T.);
#5939=EDGE_CURVE('',#4584,#4551,#2685,.T.);
#5940=EDGE_CURVE('',#4590,#4591,#3715,.T.);
#5941=EDGE_CURVE('',#4591,#4592,#2686,.T.);
#5942=EDGE_CURVE('',#4592,#4593,#3716,.T.);
#5943=EDGE_CURVE('',#4593,#4590,#2687,.T.);
#5944=EDGE_CURVE('',#4594,#4592,#2688,.T.);
#5945=EDGE_CURVE('',#4595,#4594,#2689,.T.);
#5946=EDGE_CURVE('',#4596,#4595,#2690,.T.);
#5947=EDGE_CURVE('',#4596,#4597,#2691,.T.);
#5948=EDGE_CURVE('',#4598,#4597,#2692,.T.);
#5949=EDGE_CURVE('',#4598,#4593,#2693,.T.);
#5950=EDGE_CURVE('',#4591,#4599,#2694,.T.);
#5951=EDGE_CURVE('',#4599,#4594,#2695,.T.);
#5952=EDGE_CURVE('',#4600,#4601,#3717,.T.);
#5953=EDGE_CURVE('',#4601,#4602,#2696,.T.);
#5954=EDGE_CURVE('',#4602,#4603,#3718,.T.);
#5955=EDGE_CURVE('',#4603,#4600,#2697,.T.);
#5956=EDGE_CURVE('',#4601,#4604,#2698,.T.);
#5957=EDGE_CURVE('',#4604,#4605,#2699,.T.);
#5958=EDGE_CURVE('',#4605,#4602,#2700,.T.);
#5959=EDGE_CURVE('',#4606,#4600,#2701,.T.);
#5960=EDGE_CURVE('',#4607,#4606,#2702,.T.);
#5961=EDGE_CURVE('',#4608,#4607,#2703,.T.);
#5962=EDGE_CURVE('',#4608,#4604,#2704,.T.);
#5963=EDGE_CURVE('',#4607,#4609,#2705,.T.);
#5964=EDGE_CURVE('',#4606,#4610,#2706,.T.);
#5965=EDGE_CURVE('',#4610,#4609,#2707,.T.);
#5966=EDGE_CURVE('',#4610,#4603,#2708,.T.);
#5967=EDGE_CURVE('',#4611,#4605,#2709,.T.);
#5968=EDGE_CURVE('',#4609,#4611,#2710,.T.);
#5969=EDGE_CURVE('',#4608,#4542,#2711,.T.);
#5970=EDGE_CURVE('',#4612,#4607,#2712,.T.);
#5971=EDGE_CURVE('',#4613,#4612,#2713,.T.);
#5972=EDGE_CURVE('',#4613,#4614,#2714,.T.);
#5973=EDGE_CURVE('',#4614,#4543,#2715,.T.);
#5974=EDGE_CURVE('',#4615,#4554,#2716,.T.);
#5975=EDGE_CURVE('',#4615,#4616,#2717,.T.);
#5976=EDGE_CURVE('',#4609,#4616,#2718,.T.);
#5977=EDGE_CURVE('',#4537,#4611,#2719,.T.);
#5978=EDGE_CURVE('',#4617,#4575,#2720,.T.);
#5979=EDGE_CURVE('',#4617,#4576,#2721,.T.);
#5980=EDGE_CURVE('',#4569,#4617,#2722,.T.);
#5981=EDGE_CURVE('',#4577,#4569,#2723,.T.);
#5982=EDGE_CURVE('',#4618,#4577,#2724,.T.);
#5983=EDGE_CURVE('',#4618,#4563,#2725,.T.);
#5984=EDGE_CURVE('',#4619,#4598,#2726,.T.);
#5985=EDGE_CURVE('',#4619,#4590,#2727,.T.);
#5986=EDGE_CURVE('',#4620,#4597,#2728,.T.);
#5987=EDGE_CURVE('',#4620,#4619,#2729,.T.);
#5988=EDGE_CURVE('',#4556,#4618,#2730,.T.);
#5989=EDGE_CURVE('',#4582,#4621,#2731,.T.);
#5990=EDGE_CURVE('',#4621,#4618,#2732,.T.);
#5991=EDGE_CURVE('',#4621,#4581,#2733,.T.);
#5992=EDGE_CURVE('',#4589,#4622,#2734,.T.);
#5993=EDGE_CURVE('',#4622,#4583,#2735,.T.);
#5994=EDGE_CURVE('',#4588,#4623,#2736,.T.);
#5995=EDGE_CURVE('',#4622,#4623,#2737,.T.);
#5996=EDGE_CURVE('',#4570,#4624,#3719,.T.);
#5997=EDGE_CURVE('',#4624,#4624,#3720,.T.);
#5998=EDGE_CURVE('',#4625,#4625,#3721,.T.);
#5999=EDGE_CURVE('',#4625,#4626,#2738,.T.);
#6000=EDGE_CURVE('',#4626,#4626,#3722,.T.);
#6001=EDGE_CURVE('',#4627,#4627,#3723,.T.);
#6002=EDGE_CURVE('',#4628,#4627,#2739,.T.);
#6003=EDGE_CURVE('',#4629,#4628,#2740,.T.);
#6004=EDGE_CURVE('',#4630,#4629,#2741,.T.);
#6005=EDGE_CURVE('',#4630,#4631,#2742,.T.);
#6006=EDGE_CURVE('',#4627,#4631,#2743,.T.);
#6007=EDGE_CURVE('',#4627,#4571,#2744,.T.);
#6008=EDGE_CURVE('',#4612,#4629,#2745,.T.);
#6009=EDGE_CURVE('',#4616,#4630,#2746,.T.);
#6010=EDGE_CURVE('',#4623,#4632,#2747,.T.);
#6011=EDGE_CURVE('',#4633,#4587,#3724,.T.);
#6012=EDGE_CURVE('',#4558,#4633,#2748,.T.);
#6013=EDGE_CURVE('',#4631,#4557,#2749,.T.);
#6014=EDGE_CURVE('',#4634,#4615,#2750,.T.);
#6015=EDGE_CURVE('',#4632,#4634,#3725,.T.);
#6016=EDGE_CURVE('',#4633,#4548,#2751,.T.);
#6017=EDGE_CURVE('',#4632,#4552,#2752,.T.);
#6018=EDGE_CURVE('',#4634,#4553,#2753,.T.);
#6019=EDGE_CURVE('',#4628,#4568,#2754,.T.);
#6020=EDGE_CURVE('',#4596,#4635,#3726,.T.);
#6021=EDGE_CURVE('',#4636,#4595,#3727,.T.);
#6022=EDGE_CURVE('',#4635,#4636,#2755,.T.);
#6023=EDGE_CURVE('',#4635,#4613,#2756,.T.);
#6024=EDGE_CURVE('',#4614,#4636,#2757,.T.);
#6025=EDGE_CURVE('',#4637,#4567,#2758,.T.);
#6026=EDGE_CURVE('',#4638,#4566,#2759,.T.);
#6027=EDGE_CURVE('',#4637,#4638,#2760,.T.);
#6028=EDGE_CURVE('',#4637,#4639,#3728,.T.);
#6029=EDGE_CURVE('',#4640,#4638,#3729,.T.);
#6030=EDGE_CURVE('',#4639,#4640,#2761,.T.);
#6031=EDGE_CURVE('',#4639,#4620,#2762,.T.);
#6032=EDGE_CURVE('',#4640,#4599,#2763,.T.);
#6033=EDGE_CURVE('',#4641,#4641,#3730,.T.);
#6034=EDGE_CURVE('',#4641,#4642,#2764,.T.);
#6035=EDGE_CURVE('',#4642,#4642,#3731,.T.);
#6036=EDGE_CURVE('',#4643,#4643,#3732,.T.);
#6037=EDGE_CURVE('',#4643,#4641,#2765,.T.);
#6038=EDGE_CURVE('',#4644,#4645,#2766,.T.);
#6039=EDGE_CURVE('',#4644,#4646,#517,.T.);
#6040=EDGE_CURVE('',#4646,#4647,#3733,.T.);
#6041=EDGE_CURVE('',#4645,#4647,#518,.F.);
#6042=EDGE_CURVE('',#4648,#4649,#2767,.T.);
#6043=EDGE_CURVE('',#4648,#4644,#519,.T.);
#6044=EDGE_CURVE('',#4649,#4645,#520,.F.);
#6045=EDGE_CURVE('',#4650,#4651,#2768,.T.);
#6046=EDGE_CURVE('',#4650,#4648,#521,.T.);
#6047=EDGE_CURVE('',#4651,#4649,#522,.F.);
#6048=EDGE_CURVE('',#4652,#4653,#2769,.T.);
#6049=EDGE_CURVE('',#4652,#4650,#523,.T.);
#6050=EDGE_CURVE('',#4653,#4651,#524,.F.);
#6051=EDGE_CURVE('',#4654,#4655,#2770,.T.);
#6052=EDGE_CURVE('',#4654,#4652,#525,.T.);
#6053=EDGE_CURVE('',#4655,#4653,#526,.F.);
#6054=EDGE_CURVE('',#4656,#4657,#2771,.T.);
#6055=EDGE_CURVE('',#4656,#4654,#527,.T.);
#6056=EDGE_CURVE('',#4657,#4655,#528,.F.);
#6057=EDGE_CURVE('',#4658,#4659,#2772,.T.);
#6058=EDGE_CURVE('',#4658,#4656,#529,.T.);
#6059=EDGE_CURVE('',#4659,#4657,#530,.F.);
#6060=EDGE_CURVE('',#4660,#4661,#2773,.T.);
#6061=EDGE_CURVE('',#4660,#4658,#531,.T.);
#6062=EDGE_CURVE('',#4661,#4659,#532,.F.);
#6063=EDGE_CURVE('',#4662,#4663,#2774,.T.);
#6064=EDGE_CURVE('',#4662,#4660,#533,.T.);
#6065=EDGE_CURVE('',#4663,#4661,#534,.F.);
#6066=EDGE_CURVE('',#4664,#4665,#2775,.T.);
#6067=EDGE_CURVE('',#4664,#4662,#535,.T.);
#6068=EDGE_CURVE('',#4665,#4663,#536,.F.);
#6069=EDGE_CURVE('',#4666,#4667,#2776,.T.);
#6070=EDGE_CURVE('',#4666,#4664,#537,.T.);
#6071=EDGE_CURVE('',#4667,#4665,#538,.F.);
#6072=EDGE_CURVE('',#4668,#4669,#2777,.T.);
#6073=EDGE_CURVE('',#4668,#4666,#539,.T.);
#6074=EDGE_CURVE('',#4669,#4667,#540,.F.);
#6075=EDGE_CURVE('',#4670,#4671,#2778,.T.);
#6076=EDGE_CURVE('',#4670,#4668,#541,.T.);
#6077=EDGE_CURVE('',#4671,#4669,#542,.F.);
#6078=EDGE_CURVE('',#4672,#4673,#2779,.T.);
#6079=EDGE_CURVE('',#4672,#4670,#543,.T.);
#6080=EDGE_CURVE('',#4673,#4671,#544,.F.);
#6081=EDGE_CURVE('',#4674,#4675,#2780,.T.);
#6082=EDGE_CURVE('',#4674,#4672,#545,.T.);
#6083=EDGE_CURVE('',#4675,#4673,#546,.F.);
#6084=EDGE_CURVE('',#4676,#4677,#2781,.T.);
#6085=EDGE_CURVE('',#4678,#4676,#547,.F.);
#6086=EDGE_CURVE('',#4679,#4678,#3734,.T.);
#6087=EDGE_CURVE('',#4679,#4677,#548,.T.);
#6088=EDGE_CURVE('',#4680,#4681,#2782,.T.);
#6089=EDGE_CURVE('',#4676,#4680,#549,.F.);
#6090=EDGE_CURVE('',#4677,#4681,#550,.T.);
#6091=EDGE_CURVE('',#4682,#4683,#2783,.T.);
#6092=EDGE_CURVE('',#4680,#4682,#551,.F.);
#6093=EDGE_CURVE('',#4681,#4683,#552,.T.);
#6094=EDGE_CURVE('',#4684,#4685,#2784,.T.);
#6095=EDGE_CURVE('',#4682,#4684,#553,.F.);
#6096=EDGE_CURVE('',#4683,#4685,#554,.T.);
#6097=EDGE_CURVE('',#4686,#4687,#2785,.T.);
#6098=EDGE_CURVE('',#4684,#4686,#555,.F.);
#6099=EDGE_CURVE('',#4685,#4687,#556,.T.);
#6100=EDGE_CURVE('',#4688,#4689,#2786,.T.);
#6101=EDGE_CURVE('',#4686,#4688,#557,.F.);
#6102=EDGE_CURVE('',#4687,#4689,#558,.T.);
#6103=EDGE_CURVE('',#4690,#4691,#2787,.T.);
#6104=EDGE_CURVE('',#4688,#4690,#559,.F.);
#6105=EDGE_CURVE('',#4689,#4691,#560,.T.);
#6106=EDGE_CURVE('',#4692,#4693,#2788,.T.);
#6107=EDGE_CURVE('',#4690,#4692,#561,.F.);
#6108=EDGE_CURVE('',#4691,#4693,#562,.T.);
#6109=EDGE_CURVE('',#4694,#4695,#2789,.T.);
#6110=EDGE_CURVE('',#4692,#4694,#563,.F.);
#6111=EDGE_CURVE('',#4693,#4695,#564,.T.);
#6112=EDGE_CURVE('',#4696,#4697,#2790,.T.);
#6113=EDGE_CURVE('',#4694,#4696,#565,.F.);
#6114=EDGE_CURVE('',#4695,#4697,#566,.T.);
#6115=EDGE_CURVE('',#4698,#4699,#2791,.T.);
#6116=EDGE_CURVE('',#4696,#4698,#567,.F.);
#6117=EDGE_CURVE('',#4697,#4699,#568,.T.);
#6118=EDGE_CURVE('',#4700,#4701,#2792,.T.);
#6119=EDGE_CURVE('',#4698,#4700,#569,.F.);
#6120=EDGE_CURVE('',#4699,#4701,#570,.T.);
#6121=EDGE_CURVE('',#4702,#4703,#2793,.T.);
#6122=EDGE_CURVE('',#4700,#4702,#571,.F.);
#6123=EDGE_CURVE('',#4701,#4703,#572,.T.);
#6124=EDGE_CURVE('',#4704,#4705,#2794,.T.);
#6125=EDGE_CURVE('',#4702,#4704,#573,.F.);
#6126=EDGE_CURVE('',#4703,#4705,#574,.T.);
#6127=EDGE_CURVE('',#4706,#4707,#2795,.T.);
#6128=EDGE_CURVE('',#4704,#4706,#575,.F.);
#6129=EDGE_CURVE('',#4705,#4707,#576,.T.);
#6130=EDGE_CURVE('',#4708,#4709,#2796,.T.);
#6131=EDGE_CURVE('',#4706,#4708,#577,.F.);
#6132=EDGE_CURVE('',#4707,#4709,#578,.T.);
#6133=EDGE_CURVE('',#4709,#4710,#579,.T.);
#6134=EDGE_CURVE('',#4710,#4711,#3735,.T.);
#6135=EDGE_CURVE('',#4708,#4711,#580,.F.);
#6136=EDGE_CURVE('',#4712,#4675,#581,.F.);
#6137=EDGE_CURVE('',#4712,#4713,#3736,.T.);
#6138=EDGE_CURVE('',#4713,#4674,#582,.T.);
#6139=EDGE_CURVE('',#4714,#4715,#681,.T.);
#6140=EDGE_CURVE('',#4714,#4715,#3737,.T.);
#6141=EDGE_CURVE('',#4716,#4716,#3738,.T.);
#6142=EDGE_CURVE('',#4716,#4717,#2797,.T.);
#6143=EDGE_CURVE('',#4717,#4717,#3739,.T.);
#6144=EDGE_CURVE('',#4718,#4718,#3740,.T.);
#6145=EDGE_CURVE('',#4712,#4719,#583,.F.);
#6146=EDGE_CURVE('',#4719,#4720,#2798,.T.);
#6147=EDGE_CURVE('',#4720,#4720,#3741,.T.);
#6148=EDGE_CURVE('',#4719,#4679,#584,.F.);
#6149=EDGE_CURVE('',#4678,#4713,#585,.T.);
#6150=EDGE_CURVE('',#4647,#4710,#586,.F.);
#6151=EDGE_CURVE('',#4711,#4646,#587,.F.);
#6152=EDGE_CURVE('',#4721,#4722,#3742,.T.);
#6153=EDGE_CURVE('',#4723,#4721,#3743,.T.);
#6154=EDGE_CURVE('',#4715,#4723,#3744,.T.);
#6155=EDGE_CURVE('',#4724,#4714,#3745,.T.);
#6156=EDGE_CURVE('',#4722,#4724,#3746,.T.);
#6157=EDGE_CURVE('',#4715,#4723,#682,.T.);
#6158=EDGE_CURVE('',#4723,#4721,#683,.T.);
#6159=EDGE_CURVE('',#4721,#4722,#684,.T.);
#6160=EDGE_CURVE('',#4722,#4724,#685,.T.);
#6161=EDGE_CURVE('',#4724,#4714,#686,.T.);
#6162=EDGE_CURVE('',#4725,#4726,#2799,.T.);
#6163=EDGE_CURVE('',#4726,#4727,#2800,.T.);
#6164=EDGE_CURVE('',#4727,#4728,#2801,.T.);
#6165=EDGE_CURVE('',#4728,#4729,#2802,.T.);
#6166=EDGE_CURVE('',#4729,#4730,#2803,.T.);
#6167=EDGE_CURVE('',#4730,#4725,#2804,.T.);
#6168=EDGE_CURVE('',#4726,#4714,#2805,.T.);
#6169=EDGE_CURVE('',#4727,#4715,#2806,.T.);
#6170=EDGE_CURVE('',#4728,#4723,#2807,.T.);
#6171=EDGE_CURVE('',#4729,#4721,#2808,.T.);
#6172=EDGE_CURVE('',#4730,#4722,#2809,.T.);
#6173=EDGE_CURVE('',#4725,#4724,#2810,.T.);
#6174=EDGE_CURVE('',#4731,#4731,#3747,.T.);
#6175=EDGE_CURVE('',#4732,#4732,#3748,.T.);
#6176=EDGE_CURVE('',#4732,#4733,#2811,.T.);
#6177=EDGE_CURVE('',#4733,#4734,#3749,.T.);
#6178=EDGE_CURVE('',#4734,#4733,#3750,.T.);
#6179=EDGE_CURVE('',#4734,#4735,#3751,.T.);
#6180=EDGE_CURVE('',#4735,#4736,#3752,.T.);
#6181=EDGE_CURVE('',#4736,#4735,#3753,.T.);
#6182=EDGE_CURVE('',#4736,#4731,#2812,.T.);
#6183=EDGE_CURVE('',#4737,#4737,#3754,.T.);
#6184=EDGE_CURVE('',#4737,#4738,#2813,.T.);
#6185=EDGE_CURVE('',#4738,#4739,#3755,.T.);
#6186=EDGE_CURVE('',#4739,#4738,#3756,.T.);
#6187=EDGE_CURVE('',#4739,#4740,#3757,.T.);
#6188=EDGE_CURVE('',#4740,#4741,#3758,.T.);
#6189=EDGE_CURVE('',#4741,#4740,#3759,.T.);
#6190=EDGE_CURVE('',#4741,#4742,#2814,.T.);
#6191=EDGE_CURVE('',#4742,#4742,#3760,.T.);
#6192=EDGE_CURVE('',#4743,#4744,#2815,.T.);
#6193=EDGE_CURVE('',#4743,#4745,#588,.T.);
#6194=EDGE_CURVE('',#4745,#4746,#3761,.T.);
#6195=EDGE_CURVE('',#4746,#4744,#589,.T.);
#6196=EDGE_CURVE('',#4747,#4748,#2816,.T.);
#6197=EDGE_CURVE('',#4749,#4747,#590,.F.);
#6198=EDGE_CURVE('',#4750,#4749,#591,.F.);
#6199=EDGE_CURVE('',#4751,#4750,#3762,.T.);
#6200=EDGE_CURVE('',#4751,#4748,#592,.T.);
#6201=EDGE_CURVE('',#4748,#4752,#593,.T.);
#6202=EDGE_CURVE('',#4752,#4753,#594,.T.);
#6203=EDGE_CURVE('',#4754,#4753,#3763,.T.);
#6204=EDGE_CURVE('',#4755,#4754,#595,.F.);
#6205=EDGE_CURVE('',#4747,#4755,#596,.F.);
#6206=EDGE_CURVE('',#4744,#4756,#597,.T.);
#6207=EDGE_CURVE('',#4757,#4756,#3764,.T.);
#6208=EDGE_CURVE('',#4757,#4743,#598,.T.);
#6209=EDGE_CURVE('',#4758,#4758,#3765,.T.);
#6210=EDGE_CURVE('',#4758,#4759,#2817,.T.);
#6211=EDGE_CURVE('',#4759,#4759,#3766,.T.);
#6212=EDGE_CURVE('',#4758,#4760,#2818,.T.);
#6213=EDGE_CURVE('',#4760,#4760,#3767,.T.);
#6214=EDGE_CURVE('',#4761,#4746,#599,.T.);
#6215=EDGE_CURVE('',#4745,#4751,#600,.T.);
#6216=EDGE_CURVE('',#4761,#4750,#601,.T.);
#6217=EDGE_CURVE('',#4760,#4762,#2819,.T.);
#6218=EDGE_CURVE('',#4762,#4762,#3768,.T.);
#6219=EDGE_CURVE('',#4763,#4763,#3769,.T.);
#6220=EDGE_CURVE('',#4764,#4765,#3770,.T.);
#6221=EDGE_CURVE('',#4764,#4754,#602,.T.);
#6222=EDGE_CURVE('',#4753,#4757,#603,.T.);
#6223=EDGE_CURVE('',#4765,#4757,#3771,.T.);
#6224=EDGE_CURVE('',#4756,#4764,#604,.T.);
#6225=EDGE_CURVE('',#4765,#4763,#2820,.T.);
#6226=ORIENTED_EDGE('',*,*,#4766,.F.);
#6227=ORIENTED_EDGE('',*,*,#4767,.T.);
#6228=ORIENTED_EDGE('',*,*,#4768,.T.);
#6229=ORIENTED_EDGE('',*,*,#4767,.F.);
#6230=ORIENTED_EDGE('',*,*,#4766,.T.);
#6231=ORIENTED_EDGE('',*,*,#4768,.F.);
#6232=ORIENTED_EDGE('',*,*,#4769,.F.);
#6233=ORIENTED_EDGE('',*,*,#4770,.F.);
#6234=ORIENTED_EDGE('',*,*,#4771,.T.);
#6235=ORIENTED_EDGE('',*,*,#4772,.T.);
#6236=ORIENTED_EDGE('',*,*,#4773,.T.);
#6237=ORIENTED_EDGE('',*,*,#4771,.F.);
#6238=ORIENTED_EDGE('',*,*,#4773,.F.);
#6239=ORIENTED_EDGE('',*,*,#4774,.T.);
#6240=ORIENTED_EDGE('',*,*,#4775,.T.);
#6241=ORIENTED_EDGE('',*,*,#4776,.T.);
#6242=ORIENTED_EDGE('',*,*,#4774,.F.);
#6243=ORIENTED_EDGE('',*,*,#4772,.F.);
#6244=ORIENTED_EDGE('',*,*,#4776,.F.);
#6245=ORIENTED_EDGE('',*,*,#4777,.T.);
#6246=ORIENTED_EDGE('',*,*,#4769,.T.);
#6247=ORIENTED_EDGE('',*,*,#4777,.F.);
#6248=ORIENTED_EDGE('',*,*,#4775,.F.);
#6249=ORIENTED_EDGE('',*,*,#4770,.T.);
#6250=ORIENTED_EDGE('',*,*,#4778,.F.);
#6251=ORIENTED_EDGE('',*,*,#4779,.F.);
#6252=ORIENTED_EDGE('',*,*,#4780,.T.);
#6253=ORIENTED_EDGE('',*,*,#4781,.T.);
#6254=ORIENTED_EDGE('',*,*,#4782,.T.);
#6255=ORIENTED_EDGE('',*,*,#4780,.F.);
#6256=ORIENTED_EDGE('',*,*,#4782,.F.);
#6257=ORIENTED_EDGE('',*,*,#4783,.T.);
#6258=ORIENTED_EDGE('',*,*,#4784,.T.);
#6259=ORIENTED_EDGE('',*,*,#4785,.T.);
#6260=ORIENTED_EDGE('',*,*,#4783,.F.);
#6261=ORIENTED_EDGE('',*,*,#4781,.F.);
#6262=ORIENTED_EDGE('',*,*,#4785,.F.);
#6263=ORIENTED_EDGE('',*,*,#4786,.T.);
#6264=ORIENTED_EDGE('',*,*,#4778,.T.);
#6265=ORIENTED_EDGE('',*,*,#4786,.F.);
#6266=ORIENTED_EDGE('',*,*,#4784,.F.);
#6267=ORIENTED_EDGE('',*,*,#4779,.T.);
#6268=ORIENTED_EDGE('',*,*,#4787,.T.);
#6269=ORIENTED_EDGE('',*,*,#4788,.T.);
#6270=ORIENTED_EDGE('',*,*,#4789,.T.);
#6271=ORIENTED_EDGE('',*,*,#4788,.F.);
#6272=ORIENTED_EDGE('',*,*,#4790,.T.);
#6273=ORIENTED_EDGE('',*,*,#4787,.F.);
#6274=ORIENTED_EDGE('',*,*,#4791,.F.);
#6275=ORIENTED_EDGE('',*,*,#4792,.F.);
#6276=ORIENTED_EDGE('',*,*,#4793,.F.);
#6277=ORIENTED_EDGE('',*,*,#4794,.T.);
#6278=ORIENTED_EDGE('',*,*,#4795,.F.);
#6279=ORIENTED_EDGE('',*,*,#4796,.F.);
#6280=ORIENTED_EDGE('',*,*,#4797,.F.);
#6281=ORIENTED_EDGE('',*,*,#4798,.T.);
#6282=ORIENTED_EDGE('',*,*,#4799,.F.);
#6283=ORIENTED_EDGE('',*,*,#4800,.F.);
#6284=ORIENTED_EDGE('',*,*,#4801,.F.);
#6285=ORIENTED_EDGE('',*,*,#4802,.T.);
#6286=ORIENTED_EDGE('',*,*,#4803,.F.);
#6287=ORIENTED_EDGE('',*,*,#4804,.F.);
#6288=ORIENTED_EDGE('',*,*,#4805,.F.);
#6289=ORIENTED_EDGE('',*,*,#4806,.T.);
#6290=ORIENTED_EDGE('',*,*,#4807,.F.);
#6291=ORIENTED_EDGE('',*,*,#4808,.T.);
#6292=ORIENTED_EDGE('',*,*,#4789,.F.);
#6293=ORIENTED_EDGE('',*,*,#4808,.F.);
#6294=ORIENTED_EDGE('',*,*,#4809,.T.);
#6295=ORIENTED_EDGE('',*,*,#4810,.T.);
#6296=ORIENTED_EDGE('',*,*,#4811,.T.);
#6297=ORIENTED_EDGE('',*,*,#4810,.F.);
#6298=ORIENTED_EDGE('',*,*,#4809,.F.);
#6299=ORIENTED_EDGE('',*,*,#4812,.T.);
#6300=ORIENTED_EDGE('',*,*,#4813,.F.);
#6301=ORIENTED_EDGE('',*,*,#4814,.F.);
#6302=ORIENTED_EDGE('',*,*,#4815,.F.);
#6303=ORIENTED_EDGE('',*,*,#4816,.F.);
#6304=ORIENTED_EDGE('',*,*,#4817,.F.);
#6305=ORIENTED_EDGE('',*,*,#4818,.F.);
#6306=ORIENTED_EDGE('',*,*,#4819,.T.);
#6307=ORIENTED_EDGE('',*,*,#4820,.F.);
#6308=ORIENTED_EDGE('',*,*,#4821,.T.);
#6309=ORIENTED_EDGE('',*,*,#4822,.F.);
#6310=ORIENTED_EDGE('',*,*,#4823,.F.);
#6311=ORIENTED_EDGE('',*,*,#4824,.F.);
#6312=ORIENTED_EDGE('',*,*,#4825,.F.);
#6313=ORIENTED_EDGE('',*,*,#4826,.F.);
#6314=ORIENTED_EDGE('',*,*,#4827,.F.);
#6315=ORIENTED_EDGE('',*,*,#4828,.F.);
#6316=ORIENTED_EDGE('',*,*,#4829,.T.);
#6317=ORIENTED_EDGE('',*,*,#4830,.F.);
#6318=ORIENTED_EDGE('',*,*,#4831,.T.);
#6319=ORIENTED_EDGE('',*,*,#4832,.F.);
#6320=ORIENTED_EDGE('',*,*,#4833,.F.);
#6321=ORIENTED_EDGE('',*,*,#4834,.F.);
#6322=ORIENTED_EDGE('',*,*,#4835,.F.);
#6323=ORIENTED_EDGE('',*,*,#4836,.F.);
#6324=ORIENTED_EDGE('',*,*,#4837,.F.);
#6325=ORIENTED_EDGE('',*,*,#4838,.F.);
#6326=ORIENTED_EDGE('',*,*,#4839,.T.);
#6327=ORIENTED_EDGE('',*,*,#4840,.F.);
#6328=ORIENTED_EDGE('',*,*,#4841,.T.);
#6329=ORIENTED_EDGE('',*,*,#4842,.F.);
#6330=ORIENTED_EDGE('',*,*,#4843,.F.);
#6331=ORIENTED_EDGE('',*,*,#4844,.F.);
#6332=ORIENTED_EDGE('',*,*,#4845,.F.);
#6333=ORIENTED_EDGE('',*,*,#4846,.F.);
#6334=ORIENTED_EDGE('',*,*,#4847,.F.);
#6335=ORIENTED_EDGE('',*,*,#4848,.F.);
#6336=ORIENTED_EDGE('',*,*,#4849,.T.);
#6337=ORIENTED_EDGE('',*,*,#4850,.F.);
#6338=ORIENTED_EDGE('',*,*,#4851,.T.);
#6339=ORIENTED_EDGE('',*,*,#4852,.F.);
#6340=ORIENTED_EDGE('',*,*,#4853,.F.);
#6341=ORIENTED_EDGE('',*,*,#4812,.F.);
#6342=ORIENTED_EDGE('',*,*,#4854,.F.);
#6343=ORIENTED_EDGE('',*,*,#4811,.F.);
#6344=ORIENTED_EDGE('',*,*,#4844,.T.);
#6345=ORIENTED_EDGE('',*,*,#4855,.T.);
#6346=ORIENTED_EDGE('',*,*,#4856,.T.);
#6347=ORIENTED_EDGE('',*,*,#4857,.T.);
#6348=ORIENTED_EDGE('',*,*,#4856,.F.);
#6349=ORIENTED_EDGE('',*,*,#4858,.T.);
#6350=ORIENTED_EDGE('',*,*,#4859,.F.);
#6351=ORIENTED_EDGE('',*,*,#4860,.T.);
#6352=ORIENTED_EDGE('',*,*,#4855,.F.);
#6353=ORIENTED_EDGE('',*,*,#4843,.T.);
#6354=ORIENTED_EDGE('',*,*,#4861,.F.);
#6355=ORIENTED_EDGE('',*,*,#4858,.F.);
#6356=ORIENTED_EDGE('',*,*,#4859,.T.);
#6357=ORIENTED_EDGE('',*,*,#4861,.T.);
#6358=ORIENTED_EDGE('',*,*,#4842,.T.);
#6359=ORIENTED_EDGE('',*,*,#4862,.T.);
#6360=ORIENTED_EDGE('',*,*,#4834,.T.);
#6361=ORIENTED_EDGE('',*,*,#4863,.T.);
#6362=ORIENTED_EDGE('',*,*,#4864,.T.);
#6363=ORIENTED_EDGE('',*,*,#4865,.T.);
#6364=ORIENTED_EDGE('',*,*,#4863,.F.);
#6365=ORIENTED_EDGE('',*,*,#4833,.T.);
#6366=ORIENTED_EDGE('',*,*,#4866,.F.);
#6367=ORIENTED_EDGE('',*,*,#4867,.F.);
#6368=ORIENTED_EDGE('',*,*,#4868,.T.);
#6369=ORIENTED_EDGE('',*,*,#4869,.T.);
#6370=ORIENTED_EDGE('',*,*,#4852,.T.);
#6371=ORIENTED_EDGE('',*,*,#4870,.T.);
#6372=ORIENTED_EDGE('',*,*,#4869,.F.);
#6373=ORIENTED_EDGE('',*,*,#4871,.F.);
#6374=ORIENTED_EDGE('',*,*,#4872,.F.);
#6375=ORIENTED_EDGE('',*,*,#4813,.T.);
#6376=ORIENTED_EDGE('',*,*,#4853,.T.);
#6377=ORIENTED_EDGE('',*,*,#4814,.T.);
#6378=ORIENTED_EDGE('',*,*,#4872,.T.);
#6379=ORIENTED_EDGE('',*,*,#4873,.T.);
#6380=ORIENTED_EDGE('',*,*,#4874,.T.);
#6381=ORIENTED_EDGE('',*,*,#4875,.T.);
#6382=ORIENTED_EDGE('',*,*,#4876,.T.);
#6383=ORIENTED_EDGE('',*,*,#4822,.T.);
#6384=ORIENTED_EDGE('',*,*,#4877,.T.);
#6385=ORIENTED_EDGE('',*,*,#4876,.F.);
#6386=ORIENTED_EDGE('',*,*,#4878,.F.);
#6387=ORIENTED_EDGE('',*,*,#4879,.F.);
#6388=ORIENTED_EDGE('',*,*,#4823,.T.);
#6389=ORIENTED_EDGE('',*,*,#4875,.F.);
#6390=ORIENTED_EDGE('',*,*,#4880,.T.);
#6391=ORIENTED_EDGE('',*,*,#4881,.F.);
#6392=ORIENTED_EDGE('',*,*,#4878,.T.);
#6393=ORIENTED_EDGE('',*,*,#4882,.T.);
#6394=ORIENTED_EDGE('',*,*,#4866,.T.);
#6395=ORIENTED_EDGE('',*,*,#4832,.T.);
#6396=ORIENTED_EDGE('',*,*,#4883,.T.);
#6397=ORIENTED_EDGE('',*,*,#4864,.F.);
#6398=ORIENTED_EDGE('',*,*,#4867,.T.);
#6399=ORIENTED_EDGE('',*,*,#4882,.F.);
#6400=ORIENTED_EDGE('',*,*,#4884,.T.);
#6401=ORIENTED_EDGE('',*,*,#4824,.T.);
#6402=ORIENTED_EDGE('',*,*,#4879,.T.);
#6403=ORIENTED_EDGE('',*,*,#4881,.T.);
#6404=ORIENTED_EDGE('',*,*,#4885,.T.);
#6405=ORIENTED_EDGE('',*,*,#4885,.F.);
#6406=ORIENTED_EDGE('',*,*,#4886,.F.);
#6407=ORIENTED_EDGE('',*,*,#4887,.F.);
#6408=ORIENTED_EDGE('',*,*,#4825,.T.);
#6409=ORIENTED_EDGE('',*,*,#4836,.T.);
#6410=ORIENTED_EDGE('',*,*,#4888,.T.);
#6411=ORIENTED_EDGE('',*,*,#4889,.T.);
#6412=ORIENTED_EDGE('',*,*,#4890,.T.);
#6413=ORIENTED_EDGE('',*,*,#4891,.T.);
#6414=ORIENTED_EDGE('',*,*,#4890,.F.);
#6415=ORIENTED_EDGE('',*,*,#4892,.F.);
#6416=ORIENTED_EDGE('',*,*,#4893,.F.);
#6417=ORIENTED_EDGE('',*,*,#4799,.T.);
#6418=ORIENTED_EDGE('',*,*,#4889,.F.);
#6419=ORIENTED_EDGE('',*,*,#4894,.T.);
#6420=ORIENTED_EDGE('',*,*,#4895,.F.);
#6421=ORIENTED_EDGE('',*,*,#4892,.T.);
#6422=ORIENTED_EDGE('',*,*,#4896,.T.);
#6423=ORIENTED_EDGE('',*,*,#4897,.T.);
#6424=ORIENTED_EDGE('',*,*,#4840,.T.);
#6425=ORIENTED_EDGE('',*,*,#4898,.T.);
#6426=ORIENTED_EDGE('',*,*,#4899,.T.);
#6427=ORIENTED_EDGE('',*,*,#4896,.F.);
#6428=ORIENTED_EDGE('',*,*,#4900,.T.);
#6429=ORIENTED_EDGE('',*,*,#4901,.F.);
#6430=ORIENTED_EDGE('',*,*,#4902,.T.);
#6431=ORIENTED_EDGE('',*,*,#4899,.F.);
#6432=ORIENTED_EDGE('',*,*,#4795,.T.);
#6433=ORIENTED_EDGE('',*,*,#4903,.F.);
#6434=ORIENTED_EDGE('',*,*,#4900,.F.);
#6435=ORIENTED_EDGE('',*,*,#4846,.T.);
#6436=ORIENTED_EDGE('',*,*,#4904,.T.);
#6437=ORIENTED_EDGE('',*,*,#4901,.T.);
#6438=ORIENTED_EDGE('',*,*,#4903,.T.);
#6439=ORIENTED_EDGE('',*,*,#4905,.T.);
#6440=ORIENTED_EDGE('',*,*,#4857,.F.);
#6441=ORIENTED_EDGE('',*,*,#4906,.F.);
#6442=ORIENTED_EDGE('',*,*,#4904,.F.);
#6443=ORIENTED_EDGE('',*,*,#4845,.T.);
#6444=ORIENTED_EDGE('',*,*,#4907,.T.);
#6445=ORIENTED_EDGE('',*,*,#4908,.T.);
#6446=ORIENTED_EDGE('',*,*,#4850,.T.);
#6447=ORIENTED_EDGE('',*,*,#4909,.T.);
#6448=ORIENTED_EDGE('',*,*,#4910,.T.);
#6449=ORIENTED_EDGE('',*,*,#4907,.F.);
#6450=ORIENTED_EDGE('',*,*,#4911,.T.);
#6451=ORIENTED_EDGE('',*,*,#4912,.F.);
#6452=ORIENTED_EDGE('',*,*,#4913,.T.);
#6453=ORIENTED_EDGE('',*,*,#4910,.F.);
#6454=ORIENTED_EDGE('',*,*,#4791,.T.);
#6455=ORIENTED_EDGE('',*,*,#4807,.T.);
#6456=ORIENTED_EDGE('',*,*,#4914,.F.);
#6457=ORIENTED_EDGE('',*,*,#4911,.F.);
#6458=ORIENTED_EDGE('',*,*,#4816,.T.);
#6459=ORIENTED_EDGE('',*,*,#4915,.T.);
#6460=ORIENTED_EDGE('',*,*,#4912,.T.);
#6461=ORIENTED_EDGE('',*,*,#4914,.T.);
#6462=ORIENTED_EDGE('',*,*,#4916,.T.);
#6463=ORIENTED_EDGE('',*,*,#4874,.F.);
#6464=ORIENTED_EDGE('',*,*,#4917,.F.);
#6465=ORIENTED_EDGE('',*,*,#4915,.F.);
#6466=ORIENTED_EDGE('',*,*,#4815,.T.);
#6467=ORIENTED_EDGE('',*,*,#4918,.T.);
#6468=ORIENTED_EDGE('',*,*,#4919,.T.);
#6469=ORIENTED_EDGE('',*,*,#4820,.T.);
#6470=ORIENTED_EDGE('',*,*,#4920,.T.);
#6471=ORIENTED_EDGE('',*,*,#4921,.T.);
#6472=ORIENTED_EDGE('',*,*,#4918,.F.);
#6473=ORIENTED_EDGE('',*,*,#4922,.T.);
#6474=ORIENTED_EDGE('',*,*,#4923,.F.);
#6475=ORIENTED_EDGE('',*,*,#4924,.T.);
#6476=ORIENTED_EDGE('',*,*,#4921,.F.);
#6477=ORIENTED_EDGE('',*,*,#4803,.T.);
#6478=ORIENTED_EDGE('',*,*,#4925,.F.);
#6479=ORIENTED_EDGE('',*,*,#4922,.F.);
#6480=ORIENTED_EDGE('',*,*,#4895,.T.);
#6481=ORIENTED_EDGE('',*,*,#4926,.T.);
#6482=ORIENTED_EDGE('',*,*,#4830,.T.);
#6483=ORIENTED_EDGE('',*,*,#4927,.T.);
#6484=ORIENTED_EDGE('',*,*,#4893,.T.);
#6485=ORIENTED_EDGE('',*,*,#4826,.T.);
#6486=ORIENTED_EDGE('',*,*,#4887,.T.);
#6487=ORIENTED_EDGE('',*,*,#4923,.T.);
#6488=ORIENTED_EDGE('',*,*,#4925,.T.);
#6489=ORIENTED_EDGE('',*,*,#4928,.T.);
#6490=ORIENTED_EDGE('',*,*,#4929,.F.);
#6491=ORIENTED_EDGE('',*,*,#4796,.T.);
#6492=ORIENTED_EDGE('',*,*,#4898,.F.);
#6493=ORIENTED_EDGE('',*,*,#4839,.F.);
#6494=ORIENTED_EDGE('',*,*,#4930,.F.);
#6495=ORIENTED_EDGE('',*,*,#4847,.T.);
#6496=ORIENTED_EDGE('',*,*,#4905,.F.);
#6497=ORIENTED_EDGE('',*,*,#4794,.F.);
#6498=ORIENTED_EDGE('',*,*,#4931,.F.);
#6499=ORIENTED_EDGE('',*,*,#4800,.T.);
#6500=ORIENTED_EDGE('',*,*,#4927,.F.);
#6501=ORIENTED_EDGE('',*,*,#4829,.F.);
#6502=ORIENTED_EDGE('',*,*,#4932,.F.);
#6503=ORIENTED_EDGE('',*,*,#4837,.T.);
#6504=ORIENTED_EDGE('',*,*,#4891,.F.);
#6505=ORIENTED_EDGE('',*,*,#4798,.F.);
#6506=ORIENTED_EDGE('',*,*,#4933,.F.);
#6507=ORIENTED_EDGE('',*,*,#4792,.T.);
#6508=ORIENTED_EDGE('',*,*,#4909,.F.);
#6509=ORIENTED_EDGE('',*,*,#4849,.F.);
#6510=ORIENTED_EDGE('',*,*,#4934,.F.);
#6511=ORIENTED_EDGE('',*,*,#4817,.T.);
#6512=ORIENTED_EDGE('',*,*,#4916,.F.);
#6513=ORIENTED_EDGE('',*,*,#4806,.F.);
#6514=ORIENTED_EDGE('',*,*,#4935,.F.);
#6515=ORIENTED_EDGE('',*,*,#4804,.T.);
#6516=ORIENTED_EDGE('',*,*,#4920,.F.);
#6517=ORIENTED_EDGE('',*,*,#4819,.F.);
#6518=ORIENTED_EDGE('',*,*,#4936,.F.);
#6519=ORIENTED_EDGE('',*,*,#4827,.T.);
#6520=ORIENTED_EDGE('',*,*,#4928,.F.);
#6521=ORIENTED_EDGE('',*,*,#4802,.F.);
#6522=ORIENTED_EDGE('',*,*,#4932,.T.);
#6523=ORIENTED_EDGE('',*,*,#4797,.T.);
#6524=ORIENTED_EDGE('',*,*,#4929,.T.);
#6525=ORIENTED_EDGE('',*,*,#4838,.T.);
#6526=ORIENTED_EDGE('',*,*,#4936,.T.);
#6527=ORIENTED_EDGE('',*,*,#4801,.T.);
#6528=ORIENTED_EDGE('',*,*,#4931,.T.);
#6529=ORIENTED_EDGE('',*,*,#4828,.T.);
#6530=ORIENTED_EDGE('',*,*,#4930,.T.);
#6531=ORIENTED_EDGE('',*,*,#4793,.T.);
#6532=ORIENTED_EDGE('',*,*,#4933,.T.);
#6533=ORIENTED_EDGE('',*,*,#4848,.T.);
#6534=ORIENTED_EDGE('',*,*,#4934,.T.);
#6535=ORIENTED_EDGE('',*,*,#4805,.T.);
#6536=ORIENTED_EDGE('',*,*,#4935,.T.);
#6537=ORIENTED_EDGE('',*,*,#4818,.T.);
#6538=ORIENTED_EDGE('',*,*,#4790,.F.);
#6539=ORIENTED_EDGE('',*,*,#4937,.T.);
#6540=ORIENTED_EDGE('',*,*,#4854,.T.);
#6541=ORIENTED_EDGE('',*,*,#4937,.F.);
#6542=ORIENTED_EDGE('',*,*,#4865,.F.);
#6543=ORIENTED_EDGE('',*,*,#4938,.F.);
#6544=ORIENTED_EDGE('',*,*,#4888,.F.);
#6545=ORIENTED_EDGE('',*,*,#4835,.T.);
#6546=ORIENTED_EDGE('',*,*,#4884,.F.);
#6547=ORIENTED_EDGE('',*,*,#4939,.F.);
#6548=ORIENTED_EDGE('',*,*,#4894,.F.);
#6549=ORIENTED_EDGE('',*,*,#4938,.T.);
#6550=ORIENTED_EDGE('',*,*,#4883,.F.);
#6551=ORIENTED_EDGE('',*,*,#4831,.F.);
#6552=ORIENTED_EDGE('',*,*,#4926,.F.);
#6553=ORIENTED_EDGE('',*,*,#4939,.T.);
#6554=ORIENTED_EDGE('',*,*,#4868,.F.);
#6555=ORIENTED_EDGE('',*,*,#4940,.T.);
#6556=ORIENTED_EDGE('',*,*,#4873,.F.);
#6557=ORIENTED_EDGE('',*,*,#4871,.T.);
#6558=ORIENTED_EDGE('',*,*,#4940,.F.);
#6559=ORIENTED_EDGE('',*,*,#4941,.F.);
#6560=ORIENTED_EDGE('',*,*,#4913,.F.);
#6561=ORIENTED_EDGE('',*,*,#4917,.T.);
#6562=ORIENTED_EDGE('',*,*,#4870,.F.);
#6563=ORIENTED_EDGE('',*,*,#4851,.F.);
#6564=ORIENTED_EDGE('',*,*,#4908,.F.);
#6565=ORIENTED_EDGE('',*,*,#4941,.T.);
#6566=ORIENTED_EDGE('',*,*,#4880,.F.);
#6567=ORIENTED_EDGE('',*,*,#4942,.F.);
#6568=ORIENTED_EDGE('',*,*,#4924,.F.);
#6569=ORIENTED_EDGE('',*,*,#4886,.T.);
#6570=ORIENTED_EDGE('',*,*,#4877,.F.);
#6571=ORIENTED_EDGE('',*,*,#4821,.F.);
#6572=ORIENTED_EDGE('',*,*,#4919,.F.);
#6573=ORIENTED_EDGE('',*,*,#4942,.T.);
#6574=ORIENTED_EDGE('',*,*,#4860,.F.);
#6575=ORIENTED_EDGE('',*,*,#4943,.F.);
#6576=ORIENTED_EDGE('',*,*,#4902,.F.);
#6577=ORIENTED_EDGE('',*,*,#4906,.T.);
#6578=ORIENTED_EDGE('',*,*,#4862,.F.);
#6579=ORIENTED_EDGE('',*,*,#4841,.F.);
#6580=ORIENTED_EDGE('',*,*,#4897,.F.);
#6581=ORIENTED_EDGE('',*,*,#4943,.T.);
#6582=ORIENTED_EDGE('',*,*,#4944,.T.);
#6583=ORIENTED_EDGE('',*,*,#4945,.T.);
#6584=ORIENTED_EDGE('',*,*,#4946,.T.);
#6585=ORIENTED_EDGE('',*,*,#4947,.T.);
#6586=ORIENTED_EDGE('',*,*,#4948,.T.);
#6587=ORIENTED_EDGE('',*,*,#4949,.T.);
#6588=ORIENTED_EDGE('',*,*,#4950,.T.);
#6589=ORIENTED_EDGE('',*,*,#4951,.T.);
#6590=ORIENTED_EDGE('',*,*,#4952,.T.);
#6591=ORIENTED_EDGE('',*,*,#4953,.T.);
#6592=ORIENTED_EDGE('',*,*,#4954,.T.);
#6593=ORIENTED_EDGE('',*,*,#4955,.F.);
#6594=ORIENTED_EDGE('',*,*,#4956,.F.);
#6595=ORIENTED_EDGE('',*,*,#4957,.F.);
#6596=ORIENTED_EDGE('',*,*,#4958,.F.);
#6597=ORIENTED_EDGE('',*,*,#4959,.F.);
#6598=ORIENTED_EDGE('',*,*,#4960,.F.);
#6599=ORIENTED_EDGE('',*,*,#4961,.F.);
#6600=ORIENTED_EDGE('',*,*,#4962,.F.);
#6601=ORIENTED_EDGE('',*,*,#4963,.F.);
#6602=ORIENTED_EDGE('',*,*,#4964,.F.);
#6603=ORIENTED_EDGE('',*,*,#4965,.F.);
#6604=ORIENTED_EDGE('',*,*,#4966,.F.);
#6605=ORIENTED_EDGE('',*,*,#4967,.F.);
#6606=ORIENTED_EDGE('',*,*,#4968,.F.);
#6607=ORIENTED_EDGE('',*,*,#4969,.F.);
#6608=ORIENTED_EDGE('',*,*,#4970,.F.);
#6609=ORIENTED_EDGE('',*,*,#4971,.F.);
#6610=ORIENTED_EDGE('',*,*,#4972,.T.);
#6611=ORIENTED_EDGE('',*,*,#4973,.T.);
#6612=ORIENTED_EDGE('',*,*,#4974,.T.);
#6613=ORIENTED_EDGE('',*,*,#4975,.T.);
#6614=ORIENTED_EDGE('',*,*,#4976,.T.);
#6615=ORIENTED_EDGE('',*,*,#4977,.T.);
#6616=ORIENTED_EDGE('',*,*,#4978,.T.);
#6617=ORIENTED_EDGE('',*,*,#4979,.T.);
#6618=ORIENTED_EDGE('',*,*,#4980,.T.);
#6619=ORIENTED_EDGE('',*,*,#4981,.T.);
#6620=ORIENTED_EDGE('',*,*,#4982,.T.);
#6621=ORIENTED_EDGE('',*,*,#4983,.T.);
#6622=ORIENTED_EDGE('',*,*,#4984,.T.);
#6623=ORIENTED_EDGE('',*,*,#4985,.T.);
#6624=ORIENTED_EDGE('',*,*,#4986,.T.);
#6625=ORIENTED_EDGE('',*,*,#4987,.T.);
#6626=ORIENTED_EDGE('',*,*,#4988,.T.);
#6627=ORIENTED_EDGE('',*,*,#4989,.T.);
#6628=ORIENTED_EDGE('',*,*,#4990,.T.);
#6629=ORIENTED_EDGE('',*,*,#4991,.T.);
#6630=ORIENTED_EDGE('',*,*,#4992,.T.);
#6631=ORIENTED_EDGE('',*,*,#4993,.T.);
#6632=ORIENTED_EDGE('',*,*,#4994,.T.);
#6633=ORIENTED_EDGE('',*,*,#4995,.T.);
#6634=ORIENTED_EDGE('',*,*,#4996,.T.);
#6635=ORIENTED_EDGE('',*,*,#4997,.T.);
#6636=ORIENTED_EDGE('',*,*,#4998,.T.);
#6637=ORIENTED_EDGE('',*,*,#4999,.T.);
#6638=ORIENTED_EDGE('',*,*,#5000,.T.);
#6639=ORIENTED_EDGE('',*,*,#5001,.F.);
#6640=ORIENTED_EDGE('',*,*,#5002,.T.);
#6641=ORIENTED_EDGE('',*,*,#5003,.T.);
#6642=ORIENTED_EDGE('',*,*,#5004,.T.);
#6643=ORIENTED_EDGE('',*,*,#5005,.T.);
#6644=ORIENTED_EDGE('',*,*,#5006,.T.);
#6645=ORIENTED_EDGE('',*,*,#5007,.T.);
#6646=ORIENTED_EDGE('',*,*,#5008,.T.);
#6647=ORIENTED_EDGE('',*,*,#5009,.T.);
#6648=ORIENTED_EDGE('',*,*,#5010,.T.);
#6649=ORIENTED_EDGE('',*,*,#5009,.F.);
#6650=ORIENTED_EDGE('',*,*,#5011,.F.);
#6651=ORIENTED_EDGE('',*,*,#5010,.F.);
#6652=ORIENTED_EDGE('',*,*,#5008,.F.);
#6653=ORIENTED_EDGE('',*,*,#5012,.T.);
#6654=ORIENTED_EDGE('',*,*,#5013,.T.);
#6655=ORIENTED_EDGE('',*,*,#5014,.T.);
#6656=ORIENTED_EDGE('',*,*,#5012,.F.);
#6657=ORIENTED_EDGE('',*,*,#5015,.T.);
#6658=ORIENTED_EDGE('',*,*,#5016,.T.);
#6659=ORIENTED_EDGE('',*,*,#5017,.T.);
#6660=ORIENTED_EDGE('',*,*,#5016,.F.);
#6661=ORIENTED_EDGE('',*,*,#5015,.F.);
#6662=ORIENTED_EDGE('',*,*,#5018,.T.);
#6663=ORIENTED_EDGE('',*,*,#5019,.F.);
#6664=ORIENTED_EDGE('',*,*,#5018,.F.);
#6665=ORIENTED_EDGE('',*,*,#5017,.F.);
#6666=ORIENTED_EDGE('',*,*,#5020,.T.);
#6667=ORIENTED_EDGE('',*,*,#5019,.T.);
#6668=ORIENTED_EDGE('',*,*,#5021,.T.);
#6669=ORIENTED_EDGE('',*,*,#5011,.T.);
#6670=ORIENTED_EDGE('',*,*,#5021,.F.);
#6671=ORIENTED_EDGE('',*,*,#5022,.T.);
#6672=ORIENTED_EDGE('',*,*,#5023,.T.);
#6673=ORIENTED_EDGE('',*,*,#5013,.F.);
#6674=ORIENTED_EDGE('',*,*,#5014,.F.);
#6675=ORIENTED_EDGE('',*,*,#5023,.F.);
#6676=ORIENTED_EDGE('',*,*,#5024,.T.);
#6677=ORIENTED_EDGE('',*,*,#5022,.F.);
#6678=ORIENTED_EDGE('',*,*,#5025,.T.);
#6679=ORIENTED_EDGE('',*,*,#5026,.F.);
#6680=ORIENTED_EDGE('',*,*,#5027,.F.);
#6681=ORIENTED_EDGE('',*,*,#5025,.F.);
#6682=ORIENTED_EDGE('',*,*,#5024,.F.);
#6683=ORIENTED_EDGE('',*,*,#4985,.F.);
#6684=ORIENTED_EDGE('',*,*,#5028,.T.);
#6685=ORIENTED_EDGE('',*,*,#4955,.T.);
#6686=ORIENTED_EDGE('',*,*,#5029,.T.);
#6687=ORIENTED_EDGE('',*,*,#5029,.F.);
#6688=ORIENTED_EDGE('',*,*,#4954,.F.);
#6689=ORIENTED_EDGE('',*,*,#4953,.F.);
#6690=ORIENTED_EDGE('',*,*,#4952,.F.);
#6691=ORIENTED_EDGE('',*,*,#4951,.F.);
#6692=ORIENTED_EDGE('',*,*,#4950,.F.);
#6693=ORIENTED_EDGE('',*,*,#4949,.F.);
#6694=ORIENTED_EDGE('',*,*,#4948,.F.);
#6695=ORIENTED_EDGE('',*,*,#4947,.F.);
#6696=ORIENTED_EDGE('',*,*,#4946,.F.);
#6697=ORIENTED_EDGE('',*,*,#4945,.F.);
#6698=ORIENTED_EDGE('',*,*,#4944,.F.);
#6699=ORIENTED_EDGE('',*,*,#4975,.F.);
#6700=ORIENTED_EDGE('',*,*,#4974,.F.);
#6701=ORIENTED_EDGE('',*,*,#4973,.F.);
#6702=ORIENTED_EDGE('',*,*,#4972,.F.);
#6703=ORIENTED_EDGE('',*,*,#5030,.F.);
#6704=ORIENTED_EDGE('',*,*,#5000,.F.);
#6705=ORIENTED_EDGE('',*,*,#4999,.F.);
#6706=ORIENTED_EDGE('',*,*,#4998,.F.);
#6707=ORIENTED_EDGE('',*,*,#4997,.F.);
#6708=ORIENTED_EDGE('',*,*,#4996,.F.);
#6709=ORIENTED_EDGE('',*,*,#4995,.F.);
#6710=ORIENTED_EDGE('',*,*,#4994,.F.);
#6711=ORIENTED_EDGE('',*,*,#4993,.F.);
#6712=ORIENTED_EDGE('',*,*,#4992,.F.);
#6713=ORIENTED_EDGE('',*,*,#4991,.F.);
#6714=ORIENTED_EDGE('',*,*,#4990,.F.);
#6715=ORIENTED_EDGE('',*,*,#4989,.F.);
#6716=ORIENTED_EDGE('',*,*,#4988,.F.);
#6717=ORIENTED_EDGE('',*,*,#4987,.F.);
#6718=ORIENTED_EDGE('',*,*,#4986,.F.);
#6719=ORIENTED_EDGE('',*,*,#5028,.F.);
#6720=ORIENTED_EDGE('',*,*,#4984,.F.);
#6721=ORIENTED_EDGE('',*,*,#4983,.F.);
#6722=ORIENTED_EDGE('',*,*,#4982,.F.);
#6723=ORIENTED_EDGE('',*,*,#4981,.F.);
#6724=ORIENTED_EDGE('',*,*,#4980,.F.);
#6725=ORIENTED_EDGE('',*,*,#4979,.F.);
#6726=ORIENTED_EDGE('',*,*,#4978,.F.);
#6727=ORIENTED_EDGE('',*,*,#4977,.F.);
#6728=ORIENTED_EDGE('',*,*,#4976,.F.);
#6729=ORIENTED_EDGE('',*,*,#5006,.F.);
#6730=ORIENTED_EDGE('',*,*,#5005,.F.);
#6731=ORIENTED_EDGE('',*,*,#5004,.F.);
#6732=ORIENTED_EDGE('',*,*,#5003,.F.);
#6733=ORIENTED_EDGE('',*,*,#5002,.F.);
#6734=ORIENTED_EDGE('',*,*,#5031,.F.);
#6735=ORIENTED_EDGE('',*,*,#4970,.T.);
#6736=ORIENTED_EDGE('',*,*,#4969,.T.);
#6737=ORIENTED_EDGE('',*,*,#4968,.T.);
#6738=ORIENTED_EDGE('',*,*,#4967,.T.);
#6739=ORIENTED_EDGE('',*,*,#4966,.T.);
#6740=ORIENTED_EDGE('',*,*,#4965,.T.);
#6741=ORIENTED_EDGE('',*,*,#4964,.T.);
#6742=ORIENTED_EDGE('',*,*,#4963,.T.);
#6743=ORIENTED_EDGE('',*,*,#4962,.T.);
#6744=ORIENTED_EDGE('',*,*,#4961,.T.);
#6745=ORIENTED_EDGE('',*,*,#4960,.T.);
#6746=ORIENTED_EDGE('',*,*,#4959,.T.);
#6747=ORIENTED_EDGE('',*,*,#4958,.T.);
#6748=ORIENTED_EDGE('',*,*,#4957,.T.);
#6749=ORIENTED_EDGE('',*,*,#4956,.T.);
#6750=ORIENTED_EDGE('',*,*,#5026,.T.);
#6751=ORIENTED_EDGE('',*,*,#5027,.T.);
#6752=ORIENTED_EDGE('',*,*,#5032,.T.);
#6753=ORIENTED_EDGE('',*,*,#5007,.F.);
#6754=ORIENTED_EDGE('',*,*,#5032,.F.);
#6755=ORIENTED_EDGE('',*,*,#5033,.T.);
#6756=ORIENTED_EDGE('',*,*,#5034,.F.);
#6757=ORIENTED_EDGE('',*,*,#5035,.T.);
#6758=ORIENTED_EDGE('',*,*,#5036,.F.);
#6759=ORIENTED_EDGE('',*,*,#5037,.T.);
#6760=ORIENTED_EDGE('',*,*,#5038,.F.);
#6761=ORIENTED_EDGE('',*,*,#5039,.T.);
#6762=ORIENTED_EDGE('',*,*,#5040,.F.);
#6763=ORIENTED_EDGE('',*,*,#5041,.T.);
#6764=ORIENTED_EDGE('',*,*,#5042,.F.);
#6765=ORIENTED_EDGE('',*,*,#5043,.T.);
#6766=ORIENTED_EDGE('',*,*,#5044,.F.);
#6767=ORIENTED_EDGE('',*,*,#5045,.T.);
#6768=ORIENTED_EDGE('',*,*,#5046,.F.);
#6769=ORIENTED_EDGE('',*,*,#5047,.T.);
#6770=ORIENTED_EDGE('',*,*,#5048,.F.);
#6771=ORIENTED_EDGE('',*,*,#5049,.T.);
#6772=ORIENTED_EDGE('',*,*,#5050,.F.);
#6773=ORIENTED_EDGE('',*,*,#5051,.T.);
#6774=ORIENTED_EDGE('',*,*,#5052,.F.);
#6775=ORIENTED_EDGE('',*,*,#5053,.T.);
#6776=ORIENTED_EDGE('',*,*,#5054,.F.);
#6777=ORIENTED_EDGE('',*,*,#5055,.F.);
#6778=ORIENTED_EDGE('',*,*,#5056,.F.);
#6779=ORIENTED_EDGE('',*,*,#5057,.T.);
#6780=ORIENTED_EDGE('',*,*,#5058,.F.);
#6781=ORIENTED_EDGE('',*,*,#5059,.T.);
#6782=ORIENTED_EDGE('',*,*,#5060,.F.);
#6783=ORIENTED_EDGE('',*,*,#5061,.F.);
#6784=ORIENTED_EDGE('',*,*,#5062,.F.);
#6785=ORIENTED_EDGE('',*,*,#5063,.F.);
#6786=ORIENTED_EDGE('',*,*,#5064,.T.);
#6787=ORIENTED_EDGE('',*,*,#5033,.F.);
#6788=ORIENTED_EDGE('',*,*,#5064,.F.);
#6789=ORIENTED_EDGE('',*,*,#5037,.F.);
#6790=ORIENTED_EDGE('',*,*,#5065,.T.);
#6791=ORIENTED_EDGE('',*,*,#5035,.F.);
#6792=ORIENTED_EDGE('',*,*,#5065,.F.);
#6793=ORIENTED_EDGE('',*,*,#5041,.F.);
#6794=ORIENTED_EDGE('',*,*,#5066,.T.);
#6795=ORIENTED_EDGE('',*,*,#5039,.F.);
#6796=ORIENTED_EDGE('',*,*,#5066,.F.);
#6797=ORIENTED_EDGE('',*,*,#5045,.F.);
#6798=ORIENTED_EDGE('',*,*,#5067,.T.);
#6799=ORIENTED_EDGE('',*,*,#5043,.F.);
#6800=ORIENTED_EDGE('',*,*,#5067,.F.);
#6801=ORIENTED_EDGE('',*,*,#5049,.F.);
#6802=ORIENTED_EDGE('',*,*,#5068,.T.);
#6803=ORIENTED_EDGE('',*,*,#5047,.F.);
#6804=ORIENTED_EDGE('',*,*,#5068,.F.);
#6805=ORIENTED_EDGE('',*,*,#5053,.F.);
#6806=ORIENTED_EDGE('',*,*,#5069,.T.);
#6807=ORIENTED_EDGE('',*,*,#5051,.F.);
#6808=ORIENTED_EDGE('',*,*,#5069,.F.);
#6809=ORIENTED_EDGE('',*,*,#5057,.F.);
#6810=ORIENTED_EDGE('',*,*,#5070,.T.);
#6811=ORIENTED_EDGE('',*,*,#5055,.T.);
#6812=ORIENTED_EDGE('',*,*,#5070,.F.);
#6813=ORIENTED_EDGE('',*,*,#5059,.F.);
#6814=ORIENTED_EDGE('',*,*,#5071,.T.);
#6815=ORIENTED_EDGE('',*,*,#5061,.T.);
#6816=ORIENTED_EDGE('',*,*,#5071,.F.);
#6817=ORIENTED_EDGE('',*,*,#5062,.T.);
#6818=ORIENTED_EDGE('',*,*,#5072,.T.);
#6819=ORIENTED_EDGE('',*,*,#5073,.F.);
#6820=ORIENTED_EDGE('',*,*,#5072,.F.);
#6821=ORIENTED_EDGE('',*,*,#5052,.T.);
#6822=ORIENTED_EDGE('',*,*,#5074,.T.);
#6823=ORIENTED_EDGE('',*,*,#5058,.T.);
#6824=ORIENTED_EDGE('',*,*,#5074,.F.);
#6825=ORIENTED_EDGE('',*,*,#5048,.T.);
#6826=ORIENTED_EDGE('',*,*,#5075,.T.);
#6827=ORIENTED_EDGE('',*,*,#5054,.T.);
#6828=ORIENTED_EDGE('',*,*,#5075,.F.);
#6829=ORIENTED_EDGE('',*,*,#5044,.T.);
#6830=ORIENTED_EDGE('',*,*,#5076,.T.);
#6831=ORIENTED_EDGE('',*,*,#5050,.T.);
#6832=ORIENTED_EDGE('',*,*,#5076,.F.);
#6833=ORIENTED_EDGE('',*,*,#5040,.T.);
#6834=ORIENTED_EDGE('',*,*,#5077,.T.);
#6835=ORIENTED_EDGE('',*,*,#5046,.T.);
#6836=ORIENTED_EDGE('',*,*,#5077,.F.);
#6837=ORIENTED_EDGE('',*,*,#5036,.T.);
#6838=ORIENTED_EDGE('',*,*,#5078,.T.);
#6839=ORIENTED_EDGE('',*,*,#5042,.T.);
#6840=ORIENTED_EDGE('',*,*,#5078,.F.);
#6841=ORIENTED_EDGE('',*,*,#5034,.T.);
#6842=ORIENTED_EDGE('',*,*,#5079,.T.);
#6843=ORIENTED_EDGE('',*,*,#5038,.T.);
#6844=ORIENTED_EDGE('',*,*,#5079,.F.);
#6845=ORIENTED_EDGE('',*,*,#5063,.T.);
#6846=ORIENTED_EDGE('',*,*,#5031,.T.);
#6847=ORIENTED_EDGE('',*,*,#5001,.T.);
#6848=ORIENTED_EDGE('',*,*,#5030,.T.);
#6849=ORIENTED_EDGE('',*,*,#4971,.T.);
#6850=ORIENTED_EDGE('',*,*,#5080,.F.);
#6851=ORIENTED_EDGE('',*,*,#5081,.T.);
#6852=ORIENTED_EDGE('',*,*,#5082,.F.);
#6853=ORIENTED_EDGE('',*,*,#5081,.F.);
#6854=ORIENTED_EDGE('',*,*,#5083,.F.);
#6855=ORIENTED_EDGE('',*,*,#5084,.T.);
#6856=ORIENTED_EDGE('',*,*,#5085,.F.);
#6857=ORIENTED_EDGE('',*,*,#5084,.F.);
#6858=ORIENTED_EDGE('',*,*,#5086,.F.);
#6859=ORIENTED_EDGE('',*,*,#5087,.T.);
#6860=ORIENTED_EDGE('',*,*,#5088,.F.);
#6861=ORIENTED_EDGE('',*,*,#5087,.F.);
#6862=ORIENTED_EDGE('',*,*,#5089,.F.);
#6863=ORIENTED_EDGE('',*,*,#5090,.T.);
#6864=ORIENTED_EDGE('',*,*,#5091,.F.);
#6865=ORIENTED_EDGE('',*,*,#5090,.F.);
#6866=ORIENTED_EDGE('',*,*,#5056,.T.);
#6867=ORIENTED_EDGE('',*,*,#5092,.T.);
#6868=ORIENTED_EDGE('',*,*,#5060,.T.);
#6869=ORIENTED_EDGE('',*,*,#5092,.F.);
#6870=ORIENTED_EDGE('',*,*,#5093,.F.);
#6871=ORIENTED_EDGE('',*,*,#5089,.T.);
#6872=ORIENTED_EDGE('',*,*,#5094,.F.);
#6873=ORIENTED_EDGE('',*,*,#5095,.T.);
#6874=ORIENTED_EDGE('',*,*,#5093,.T.);
#6875=ORIENTED_EDGE('',*,*,#5095,.F.);
#6876=ORIENTED_EDGE('',*,*,#5094,.T.);
#6877=ORIENTED_EDGE('',*,*,#5073,.T.);
#6878=ORIENTED_EDGE('',*,*,#5096,.F.);
#6879=ORIENTED_EDGE('',*,*,#5086,.T.);
#6880=ORIENTED_EDGE('',*,*,#5097,.F.);
#6881=ORIENTED_EDGE('',*,*,#5098,.T.);
#6882=ORIENTED_EDGE('',*,*,#5096,.T.);
#6883=ORIENTED_EDGE('',*,*,#5098,.F.);
#6884=ORIENTED_EDGE('',*,*,#5097,.T.);
#6885=ORIENTED_EDGE('',*,*,#5091,.T.);
#6886=ORIENTED_EDGE('',*,*,#5099,.F.);
#6887=ORIENTED_EDGE('',*,*,#5080,.T.);
#6888=ORIENTED_EDGE('',*,*,#5100,.F.);
#6889=ORIENTED_EDGE('',*,*,#5101,.T.);
#6890=ORIENTED_EDGE('',*,*,#5099,.T.);
#6891=ORIENTED_EDGE('',*,*,#5101,.F.);
#6892=ORIENTED_EDGE('',*,*,#5100,.T.);
#6893=ORIENTED_EDGE('',*,*,#5088,.T.);
#6894=ORIENTED_EDGE('',*,*,#5102,.F.);
#6895=ORIENTED_EDGE('',*,*,#5083,.T.);
#6896=ORIENTED_EDGE('',*,*,#5103,.F.);
#6897=ORIENTED_EDGE('',*,*,#5104,.T.);
#6898=ORIENTED_EDGE('',*,*,#5102,.T.);
#6899=ORIENTED_EDGE('',*,*,#5104,.F.);
#6900=ORIENTED_EDGE('',*,*,#5103,.T.);
#6901=ORIENTED_EDGE('',*,*,#5082,.T.);
#6902=ORIENTED_EDGE('',*,*,#5105,.F.);
#6903=ORIENTED_EDGE('',*,*,#5106,.T.);
#6904=ORIENTED_EDGE('',*,*,#5107,.F.);
#6905=ORIENTED_EDGE('',*,*,#5108,.T.);
#6906=ORIENTED_EDGE('',*,*,#5105,.T.);
#6907=ORIENTED_EDGE('',*,*,#5108,.F.);
#6908=ORIENTED_EDGE('',*,*,#5107,.T.);
#6909=ORIENTED_EDGE('',*,*,#5085,.T.);
#6910=ORIENTED_EDGE('',*,*,#5106,.F.);
#6911=ORIENTED_EDGE('',*,*,#5109,.T.);
#6912=ORIENTED_EDGE('',*,*,#5020,.F.);
#6913=ORIENTED_EDGE('',*,*,#5109,.F.);
#6914=ORIENTED_EDGE('',*,*,#5110,.T.);
#6915=ORIENTED_EDGE('',*,*,#5111,.T.);
#6916=ORIENTED_EDGE('',*,*,#5112,.T.);
#6917=ORIENTED_EDGE('',*,*,#5113,.F.);
#6918=ORIENTED_EDGE('',*,*,#5111,.F.);
#6919=ORIENTED_EDGE('',*,*,#5114,.F.);
#6920=ORIENTED_EDGE('',*,*,#5115,.F.);
#6921=ORIENTED_EDGE('',*,*,#5116,.T.);
#6922=ORIENTED_EDGE('',*,*,#5117,.T.);
#6923=ORIENTED_EDGE('',*,*,#5118,.T.);
#6924=ORIENTED_EDGE('',*,*,#5119,.F.);
#6925=ORIENTED_EDGE('',*,*,#5117,.F.);
#6926=ORIENTED_EDGE('',*,*,#5120,.F.);
#6927=ORIENTED_EDGE('',*,*,#5121,.F.);
#6928=ORIENTED_EDGE('',*,*,#5115,.T.);
#6929=ORIENTED_EDGE('',*,*,#5122,.F.);
#6930=ORIENTED_EDGE('',*,*,#5123,.T.);
#6931=ORIENTED_EDGE('',*,*,#5124,.T.);
#6932=ORIENTED_EDGE('',*,*,#5125,.F.);
#6933=ORIENTED_EDGE('',*,*,#5112,.F.);
#6934=ORIENTED_EDGE('',*,*,#5114,.T.);
#6935=ORIENTED_EDGE('',*,*,#5110,.F.);
#6936=ORIENTED_EDGE('',*,*,#5126,.F.);
#6937=ORIENTED_EDGE('',*,*,#5127,.F.);
#6938=ORIENTED_EDGE('',*,*,#5128,.T.);
#6939=ORIENTED_EDGE('',*,*,#5122,.T.);
#6940=ORIENTED_EDGE('',*,*,#5121,.T.);
#6941=ORIENTED_EDGE('',*,*,#5129,.F.);
#6942=ORIENTED_EDGE('',*,*,#5130,.F.);
#6943=ORIENTED_EDGE('',*,*,#5131,.T.);
#6944=ORIENTED_EDGE('',*,*,#5132,.F.);
#6945=ORIENTED_EDGE('',*,*,#5118,.F.);
#6946=ORIENTED_EDGE('',*,*,#5133,.F.);
#6947=ORIENTED_EDGE('',*,*,#5134,.T.);
#6948=ORIENTED_EDGE('',*,*,#5135,.F.);
#6949=ORIENTED_EDGE('',*,*,#5136,.F.);
#6950=ORIENTED_EDGE('',*,*,#5137,.F.);
#6951=ORIENTED_EDGE('',*,*,#5138,.T.);
#6952=ORIENTED_EDGE('',*,*,#5139,.F.);
#6953=ORIENTED_EDGE('',*,*,#5140,.F.);
#6954=ORIENTED_EDGE('',*,*,#5141,.T.);
#6955=ORIENTED_EDGE('',*,*,#5139,.T.);
#6956=ORIENTED_EDGE('',*,*,#5142,.T.);
#6957=ORIENTED_EDGE('',*,*,#5135,.T.);
#6958=ORIENTED_EDGE('',*,*,#5143,.F.);
#6959=ORIENTED_EDGE('',*,*,#5127,.T.);
#6960=ORIENTED_EDGE('',*,*,#5144,.F.);
#6961=ORIENTED_EDGE('',*,*,#5131,.F.);
#6962=ORIENTED_EDGE('',*,*,#5145,.F.);
#6963=ORIENTED_EDGE('',*,*,#5146,.F.);
#6964=ORIENTED_EDGE('',*,*,#5147,.T.);
#6965=ORIENTED_EDGE('',*,*,#5129,.T.);
#6966=ORIENTED_EDGE('',*,*,#5120,.T.);
#6967=ORIENTED_EDGE('',*,*,#5116,.F.);
#6968=ORIENTED_EDGE('',*,*,#5148,.F.);
#6969=ORIENTED_EDGE('',*,*,#5146,.T.);
#6970=ORIENTED_EDGE('',*,*,#5149,.F.);
#6971=ORIENTED_EDGE('',*,*,#5140,.T.);
#6972=ORIENTED_EDGE('',*,*,#5141,.F.);
#6973=ORIENTED_EDGE('',*,*,#5134,.F.);
#6974=ORIENTED_EDGE('',*,*,#5150,.F.);
#6975=ORIENTED_EDGE('',*,*,#5136,.T.);
#6976=ORIENTED_EDGE('',*,*,#5142,.F.);
#6977=ORIENTED_EDGE('',*,*,#5138,.F.);
#6978=ORIENTED_EDGE('',*,*,#5151,.F.);
#6979=ORIENTED_EDGE('',*,*,#5124,.F.);
#6980=ORIENTED_EDGE('',*,*,#5113,.T.);
#6981=ORIENTED_EDGE('',*,*,#5125,.T.);
#6982=ORIENTED_EDGE('',*,*,#5151,.T.);
#6983=ORIENTED_EDGE('',*,*,#5137,.T.);
#6984=ORIENTED_EDGE('',*,*,#5149,.T.);
#6985=ORIENTED_EDGE('',*,*,#5145,.T.);
#6986=ORIENTED_EDGE('',*,*,#5119,.T.);
#6987=ORIENTED_EDGE('',*,*,#5132,.T.);
#6988=ORIENTED_EDGE('',*,*,#5144,.T.);
#6989=ORIENTED_EDGE('',*,*,#5126,.T.);
#6990=ORIENTED_EDGE('',*,*,#5128,.F.);
#6991=ORIENTED_EDGE('',*,*,#5143,.T.);
#6992=ORIENTED_EDGE('',*,*,#5130,.T.);
#6993=ORIENTED_EDGE('',*,*,#5147,.F.);
#6994=ORIENTED_EDGE('',*,*,#5148,.T.);
#6995=ORIENTED_EDGE('',*,*,#5133,.T.);
#6996=ORIENTED_EDGE('',*,*,#5150,.T.);
#6997=ORIENTED_EDGE('',*,*,#5123,.F.);
#6998=ORIENTED_EDGE('',*,*,#5152,.F.);
#6999=ORIENTED_EDGE('',*,*,#5153,.F.);
#7000=ORIENTED_EDGE('',*,*,#5154,.T.);
#7001=ORIENTED_EDGE('',*,*,#5155,.T.);
#7002=ORIENTED_EDGE('',*,*,#5156,.T.);
#7003=ORIENTED_EDGE('',*,*,#5154,.F.);
#7004=ORIENTED_EDGE('',*,*,#5156,.F.);
#7005=ORIENTED_EDGE('',*,*,#5157,.T.);
#7006=ORIENTED_EDGE('',*,*,#5158,.T.);
#7007=ORIENTED_EDGE('',*,*,#5159,.T.);
#7008=ORIENTED_EDGE('',*,*,#5157,.F.);
#7009=ORIENTED_EDGE('',*,*,#5155,.F.);
#7010=ORIENTED_EDGE('',*,*,#5159,.F.);
#7011=ORIENTED_EDGE('',*,*,#5160,.T.);
#7012=ORIENTED_EDGE('',*,*,#5152,.T.);
#7013=ORIENTED_EDGE('',*,*,#5160,.F.);
#7014=ORIENTED_EDGE('',*,*,#5158,.F.);
#7015=ORIENTED_EDGE('',*,*,#5153,.T.);
#7016=ORIENTED_EDGE('',*,*,#5161,.F.);
#7017=ORIENTED_EDGE('',*,*,#5162,.T.);
#7018=ORIENTED_EDGE('',*,*,#5163,.T.);
#7019=ORIENTED_EDGE('',*,*,#5164,.T.);
#7020=ORIENTED_EDGE('',*,*,#5162,.F.);
#7021=ORIENTED_EDGE('',*,*,#5164,.F.);
#7022=ORIENTED_EDGE('',*,*,#5165,.T.);
#7023=ORIENTED_EDGE('',*,*,#5166,.T.);
#7024=ORIENTED_EDGE('',*,*,#5167,.T.);
#7025=ORIENTED_EDGE('',*,*,#5165,.F.);
#7026=ORIENTED_EDGE('',*,*,#5163,.F.);
#7027=ORIENTED_EDGE('',*,*,#5167,.F.);
#7028=ORIENTED_EDGE('',*,*,#5168,.T.);
#7029=ORIENTED_EDGE('',*,*,#5169,.T.);
#7030=ORIENTED_EDGE('',*,*,#5168,.F.);
#7031=ORIENTED_EDGE('',*,*,#5166,.F.);
#7032=ORIENTED_EDGE('',*,*,#5161,.T.);
#7033=ORIENTED_EDGE('',*,*,#5169,.F.);
#7034=ORIENTED_EDGE('',*,*,#5170,.F.);
#7035=ORIENTED_EDGE('',*,*,#5171,.T.);
#7036=ORIENTED_EDGE('',*,*,#5172,.T.);
#7037=ORIENTED_EDGE('',*,*,#5173,.T.);
#7038=ORIENTED_EDGE('',*,*,#5171,.F.);
#7039=ORIENTED_EDGE('',*,*,#5173,.F.);
#7040=ORIENTED_EDGE('',*,*,#5174,.T.);
#7041=ORIENTED_EDGE('',*,*,#5175,.T.);
#7042=ORIENTED_EDGE('',*,*,#5176,.T.);
#7043=ORIENTED_EDGE('',*,*,#5174,.F.);
#7044=ORIENTED_EDGE('',*,*,#5172,.F.);
#7045=ORIENTED_EDGE('',*,*,#5176,.F.);
#7046=ORIENTED_EDGE('',*,*,#5177,.T.);
#7047=ORIENTED_EDGE('',*,*,#5178,.T.);
#7048=ORIENTED_EDGE('',*,*,#5177,.F.);
#7049=ORIENTED_EDGE('',*,*,#5175,.F.);
#7050=ORIENTED_EDGE('',*,*,#5170,.T.);
#7051=ORIENTED_EDGE('',*,*,#5178,.F.);
#7052=ORIENTED_EDGE('',*,*,#5179,.T.);
#7053=ORIENTED_EDGE('',*,*,#5180,.T.);
#7054=ORIENTED_EDGE('',*,*,#5181,.T.);
#7055=ORIENTED_EDGE('',*,*,#5182,.F.);
#7056=ORIENTED_EDGE('',*,*,#5183,.F.);
#7057=ORIENTED_EDGE('',*,*,#5184,.F.);
#7058=ORIENTED_EDGE('',*,*,#5185,.T.);
#7059=ORIENTED_EDGE('',*,*,#5186,.T.);
#7060=ORIENTED_EDGE('',*,*,#5187,.T.);
#7061=ORIENTED_EDGE('',*,*,#5179,.F.);
#7062=ORIENTED_EDGE('',*,*,#5188,.F.);
#7063=ORIENTED_EDGE('',*,*,#5189,.T.);
#7064=ORIENTED_EDGE('',*,*,#5190,.T.);
#7065=ORIENTED_EDGE('',*,*,#5185,.F.);
#7066=ORIENTED_EDGE('',*,*,#5191,.F.);
#7067=ORIENTED_EDGE('',*,*,#5192,.F.);
#7068=ORIENTED_EDGE('',*,*,#5193,.T.);
#7069=ORIENTED_EDGE('',*,*,#5194,.T.);
#7070=ORIENTED_EDGE('',*,*,#5189,.F.);
#7071=ORIENTED_EDGE('',*,*,#5195,.F.);
#7072=ORIENTED_EDGE('',*,*,#5196,.T.);
#7073=ORIENTED_EDGE('',*,*,#5197,.T.);
#7074=ORIENTED_EDGE('',*,*,#5193,.F.);
#7075=ORIENTED_EDGE('',*,*,#5198,.F.);
#7076=ORIENTED_EDGE('',*,*,#5199,.T.);
#7077=ORIENTED_EDGE('',*,*,#5200,.T.);
#7078=ORIENTED_EDGE('',*,*,#5196,.F.);
#7079=ORIENTED_EDGE('',*,*,#5201,.F.);
#7080=ORIENTED_EDGE('',*,*,#5202,.T.);
#7081=ORIENTED_EDGE('',*,*,#5203,.T.);
#7082=ORIENTED_EDGE('',*,*,#5204,.T.);
#7083=ORIENTED_EDGE('',*,*,#5199,.F.);
#7084=ORIENTED_EDGE('',*,*,#5205,.F.);
#7085=ORIENTED_EDGE('',*,*,#5206,.F.);
#7086=ORIENTED_EDGE('',*,*,#5207,.F.);
#7087=ORIENTED_EDGE('',*,*,#5208,.F.);
#7088=ORIENTED_EDGE('',*,*,#5209,.T.);
#7089=ORIENTED_EDGE('',*,*,#5210,.T.);
#7090=ORIENTED_EDGE('',*,*,#5211,.T.);
#7091=ORIENTED_EDGE('',*,*,#5212,.T.);
#7092=ORIENTED_EDGE('',*,*,#5213,.F.);
#7093=ORIENTED_EDGE('',*,*,#5214,.F.);
#7094=ORIENTED_EDGE('',*,*,#5215,.T.);
#7095=ORIENTED_EDGE('',*,*,#5216,.T.);
#7096=ORIENTED_EDGE('',*,*,#5217,.T.);
#7097=ORIENTED_EDGE('',*,*,#5210,.F.);
#7098=ORIENTED_EDGE('',*,*,#5218,.F.);
#7099=ORIENTED_EDGE('',*,*,#5219,.F.);
#7100=ORIENTED_EDGE('',*,*,#5220,.T.);
#7101=ORIENTED_EDGE('',*,*,#5221,.T.);
#7102=ORIENTED_EDGE('',*,*,#5215,.F.);
#7103=ORIENTED_EDGE('',*,*,#5222,.F.);
#7104=ORIENTED_EDGE('',*,*,#5223,.T.);
#7105=ORIENTED_EDGE('',*,*,#5224,.T.);
#7106=ORIENTED_EDGE('',*,*,#5220,.F.);
#7107=ORIENTED_EDGE('',*,*,#5225,.F.);
#7108=ORIENTED_EDGE('',*,*,#5226,.T.);
#7109=ORIENTED_EDGE('',*,*,#5227,.T.);
#7110=ORIENTED_EDGE('',*,*,#5223,.F.);
#7111=ORIENTED_EDGE('',*,*,#5228,.F.);
#7112=ORIENTED_EDGE('',*,*,#5229,.T.);
#7113=ORIENTED_EDGE('',*,*,#5230,.T.);
#7114=ORIENTED_EDGE('',*,*,#5231,.T.);
#7115=ORIENTED_EDGE('',*,*,#5226,.F.);
#7116=ORIENTED_EDGE('',*,*,#5232,.F.);
#7117=ORIENTED_EDGE('',*,*,#5233,.F.);
#7118=ORIENTED_EDGE('',*,*,#5234,.T.);
#7119=ORIENTED_EDGE('',*,*,#5235,.T.);
#7120=ORIENTED_EDGE('',*,*,#5229,.F.);
#7121=ORIENTED_EDGE('',*,*,#5236,.F.);
#7122=ORIENTED_EDGE('',*,*,#5237,.T.);
#7123=ORIENTED_EDGE('',*,*,#5238,.T.);
#7124=ORIENTED_EDGE('',*,*,#5234,.F.);
#7125=ORIENTED_EDGE('',*,*,#5239,.F.);
#7126=ORIENTED_EDGE('',*,*,#5240,.T.);
#7127=ORIENTED_EDGE('',*,*,#5241,.T.);
#7128=ORIENTED_EDGE('',*,*,#5237,.F.);
#7129=ORIENTED_EDGE('',*,*,#5242,.F.);
#7130=ORIENTED_EDGE('',*,*,#5243,.T.);
#7131=ORIENTED_EDGE('',*,*,#5244,.T.);
#7132=ORIENTED_EDGE('',*,*,#5240,.F.);
#7133=ORIENTED_EDGE('',*,*,#5245,.F.);
#7134=ORIENTED_EDGE('',*,*,#5246,.T.);
#7135=ORIENTED_EDGE('',*,*,#5247,.T.);
#7136=ORIENTED_EDGE('',*,*,#5243,.F.);
#7137=ORIENTED_EDGE('',*,*,#5248,.F.);
#7138=ORIENTED_EDGE('',*,*,#5249,.F.);
#7139=ORIENTED_EDGE('',*,*,#5250,.T.);
#7140=ORIENTED_EDGE('',*,*,#5251,.T.);
#7141=ORIENTED_EDGE('',*,*,#5252,.T.);
#7142=ORIENTED_EDGE('',*,*,#5246,.F.);
#7143=ORIENTED_EDGE('',*,*,#5253,.F.);
#7144=ORIENTED_EDGE('',*,*,#5254,.F.);
#7145=ORIENTED_EDGE('',*,*,#5255,.F.);
#7146=ORIENTED_EDGE('',*,*,#5256,.F.);
#7147=ORIENTED_EDGE('',*,*,#5257,.T.);
#7148=ORIENTED_EDGE('',*,*,#5258,.T.);
#7149=ORIENTED_EDGE('',*,*,#5259,.T.);
#7150=ORIENTED_EDGE('',*,*,#5260,.F.);
#7151=ORIENTED_EDGE('',*,*,#5261,.T.);
#7152=ORIENTED_EDGE('',*,*,#5262,.T.);
#7153=ORIENTED_EDGE('',*,*,#5263,.T.);
#7154=ORIENTED_EDGE('',*,*,#5258,.F.);
#7155=ORIENTED_EDGE('',*,*,#5264,.T.);
#7156=ORIENTED_EDGE('',*,*,#5265,.T.);
#7157=ORIENTED_EDGE('',*,*,#5266,.T.);
#7158=ORIENTED_EDGE('',*,*,#5262,.F.);
#7159=ORIENTED_EDGE('',*,*,#5267,.T.);
#7160=ORIENTED_EDGE('',*,*,#5268,.T.);
#7161=ORIENTED_EDGE('',*,*,#5269,.T.);
#7162=ORIENTED_EDGE('',*,*,#5265,.F.);
#7163=ORIENTED_EDGE('',*,*,#5270,.T.);
#7164=ORIENTED_EDGE('',*,*,#5271,.T.);
#7165=ORIENTED_EDGE('',*,*,#5272,.T.);
#7166=ORIENTED_EDGE('',*,*,#5268,.F.);
#7167=ORIENTED_EDGE('',*,*,#5273,.T.);
#7168=ORIENTED_EDGE('',*,*,#5274,.T.);
#7169=ORIENTED_EDGE('',*,*,#5275,.T.);
#7170=ORIENTED_EDGE('',*,*,#5271,.F.);
#7171=ORIENTED_EDGE('',*,*,#5276,.T.);
#7172=ORIENTED_EDGE('',*,*,#5277,.F.);
#7173=ORIENTED_EDGE('',*,*,#5278,.T.);
#7174=ORIENTED_EDGE('',*,*,#5279,.F.);
#7175=ORIENTED_EDGE('',*,*,#5280,.T.);
#7176=ORIENTED_EDGE('',*,*,#5281,.T.);
#7177=ORIENTED_EDGE('',*,*,#5282,.T.);
#7178=ORIENTED_EDGE('',*,*,#5283,.F.);
#7179=ORIENTED_EDGE('',*,*,#5284,.T.);
#7180=ORIENTED_EDGE('',*,*,#5285,.T.);
#7181=ORIENTED_EDGE('',*,*,#5286,.T.);
#7182=ORIENTED_EDGE('',*,*,#5281,.F.);
#7183=ORIENTED_EDGE('',*,*,#5287,.T.);
#7184=ORIENTED_EDGE('',*,*,#5288,.T.);
#7185=ORIENTED_EDGE('',*,*,#5289,.T.);
#7186=ORIENTED_EDGE('',*,*,#5285,.F.);
#7187=ORIENTED_EDGE('',*,*,#5290,.T.);
#7188=ORIENTED_EDGE('',*,*,#5291,.T.);
#7189=ORIENTED_EDGE('',*,*,#5292,.T.);
#7190=ORIENTED_EDGE('',*,*,#5288,.F.);
#7191=ORIENTED_EDGE('',*,*,#5293,.T.);
#7192=ORIENTED_EDGE('',*,*,#5294,.T.);
#7193=ORIENTED_EDGE('',*,*,#5295,.T.);
#7194=ORIENTED_EDGE('',*,*,#5291,.F.);
#7195=ORIENTED_EDGE('',*,*,#5296,.T.);
#7196=ORIENTED_EDGE('',*,*,#5297,.T.);
#7197=ORIENTED_EDGE('',*,*,#5298,.T.);
#7198=ORIENTED_EDGE('',*,*,#5294,.F.);
#7199=ORIENTED_EDGE('',*,*,#5299,.T.);
#7200=ORIENTED_EDGE('',*,*,#5300,.T.);
#7201=ORIENTED_EDGE('',*,*,#5301,.T.);
#7202=ORIENTED_EDGE('',*,*,#5297,.F.);
#7203=ORIENTED_EDGE('',*,*,#5302,.T.);
#7204=ORIENTED_EDGE('',*,*,#5303,.T.);
#7205=ORIENTED_EDGE('',*,*,#5304,.T.);
#7206=ORIENTED_EDGE('',*,*,#5300,.F.);
#7207=ORIENTED_EDGE('',*,*,#5305,.T.);
#7208=ORIENTED_EDGE('',*,*,#5306,.T.);
#7209=ORIENTED_EDGE('',*,*,#5307,.T.);
#7210=ORIENTED_EDGE('',*,*,#5303,.F.);
#7211=ORIENTED_EDGE('',*,*,#5308,.T.);
#7212=ORIENTED_EDGE('',*,*,#5309,.T.);
#7213=ORIENTED_EDGE('',*,*,#5310,.T.);
#7214=ORIENTED_EDGE('',*,*,#5306,.F.);
#7215=ORIENTED_EDGE('',*,*,#5311,.T.);
#7216=ORIENTED_EDGE('',*,*,#5312,.T.);
#7217=ORIENTED_EDGE('',*,*,#5313,.T.);
#7218=ORIENTED_EDGE('',*,*,#5309,.F.);
#7219=ORIENTED_EDGE('',*,*,#5314,.T.);
#7220=ORIENTED_EDGE('',*,*,#5315,.F.);
#7221=ORIENTED_EDGE('',*,*,#5316,.T.);
#7222=ORIENTED_EDGE('',*,*,#5317,.F.);
#7223=ORIENTED_EDGE('',*,*,#5318,.T.);
#7224=ORIENTED_EDGE('',*,*,#5315,.T.);
#7225=ORIENTED_EDGE('',*,*,#5319,.T.);
#7226=ORIENTED_EDGE('',*,*,#5312,.F.);
#7227=ORIENTED_EDGE('',*,*,#5320,.T.);
#7228=ORIENTED_EDGE('',*,*,#5277,.T.);
#7229=ORIENTED_EDGE('',*,*,#5321,.T.);
#7230=ORIENTED_EDGE('',*,*,#5274,.F.);
#7231=ORIENTED_EDGE('',*,*,#5322,.T.);
#7232=ORIENTED_EDGE('',*,*,#5323,.F.);
#7233=ORIENTED_EDGE('',*,*,#5324,.T.);
#7234=ORIENTED_EDGE('',*,*,#5325,.F.);
#7235=ORIENTED_EDGE('',*,*,#5326,.F.);
#7236=ORIENTED_EDGE('',*,*,#5327,.T.);
#7237=ORIENTED_EDGE('',*,*,#5326,.T.);
#7238=ORIENTED_EDGE('',*,*,#5328,.T.);
#7239=ORIENTED_EDGE('',*,*,#5329,.T.);
#7240=ORIENTED_EDGE('',*,*,#5330,.T.);
#7241=ORIENTED_EDGE('',*,*,#5331,.T.);
#7242=ORIENTED_EDGE('',*,*,#5332,.T.);
#7243=ORIENTED_EDGE('',*,*,#5325,.T.);
#7244=ORIENTED_EDGE('',*,*,#5333,.F.);
#7245=ORIENTED_EDGE('',*,*,#5334,.F.);
#7246=ORIENTED_EDGE('',*,*,#5330,.F.);
#7247=ORIENTED_EDGE('',*,*,#5324,.F.);
#7248=ORIENTED_EDGE('',*,*,#5335,.F.);
#7249=ORIENTED_EDGE('',*,*,#5336,.F.);
#7250=ORIENTED_EDGE('',*,*,#5337,.F.);
#7251=ORIENTED_EDGE('',*,*,#5338,.T.);
#7252=ORIENTED_EDGE('',*,*,#5339,.T.);
#7253=ORIENTED_EDGE('',*,*,#5335,.T.);
#7254=ORIENTED_EDGE('',*,*,#5323,.T.);
#7255=ORIENTED_EDGE('',*,*,#5340,.T.);
#7256=ORIENTED_EDGE('',*,*,#5341,.T.);
#7257=ORIENTED_EDGE('',*,*,#5342,.F.);
#7258=ORIENTED_EDGE('',*,*,#5343,.F.);
#7259=ORIENTED_EDGE('',*,*,#5329,.F.);
#7260=ORIENTED_EDGE('',*,*,#5344,.F.);
#7261=ORIENTED_EDGE('',*,*,#5345,.F.);
#7262=ORIENTED_EDGE('',*,*,#5346,.F.);
#7263=ORIENTED_EDGE('',*,*,#5347,.F.);
#7264=ORIENTED_EDGE('',*,*,#5348,.F.);
#7265=ORIENTED_EDGE('',*,*,#5349,.F.);
#7266=ORIENTED_EDGE('',*,*,#5350,.F.);
#7267=ORIENTED_EDGE('',*,*,#5328,.F.);
#7268=ORIENTED_EDGE('',*,*,#5332,.F.);
#7269=ORIENTED_EDGE('',*,*,#5340,.F.);
#7270=ORIENTED_EDGE('',*,*,#5327,.F.);
#7271=ORIENTED_EDGE('',*,*,#5351,.F.);
#7272=ORIENTED_EDGE('',*,*,#5352,.F.);
#7273=ORIENTED_EDGE('',*,*,#5353,.F.);
#7274=ORIENTED_EDGE('',*,*,#5354,.F.);
#7275=ORIENTED_EDGE('',*,*,#5331,.F.);
#7276=ORIENTED_EDGE('',*,*,#5334,.T.);
#7277=ORIENTED_EDGE('',*,*,#5355,.F.);
#7278=ORIENTED_EDGE('',*,*,#5356,.T.);
#7279=ORIENTED_EDGE('',*,*,#5357,.F.);
#7280=ORIENTED_EDGE('',*,*,#5358,.F.);
#7281=ORIENTED_EDGE('',*,*,#5359,.F.);
#7282=ORIENTED_EDGE('',*,*,#5360,.F.);
#7283=ORIENTED_EDGE('',*,*,#5361,.F.);
#7284=ORIENTED_EDGE('',*,*,#5362,.T.);
#7285=ORIENTED_EDGE('',*,*,#5339,.F.);
#7286=ORIENTED_EDGE('',*,*,#5362,.F.);
#7287=ORIENTED_EDGE('',*,*,#5363,.F.);
#7288=ORIENTED_EDGE('',*,*,#5338,.F.);
#7289=ORIENTED_EDGE('',*,*,#5364,.F.);
#7290=ORIENTED_EDGE('',*,*,#5365,.T.);
#7291=ORIENTED_EDGE('',*,*,#5337,.T.);
#7292=ORIENTED_EDGE('',*,*,#5366,.T.);
#7293=ORIENTED_EDGE('',*,*,#5367,.T.);
#7294=ORIENTED_EDGE('',*,*,#5364,.T.);
#7295=ORIENTED_EDGE('',*,*,#5368,.F.);
#7296=ORIENTED_EDGE('',*,*,#5369,.F.);
#7297=ORIENTED_EDGE('',*,*,#5370,.F.);
#7298=ORIENTED_EDGE('',*,*,#5371,.F.);
#7299=ORIENTED_EDGE('',*,*,#5372,.T.);
#7300=ORIENTED_EDGE('',*,*,#5366,.F.);
#7301=ORIENTED_EDGE('',*,*,#5336,.T.);
#7302=ORIENTED_EDGE('',*,*,#5341,.F.);
#7303=ORIENTED_EDGE('',*,*,#5373,.F.);
#7304=ORIENTED_EDGE('',*,*,#5374,.F.);
#7305=ORIENTED_EDGE('',*,*,#5375,.F.);
#7306=ORIENTED_EDGE('',*,*,#5376,.T.);
#7307=ORIENTED_EDGE('',*,*,#5355,.T.);
#7308=ORIENTED_EDGE('',*,*,#5333,.T.);
#7309=ORIENTED_EDGE('',*,*,#5363,.T.);
#7310=ORIENTED_EDGE('',*,*,#5361,.T.);
#7311=ORIENTED_EDGE('',*,*,#5377,.T.);
#7312=ORIENTED_EDGE('',*,*,#5349,.T.);
#7313=ORIENTED_EDGE('',*,*,#5377,.F.);
#7314=ORIENTED_EDGE('',*,*,#5378,.T.);
#7315=ORIENTED_EDGE('',*,*,#5379,.T.);
#7316=ORIENTED_EDGE('',*,*,#5380,.T.);
#7317=ORIENTED_EDGE('',*,*,#5348,.T.);
#7318=ORIENTED_EDGE('',*,*,#5380,.F.);
#7319=ORIENTED_EDGE('',*,*,#5279,.T.);
#7320=ORIENTED_EDGE('',*,*,#5381,.T.);
#7321=ORIENTED_EDGE('',*,*,#5382,.T.);
#7322=ORIENTED_EDGE('',*,*,#5346,.T.);
#7323=ORIENTED_EDGE('',*,*,#5383,.F.);
#7324=ORIENTED_EDGE('',*,*,#5347,.T.);
#7325=ORIENTED_EDGE('',*,*,#5382,.F.);
#7326=ORIENTED_EDGE('',*,*,#5383,.T.);
#7327=ORIENTED_EDGE('',*,*,#5345,.T.);
#7328=ORIENTED_EDGE('',*,*,#5384,.T.);
#7329=ORIENTED_EDGE('',*,*,#5385,.T.);
#7330=ORIENTED_EDGE('',*,*,#5386,.T.);
#7331=ORIENTED_EDGE('',*,*,#5342,.T.);
#7332=ORIENTED_EDGE('',*,*,#5350,.T.);
#7333=ORIENTED_EDGE('',*,*,#5354,.T.);
#7334=ORIENTED_EDGE('',*,*,#5387,.T.);
#7335=ORIENTED_EDGE('',*,*,#5344,.T.);
#7336=ORIENTED_EDGE('',*,*,#5388,.T.);
#7337=ORIENTED_EDGE('',*,*,#5373,.T.);
#7338=ORIENTED_EDGE('',*,*,#5351,.T.);
#7339=ORIENTED_EDGE('',*,*,#5343,.T.);
#7340=ORIENTED_EDGE('',*,*,#5389,.F.);
#7341=ORIENTED_EDGE('',*,*,#5359,.T.);
#7342=ORIENTED_EDGE('',*,*,#5390,.T.);
#7343=ORIENTED_EDGE('',*,*,#5391,.T.);
#7344=ORIENTED_EDGE('',*,*,#5392,.T.);
#7345=ORIENTED_EDGE('',*,*,#5353,.T.);
#7346=ORIENTED_EDGE('',*,*,#5393,.T.);
#7347=ORIENTED_EDGE('',*,*,#5394,.T.);
#7348=ORIENTED_EDGE('',*,*,#5395,.T.);
#7349=ORIENTED_EDGE('',*,*,#5358,.T.);
#7350=ORIENTED_EDGE('',*,*,#5396,.T.);
#7351=ORIENTED_EDGE('',*,*,#5397,.T.);
#7352=ORIENTED_EDGE('',*,*,#5398,.T.);
#7353=ORIENTED_EDGE('',*,*,#5357,.T.);
#7354=ORIENTED_EDGE('',*,*,#5376,.F.);
#7355=ORIENTED_EDGE('',*,*,#5365,.F.);
#7356=ORIENTED_EDGE('',*,*,#5367,.F.);
#7357=ORIENTED_EDGE('',*,*,#5372,.F.);
#7358=ORIENTED_EDGE('',*,*,#5399,.F.);
#7359=ORIENTED_EDGE('',*,*,#5400,.F.);
#7360=ORIENTED_EDGE('',*,*,#5396,.F.);
#7361=ORIENTED_EDGE('',*,*,#5356,.F.);
#7362=ORIENTED_EDGE('',*,*,#5401,.T.);
#7363=ORIENTED_EDGE('',*,*,#5317,.T.);
#7364=ORIENTED_EDGE('',*,*,#5402,.T.);
#7365=ORIENTED_EDGE('',*,*,#5256,.T.);
#7366=ORIENTED_EDGE('',*,*,#5403,.T.);
#7367=ORIENTED_EDGE('',*,*,#5404,.T.);
#7368=ORIENTED_EDGE('',*,*,#5360,.T.);
#7369=ORIENTED_EDGE('',*,*,#5389,.T.);
#7370=ORIENTED_EDGE('',*,*,#5352,.T.);
#7371=ORIENTED_EDGE('',*,*,#5404,.F.);
#7372=ORIENTED_EDGE('',*,*,#5405,.F.);
#7373=ORIENTED_EDGE('',*,*,#5374,.T.);
#7374=ORIENTED_EDGE('',*,*,#5406,.T.);
#7375=ORIENTED_EDGE('',*,*,#5407,.T.);
#7376=ORIENTED_EDGE('',*,*,#5408,.T.);
#7377=ORIENTED_EDGE('',*,*,#5369,.T.);
#7378=ORIENTED_EDGE('',*,*,#5399,.T.);
#7379=ORIENTED_EDGE('',*,*,#5371,.T.);
#7380=ORIENTED_EDGE('',*,*,#5409,.T.);
#7381=ORIENTED_EDGE('',*,*,#5410,.T.);
#7382=ORIENTED_EDGE('',*,*,#5411,.T.);
#7383=ORIENTED_EDGE('',*,*,#5412,.T.);
#7384=ORIENTED_EDGE('',*,*,#5413,.T.);
#7385=ORIENTED_EDGE('',*,*,#5370,.T.);
#7386=ORIENTED_EDGE('',*,*,#5414,.T.);
#7387=ORIENTED_EDGE('',*,*,#5415,.T.);
#7388=ORIENTED_EDGE('',*,*,#5375,.T.);
#7389=ORIENTED_EDGE('',*,*,#5405,.T.);
#7390=ORIENTED_EDGE('',*,*,#5368,.T.);
#7391=ORIENTED_EDGE('',*,*,#5415,.F.);
#7392=ORIENTED_EDGE('',*,*,#5416,.T.);
#7393=ORIENTED_EDGE('',*,*,#5417,.T.);
#7394=ORIENTED_EDGE('',*,*,#5418,.T.);
#7395=ORIENTED_EDGE('',*,*,#5419,.T.);
#7396=ORIENTED_EDGE('',*,*,#5420,.T.);
#7397=ORIENTED_EDGE('',*,*,#5421,.T.);
#7398=ORIENTED_EDGE('',*,*,#5422,.T.);
#7399=ORIENTED_EDGE('',*,*,#5423,.T.);
#7400=ORIENTED_EDGE('',*,*,#5424,.T.);
#7401=ORIENTED_EDGE('',*,*,#5425,.T.);
#7402=ORIENTED_EDGE('',*,*,#5426,.F.);
#7403=ORIENTED_EDGE('',*,*,#5427,.T.);
#7404=ORIENTED_EDGE('',*,*,#5428,.T.);
#7405=ORIENTED_EDGE('',*,*,#5429,.T.);
#7406=ORIENTED_EDGE('',*,*,#5430,.T.);
#7407=ORIENTED_EDGE('',*,*,#5431,.T.);
#7408=ORIENTED_EDGE('',*,*,#5432,.T.);
#7409=ORIENTED_EDGE('',*,*,#5433,.T.);
#7410=ORIENTED_EDGE('',*,*,#5434,.T.);
#7411=ORIENTED_EDGE('',*,*,#5435,.T.);
#7412=ORIENTED_EDGE('',*,*,#5436,.T.);
#7413=ORIENTED_EDGE('',*,*,#5437,.T.);
#7414=ORIENTED_EDGE('',*,*,#5378,.F.);
#7415=ORIENTED_EDGE('',*,*,#5438,.T.);
#7416=ORIENTED_EDGE('',*,*,#5439,.T.);
#7417=ORIENTED_EDGE('',*,*,#5440,.T.);
#7418=ORIENTED_EDGE('',*,*,#5379,.F.);
#7419=ORIENTED_EDGE('',*,*,#5441,.T.);
#7420=ORIENTED_EDGE('',*,*,#5208,.T.);
#7421=ORIENTED_EDGE('',*,*,#5442,.T.);
#7422=ORIENTED_EDGE('',*,*,#5381,.F.);
#7423=ORIENTED_EDGE('',*,*,#5443,.T.);
#7424=ORIENTED_EDGE('',*,*,#5406,.F.);
#7425=ORIENTED_EDGE('',*,*,#5388,.F.);
#7426=ORIENTED_EDGE('',*,*,#5386,.F.);
#7427=ORIENTED_EDGE('',*,*,#5385,.F.);
#7428=ORIENTED_EDGE('',*,*,#5391,.F.);
#7429=ORIENTED_EDGE('',*,*,#5444,.F.);
#7430=ORIENTED_EDGE('',*,*,#5407,.F.);
#7431=ORIENTED_EDGE('',*,*,#5392,.F.);
#7432=ORIENTED_EDGE('',*,*,#5384,.F.);
#7433=ORIENTED_EDGE('',*,*,#5387,.F.);
#7434=ORIENTED_EDGE('',*,*,#5445,.F.);
#7435=ORIENTED_EDGE('',*,*,#5390,.F.);
#7436=ORIENTED_EDGE('',*,*,#5395,.F.);
#7437=ORIENTED_EDGE('',*,*,#5446,.F.);
#7438=ORIENTED_EDGE('',*,*,#5394,.F.);
#7439=ORIENTED_EDGE('',*,*,#5447,.F.);
#7440=ORIENTED_EDGE('',*,*,#5412,.F.);
#7441=ORIENTED_EDGE('',*,*,#5448,.F.);
#7442=ORIENTED_EDGE('',*,*,#5449,.F.);
#7443=ORIENTED_EDGE('',*,*,#5393,.F.);
#7444=ORIENTED_EDGE('',*,*,#5398,.F.);
#7445=ORIENTED_EDGE('',*,*,#5450,.F.);
#7446=ORIENTED_EDGE('',*,*,#5410,.F.);
#7447=ORIENTED_EDGE('',*,*,#5451,.F.);
#7448=ORIENTED_EDGE('',*,*,#5397,.F.);
#7449=ORIENTED_EDGE('',*,*,#5400,.T.);
#7450=ORIENTED_EDGE('',*,*,#5254,.T.);
#7451=ORIENTED_EDGE('',*,*,#5452,.T.);
#7452=ORIENTED_EDGE('',*,*,#5453,.T.);
#7453=ORIENTED_EDGE('',*,*,#5250,.F.);
#7454=ORIENTED_EDGE('',*,*,#5454,.F.);
#7455=ORIENTED_EDGE('',*,*,#5455,.F.);
#7456=ORIENTED_EDGE('',*,*,#5212,.F.);
#7457=ORIENTED_EDGE('',*,*,#5211,.F.);
#7458=ORIENTED_EDGE('',*,*,#5217,.F.);
#7459=ORIENTED_EDGE('',*,*,#5216,.F.);
#7460=ORIENTED_EDGE('',*,*,#5221,.F.);
#7461=ORIENTED_EDGE('',*,*,#5224,.F.);
#7462=ORIENTED_EDGE('',*,*,#5227,.F.);
#7463=ORIENTED_EDGE('',*,*,#5231,.F.);
#7464=ORIENTED_EDGE('',*,*,#5230,.F.);
#7465=ORIENTED_EDGE('',*,*,#5235,.F.);
#7466=ORIENTED_EDGE('',*,*,#5238,.F.);
#7467=ORIENTED_EDGE('',*,*,#5241,.F.);
#7468=ORIENTED_EDGE('',*,*,#5244,.F.);
#7469=ORIENTED_EDGE('',*,*,#5247,.F.);
#7470=ORIENTED_EDGE('',*,*,#5252,.F.);
#7471=ORIENTED_EDGE('',*,*,#5251,.F.);
#7472=ORIENTED_EDGE('',*,*,#5453,.F.);
#7473=ORIENTED_EDGE('',*,*,#5452,.F.);
#7474=ORIENTED_EDGE('',*,*,#5257,.F.);
#7475=ORIENTED_EDGE('',*,*,#5402,.F.);
#7476=ORIENTED_EDGE('',*,*,#5316,.F.);
#7477=ORIENTED_EDGE('',*,*,#5320,.F.);
#7478=ORIENTED_EDGE('',*,*,#5314,.F.);
#7479=ORIENTED_EDGE('',*,*,#5311,.F.);
#7480=ORIENTED_EDGE('',*,*,#5308,.F.);
#7481=ORIENTED_EDGE('',*,*,#5305,.F.);
#7482=ORIENTED_EDGE('',*,*,#5302,.F.);
#7483=ORIENTED_EDGE('',*,*,#5299,.F.);
#7484=ORIENTED_EDGE('',*,*,#5296,.F.);
#7485=ORIENTED_EDGE('',*,*,#5293,.F.);
#7486=ORIENTED_EDGE('',*,*,#5290,.F.);
#7487=ORIENTED_EDGE('',*,*,#5287,.F.);
#7488=ORIENTED_EDGE('',*,*,#5284,.F.);
#7489=ORIENTED_EDGE('',*,*,#5456,.F.);
#7490=ORIENTED_EDGE('',*,*,#5282,.F.);
#7491=ORIENTED_EDGE('',*,*,#5286,.F.);
#7492=ORIENTED_EDGE('',*,*,#5289,.F.);
#7493=ORIENTED_EDGE('',*,*,#5292,.F.);
#7494=ORIENTED_EDGE('',*,*,#5295,.F.);
#7495=ORIENTED_EDGE('',*,*,#5298,.F.);
#7496=ORIENTED_EDGE('',*,*,#5301,.F.);
#7497=ORIENTED_EDGE('',*,*,#5304,.F.);
#7498=ORIENTED_EDGE('',*,*,#5307,.F.);
#7499=ORIENTED_EDGE('',*,*,#5310,.F.);
#7500=ORIENTED_EDGE('',*,*,#5313,.F.);
#7501=ORIENTED_EDGE('',*,*,#5319,.F.);
#7502=ORIENTED_EDGE('',*,*,#5318,.F.);
#7503=ORIENTED_EDGE('',*,*,#5401,.F.);
#7504=ORIENTED_EDGE('',*,*,#5255,.T.);
#7505=ORIENTED_EDGE('',*,*,#5454,.T.);
#7506=ORIENTED_EDGE('',*,*,#5253,.T.);
#7507=ORIENTED_EDGE('',*,*,#5249,.T.);
#7508=ORIENTED_EDGE('',*,*,#5248,.T.);
#7509=ORIENTED_EDGE('',*,*,#5245,.T.);
#7510=ORIENTED_EDGE('',*,*,#5242,.T.);
#7511=ORIENTED_EDGE('',*,*,#5239,.T.);
#7512=ORIENTED_EDGE('',*,*,#5236,.T.);
#7513=ORIENTED_EDGE('',*,*,#5233,.T.);
#7514=ORIENTED_EDGE('',*,*,#5232,.T.);
#7515=ORIENTED_EDGE('',*,*,#5228,.T.);
#7516=ORIENTED_EDGE('',*,*,#5225,.T.);
#7517=ORIENTED_EDGE('',*,*,#5222,.T.);
#7518=ORIENTED_EDGE('',*,*,#5219,.T.);
#7519=ORIENTED_EDGE('',*,*,#5218,.T.);
#7520=ORIENTED_EDGE('',*,*,#5214,.T.);
#7521=ORIENTED_EDGE('',*,*,#5414,.F.);
#7522=ORIENTED_EDGE('',*,*,#5457,.T.);
#7523=ORIENTED_EDGE('',*,*,#5403,.F.);
#7524=ORIENTED_EDGE('',*,*,#5457,.F.);
#7525=ORIENTED_EDGE('',*,*,#5458,.T.);
#7526=ORIENTED_EDGE('',*,*,#5459,.T.);
#7527=ORIENTED_EDGE('',*,*,#5460,.T.);
#7528=ORIENTED_EDGE('',*,*,#5461,.T.);
#7529=ORIENTED_EDGE('',*,*,#5462,.T.);
#7530=ORIENTED_EDGE('',*,*,#5182,.T.);
#7531=ORIENTED_EDGE('',*,*,#5463,.T.);
#7532=ORIENTED_EDGE('',*,*,#5464,.T.);
#7533=ORIENTED_EDGE('',*,*,#5465,.T.);
#7534=ORIENTED_EDGE('',*,*,#5466,.T.);
#7535=ORIENTED_EDGE('',*,*,#5467,.T.);
#7536=ORIENTED_EDGE('',*,*,#5468,.T.);
#7537=ORIENTED_EDGE('',*,*,#5469,.T.);
#7538=ORIENTED_EDGE('',*,*,#5470,.T.);
#7539=ORIENTED_EDGE('',*,*,#5471,.T.);
#7540=ORIENTED_EDGE('',*,*,#5472,.T.);
#7541=ORIENTED_EDGE('',*,*,#5473,.T.);
#7542=ORIENTED_EDGE('',*,*,#5260,.T.);
#7543=ORIENTED_EDGE('',*,*,#5474,.T.);
#7544=ORIENTED_EDGE('',*,*,#5475,.T.);
#7545=ORIENTED_EDGE('',*,*,#5476,.T.);
#7546=ORIENTED_EDGE('',*,*,#5477,.T.);
#7547=ORIENTED_EDGE('',*,*,#5478,.T.);
#7548=ORIENTED_EDGE('',*,*,#5479,.T.);
#7549=ORIENTED_EDGE('',*,*,#5480,.T.);
#7550=ORIENTED_EDGE('',*,*,#5411,.F.);
#7551=ORIENTED_EDGE('',*,*,#5408,.F.);
#7552=ORIENTED_EDGE('',*,*,#5481,.F.);
#7553=ORIENTED_EDGE('',*,*,#5482,.F.);
#7554=ORIENTED_EDGE('',*,*,#5409,.F.);
#7555=ORIENTED_EDGE('',*,*,#5413,.F.);
#7556=ORIENTED_EDGE('',*,*,#5483,.F.);
#7557=ORIENTED_EDGE('',*,*,#5425,.F.);
#7558=ORIENTED_EDGE('',*,*,#5424,.F.);
#7559=ORIENTED_EDGE('',*,*,#5423,.F.);
#7560=ORIENTED_EDGE('',*,*,#5422,.F.);
#7561=ORIENTED_EDGE('',*,*,#5421,.F.);
#7562=ORIENTED_EDGE('',*,*,#5420,.F.);
#7563=ORIENTED_EDGE('',*,*,#5419,.F.);
#7564=ORIENTED_EDGE('',*,*,#5418,.F.);
#7565=ORIENTED_EDGE('',*,*,#5417,.F.);
#7566=ORIENTED_EDGE('',*,*,#5416,.F.);
#7567=ORIENTED_EDGE('',*,*,#5438,.F.);
#7568=ORIENTED_EDGE('',*,*,#5440,.F.);
#7569=ORIENTED_EDGE('',*,*,#5484,.T.);
#7570=ORIENTED_EDGE('',*,*,#5485,.T.);
#7571=ORIENTED_EDGE('',*,*,#5486,.T.);
#7572=ORIENTED_EDGE('',*,*,#5487,.T.);
#7573=ORIENTED_EDGE('',*,*,#5488,.T.);
#7574=ORIENTED_EDGE('',*,*,#5489,.T.);
#7575=ORIENTED_EDGE('',*,*,#5490,.T.);
#7576=ORIENTED_EDGE('',*,*,#5491,.T.);
#7577=ORIENTED_EDGE('',*,*,#5492,.T.);
#7578=ORIENTED_EDGE('',*,*,#5493,.T.);
#7579=ORIENTED_EDGE('',*,*,#5494,.T.);
#7580=ORIENTED_EDGE('',*,*,#5495,.F.);
#7581=ORIENTED_EDGE('',*,*,#5496,.F.);
#7582=ORIENTED_EDGE('',*,*,#5497,.F.);
#7583=ORIENTED_EDGE('',*,*,#5498,.F.);
#7584=ORIENTED_EDGE('',*,*,#5499,.F.);
#7585=ORIENTED_EDGE('',*,*,#5500,.F.);
#7586=ORIENTED_EDGE('',*,*,#5441,.F.);
#7587=ORIENTED_EDGE('',*,*,#5437,.F.);
#7588=ORIENTED_EDGE('',*,*,#5436,.F.);
#7589=ORIENTED_EDGE('',*,*,#5435,.F.);
#7590=ORIENTED_EDGE('',*,*,#5434,.F.);
#7591=ORIENTED_EDGE('',*,*,#5433,.F.);
#7592=ORIENTED_EDGE('',*,*,#5432,.F.);
#7593=ORIENTED_EDGE('',*,*,#5431,.F.);
#7594=ORIENTED_EDGE('',*,*,#5430,.F.);
#7595=ORIENTED_EDGE('',*,*,#5429,.F.);
#7596=ORIENTED_EDGE('',*,*,#5428,.F.);
#7597=ORIENTED_EDGE('',*,*,#5427,.F.);
#7598=ORIENTED_EDGE('',*,*,#5501,.T.);
#7599=ORIENTED_EDGE('',*,*,#5502,.T.);
#7600=ORIENTED_EDGE('',*,*,#5448,.T.);
#7601=ORIENTED_EDGE('',*,*,#5502,.F.);
#7602=ORIENTED_EDGE('',*,*,#5503,.T.);
#7603=ORIENTED_EDGE('',*,*,#5426,.T.);
#7604=ORIENTED_EDGE('',*,*,#5500,.T.);
#7605=ORIENTED_EDGE('',*,*,#5499,.T.);
#7606=ORIENTED_EDGE('',*,*,#5498,.T.);
#7607=ORIENTED_EDGE('',*,*,#5497,.T.);
#7608=ORIENTED_EDGE('',*,*,#5496,.T.);
#7609=ORIENTED_EDGE('',*,*,#5504,.F.);
#7610=ORIENTED_EDGE('',*,*,#5494,.F.);
#7611=ORIENTED_EDGE('',*,*,#5493,.F.);
#7612=ORIENTED_EDGE('',*,*,#5492,.F.);
#7613=ORIENTED_EDGE('',*,*,#5491,.F.);
#7614=ORIENTED_EDGE('',*,*,#5490,.F.);
#7615=ORIENTED_EDGE('',*,*,#5489,.F.);
#7616=ORIENTED_EDGE('',*,*,#5488,.F.);
#7617=ORIENTED_EDGE('',*,*,#5487,.F.);
#7618=ORIENTED_EDGE('',*,*,#5486,.F.);
#7619=ORIENTED_EDGE('',*,*,#5485,.F.);
#7620=ORIENTED_EDGE('',*,*,#5484,.F.);
#7621=ORIENTED_EDGE('',*,*,#5439,.F.);
#7622=ORIENTED_EDGE('',*,*,#5462,.F.);
#7623=ORIENTED_EDGE('',*,*,#5505,.T.);
#7624=ORIENTED_EDGE('',*,*,#5474,.F.);
#7625=ORIENTED_EDGE('',*,*,#5259,.F.);
#7626=ORIENTED_EDGE('',*,*,#5263,.F.);
#7627=ORIENTED_EDGE('',*,*,#5266,.F.);
#7628=ORIENTED_EDGE('',*,*,#5269,.F.);
#7629=ORIENTED_EDGE('',*,*,#5272,.F.);
#7630=ORIENTED_EDGE('',*,*,#5275,.F.);
#7631=ORIENTED_EDGE('',*,*,#5321,.F.);
#7632=ORIENTED_EDGE('',*,*,#5280,.F.);
#7633=ORIENTED_EDGE('',*,*,#5442,.F.);
#7634=ORIENTED_EDGE('',*,*,#5207,.T.);
#7635=ORIENTED_EDGE('',*,*,#5506,.T.);
#7636=ORIENTED_EDGE('',*,*,#5205,.T.);
#7637=ORIENTED_EDGE('',*,*,#5201,.T.);
#7638=ORIENTED_EDGE('',*,*,#5198,.T.);
#7639=ORIENTED_EDGE('',*,*,#5195,.T.);
#7640=ORIENTED_EDGE('',*,*,#5192,.T.);
#7641=ORIENTED_EDGE('',*,*,#5191,.T.);
#7642=ORIENTED_EDGE('',*,*,#5188,.T.);
#7643=ORIENTED_EDGE('',*,*,#5184,.T.);
#7644=ORIENTED_EDGE('',*,*,#5183,.T.);
#7645=ORIENTED_EDGE('',*,*,#5463,.F.);
#7646=ORIENTED_EDGE('',*,*,#5181,.F.);
#7647=ORIENTED_EDGE('',*,*,#5180,.F.);
#7648=ORIENTED_EDGE('',*,*,#5187,.F.);
#7649=ORIENTED_EDGE('',*,*,#5186,.F.);
#7650=ORIENTED_EDGE('',*,*,#5190,.F.);
#7651=ORIENTED_EDGE('',*,*,#5194,.F.);
#7652=ORIENTED_EDGE('',*,*,#5197,.F.);
#7653=ORIENTED_EDGE('',*,*,#5200,.F.);
#7654=ORIENTED_EDGE('',*,*,#5204,.F.);
#7655=ORIENTED_EDGE('',*,*,#5203,.F.);
#7656=ORIENTED_EDGE('',*,*,#5507,.F.);
#7657=ORIENTED_EDGE('',*,*,#5508,.F.);
#7658=ORIENTED_EDGE('',*,*,#5209,.F.);
#7659=ORIENTED_EDGE('',*,*,#5443,.F.);
#7660=ORIENTED_EDGE('',*,*,#5278,.F.);
#7661=ORIENTED_EDGE('',*,*,#5322,.F.);
#7662=ORIENTED_EDGE('',*,*,#5276,.F.);
#7663=ORIENTED_EDGE('',*,*,#5273,.F.);
#7664=ORIENTED_EDGE('',*,*,#5270,.F.);
#7665=ORIENTED_EDGE('',*,*,#5267,.F.);
#7666=ORIENTED_EDGE('',*,*,#5264,.F.);
#7667=ORIENTED_EDGE('',*,*,#5261,.F.);
#7668=ORIENTED_EDGE('',*,*,#5473,.F.);
#7669=ORIENTED_EDGE('',*,*,#5509,.F.);
#7670=ORIENTED_EDGE('',*,*,#5206,.T.);
#7671=ORIENTED_EDGE('',*,*,#5508,.T.);
#7672=ORIENTED_EDGE('',*,*,#5507,.T.);
#7673=ORIENTED_EDGE('',*,*,#5202,.F.);
#7674=ORIENTED_EDGE('',*,*,#5506,.F.);
#7675=ORIENTED_EDGE('',*,*,#5445,.T.);
#7676=ORIENTED_EDGE('',*,*,#5446,.T.);
#7677=ORIENTED_EDGE('',*,*,#5481,.T.);
#7678=ORIENTED_EDGE('',*,*,#5444,.T.);
#7679=ORIENTED_EDGE('',*,*,#5510,.T.);
#7680=ORIENTED_EDGE('',*,*,#5511,.T.);
#7681=ORIENTED_EDGE('',*,*,#5449,.T.);
#7682=ORIENTED_EDGE('',*,*,#5511,.F.);
#7683=ORIENTED_EDGE('',*,*,#5512,.T.);
#7684=ORIENTED_EDGE('',*,*,#5283,.T.);
#7685=ORIENTED_EDGE('',*,*,#5482,.T.);
#7686=ORIENTED_EDGE('',*,*,#5447,.T.);
#7687=ORIENTED_EDGE('',*,*,#5450,.T.);
#7688=ORIENTED_EDGE('',*,*,#5451,.T.);
#7689=ORIENTED_EDGE('',*,*,#5510,.F.);
#7690=ORIENTED_EDGE('',*,*,#5456,.T.);
#7691=ORIENTED_EDGE('',*,*,#5213,.T.);
#7692=ORIENTED_EDGE('',*,*,#5455,.T.);
#7693=ORIENTED_EDGE('',*,*,#5512,.F.);
#7694=ORIENTED_EDGE('',*,*,#5480,.F.);
#7695=ORIENTED_EDGE('',*,*,#5513,.F.);
#7696=ORIENTED_EDGE('',*,*,#5514,.F.);
#7697=ORIENTED_EDGE('',*,*,#5479,.F.);
#7698=ORIENTED_EDGE('',*,*,#5515,.T.);
#7699=ORIENTED_EDGE('',*,*,#5513,.T.);
#7700=ORIENTED_EDGE('',*,*,#5458,.F.);
#7701=ORIENTED_EDGE('',*,*,#5514,.T.);
#7702=ORIENTED_EDGE('',*,*,#5515,.F.);
#7703=ORIENTED_EDGE('',*,*,#5478,.F.);
#7704=ORIENTED_EDGE('',*,*,#5516,.F.);
#7705=ORIENTED_EDGE('',*,*,#5516,.T.);
#7706=ORIENTED_EDGE('',*,*,#5477,.F.);
#7707=ORIENTED_EDGE('',*,*,#5517,.T.);
#7708=ORIENTED_EDGE('',*,*,#5459,.F.);
#7709=ORIENTED_EDGE('',*,*,#5476,.F.);
#7710=ORIENTED_EDGE('',*,*,#5518,.F.);
#7711=ORIENTED_EDGE('',*,*,#5460,.F.);
#7712=ORIENTED_EDGE('',*,*,#5517,.F.);
#7713=ORIENTED_EDGE('',*,*,#5461,.F.);
#7714=ORIENTED_EDGE('',*,*,#5518,.T.);
#7715=ORIENTED_EDGE('',*,*,#5475,.F.);
#7716=ORIENTED_EDGE('',*,*,#5505,.F.);
#7717=ORIENTED_EDGE('',*,*,#5519,.T.);
#7718=ORIENTED_EDGE('',*,*,#5464,.F.);
#7719=ORIENTED_EDGE('',*,*,#5509,.T.);
#7720=ORIENTED_EDGE('',*,*,#5472,.F.);
#7721=ORIENTED_EDGE('',*,*,#5471,.F.);
#7722=ORIENTED_EDGE('',*,*,#5520,.T.);
#7723=ORIENTED_EDGE('',*,*,#5465,.F.);
#7724=ORIENTED_EDGE('',*,*,#5519,.F.);
#7725=ORIENTED_EDGE('',*,*,#5470,.F.);
#7726=ORIENTED_EDGE('',*,*,#5521,.T.);
#7727=ORIENTED_EDGE('',*,*,#5466,.F.);
#7728=ORIENTED_EDGE('',*,*,#5520,.F.);
#7729=ORIENTED_EDGE('',*,*,#5469,.F.);
#7730=ORIENTED_EDGE('',*,*,#5522,.F.);
#7731=ORIENTED_EDGE('',*,*,#5467,.F.);
#7732=ORIENTED_EDGE('',*,*,#5521,.F.);
#7733=ORIENTED_EDGE('',*,*,#5468,.F.);
#7734=ORIENTED_EDGE('',*,*,#5522,.T.);
#7735=ORIENTED_EDGE('',*,*,#5501,.F.);
#7736=ORIENTED_EDGE('',*,*,#5483,.T.);
#7737=ORIENTED_EDGE('',*,*,#5504,.T.);
#7738=ORIENTED_EDGE('',*,*,#5495,.T.);
#7739=ORIENTED_EDGE('',*,*,#5503,.F.);
#7740=ORIENTED_EDGE('',*,*,#5523,.F.);
#7741=ORIENTED_EDGE('',*,*,#5524,.T.);
#7742=ORIENTED_EDGE('',*,*,#5525,.T.);
#7743=ORIENTED_EDGE('',*,*,#5526,.T.);
#7744=ORIENTED_EDGE('',*,*,#5524,.F.);
#7745=ORIENTED_EDGE('',*,*,#5526,.F.);
#7746=ORIENTED_EDGE('',*,*,#5527,.T.);
#7747=ORIENTED_EDGE('',*,*,#5528,.T.);
#7748=ORIENTED_EDGE('',*,*,#5529,.T.);
#7749=ORIENTED_EDGE('',*,*,#5527,.F.);
#7750=ORIENTED_EDGE('',*,*,#5525,.F.);
#7751=ORIENTED_EDGE('',*,*,#5529,.F.);
#7752=ORIENTED_EDGE('',*,*,#5530,.T.);
#7753=ORIENTED_EDGE('',*,*,#5531,.T.);
#7754=ORIENTED_EDGE('',*,*,#5530,.F.);
#7755=ORIENTED_EDGE('',*,*,#5528,.F.);
#7756=ORIENTED_EDGE('',*,*,#5523,.T.);
#7757=ORIENTED_EDGE('',*,*,#5531,.F.);
#7758=ORIENTED_EDGE('',*,*,#5532,.T.);
#7759=ORIENTED_EDGE('',*,*,#5533,.T.);
#7760=ORIENTED_EDGE('',*,*,#5534,.T.);
#7761=ORIENTED_EDGE('',*,*,#5535,.T.);
#7762=ORIENTED_EDGE('',*,*,#5536,.T.);
#7763=ORIENTED_EDGE('',*,*,#5537,.T.);
#7764=ORIENTED_EDGE('',*,*,#5538,.T.);
#7765=ORIENTED_EDGE('',*,*,#5539,.T.);
#7766=ORIENTED_EDGE('',*,*,#5540,.T.);
#7767=ORIENTED_EDGE('',*,*,#5541,.T.);
#7768=ORIENTED_EDGE('',*,*,#5542,.F.);
#7769=ORIENTED_EDGE('',*,*,#5543,.F.);
#7770=ORIENTED_EDGE('',*,*,#5544,.F.);
#7771=ORIENTED_EDGE('',*,*,#5545,.F.);
#7772=ORIENTED_EDGE('',*,*,#5546,.F.);
#7773=ORIENTED_EDGE('',*,*,#5547,.F.);
#7774=ORIENTED_EDGE('',*,*,#5548,.F.);
#7775=ORIENTED_EDGE('',*,*,#5549,.F.);
#7776=ORIENTED_EDGE('',*,*,#5550,.F.);
#7777=ORIENTED_EDGE('',*,*,#5551,.F.);
#7778=ORIENTED_EDGE('',*,*,#5552,.F.);
#7779=ORIENTED_EDGE('',*,*,#5553,.F.);
#7780=ORIENTED_EDGE('',*,*,#5554,.F.);
#7781=ORIENTED_EDGE('',*,*,#5555,.T.);
#7782=ORIENTED_EDGE('',*,*,#5556,.T.);
#7783=ORIENTED_EDGE('',*,*,#5557,.T.);
#7784=ORIENTED_EDGE('',*,*,#5558,.T.);
#7785=ORIENTED_EDGE('',*,*,#5559,.T.);
#7786=ORIENTED_EDGE('',*,*,#5560,.T.);
#7787=ORIENTED_EDGE('',*,*,#5561,.T.);
#7788=ORIENTED_EDGE('',*,*,#5562,.T.);
#7789=ORIENTED_EDGE('',*,*,#5563,.T.);
#7790=ORIENTED_EDGE('',*,*,#5564,.T.);
#7791=ORIENTED_EDGE('',*,*,#5565,.T.);
#7792=ORIENTED_EDGE('',*,*,#5566,.T.);
#7793=ORIENTED_EDGE('',*,*,#5567,.T.);
#7794=ORIENTED_EDGE('',*,*,#5568,.T.);
#7795=ORIENTED_EDGE('',*,*,#5569,.T.);
#7796=ORIENTED_EDGE('',*,*,#5570,.T.);
#7797=ORIENTED_EDGE('',*,*,#5571,.T.);
#7798=ORIENTED_EDGE('',*,*,#5572,.F.);
#7799=ORIENTED_EDGE('',*,*,#5573,.T.);
#7800=ORIENTED_EDGE('',*,*,#5574,.T.);
#7801=ORIENTED_EDGE('',*,*,#5575,.T.);
#7802=ORIENTED_EDGE('',*,*,#5575,.F.);
#7803=ORIENTED_EDGE('',*,*,#5576,.T.);
#7804=ORIENTED_EDGE('',*,*,#5577,.T.);
#7805=ORIENTED_EDGE('',*,*,#5578,.T.);
#7806=ORIENTED_EDGE('',*,*,#5579,.T.);
#7807=ORIENTED_EDGE('',*,*,#5580,.T.);
#7808=ORIENTED_EDGE('',*,*,#5581,.F.);
#7809=ORIENTED_EDGE('',*,*,#5582,.F.);
#7810=ORIENTED_EDGE('',*,*,#5583,.F.);
#7811=ORIENTED_EDGE('',*,*,#5584,.F.);
#7812=ORIENTED_EDGE('',*,*,#5585,.F.);
#7813=ORIENTED_EDGE('',*,*,#5586,.F.);
#7814=ORIENTED_EDGE('',*,*,#5587,.F.);
#7815=ORIENTED_EDGE('',*,*,#5588,.F.);
#7816=ORIENTED_EDGE('',*,*,#5589,.T.);
#7817=ORIENTED_EDGE('',*,*,#5590,.T.);
#7818=ORIENTED_EDGE('',*,*,#5591,.T.);
#7819=ORIENTED_EDGE('',*,*,#5592,.T.);
#7820=ORIENTED_EDGE('',*,*,#5593,.F.);
#7821=ORIENTED_EDGE('',*,*,#5594,.T.);
#7822=ORIENTED_EDGE('',*,*,#5595,.T.);
#7823=ORIENTED_EDGE('',*,*,#5596,.T.);
#7824=ORIENTED_EDGE('',*,*,#5597,.T.);
#7825=ORIENTED_EDGE('',*,*,#5598,.T.);
#7826=ORIENTED_EDGE('',*,*,#5599,.T.);
#7827=ORIENTED_EDGE('',*,*,#5600,.F.);
#7828=ORIENTED_EDGE('',*,*,#5601,.T.);
#7829=ORIENTED_EDGE('',*,*,#5602,.T.);
#7830=ORIENTED_EDGE('',*,*,#5603,.T.);
#7831=ORIENTED_EDGE('',*,*,#5604,.T.);
#7832=ORIENTED_EDGE('',*,*,#5605,.T.);
#7833=ORIENTED_EDGE('',*,*,#5606,.T.);
#7834=ORIENTED_EDGE('',*,*,#5605,.F.);
#7835=ORIENTED_EDGE('',*,*,#5607,.F.);
#7836=ORIENTED_EDGE('',*,*,#5608,.T.);
#7837=ORIENTED_EDGE('',*,*,#5604,.F.);
#7838=ORIENTED_EDGE('',*,*,#5608,.F.);
#7839=ORIENTED_EDGE('',*,*,#5609,.F.);
#7840=ORIENTED_EDGE('',*,*,#5606,.F.);
#7841=ORIENTED_EDGE('',*,*,#5610,.T.);
#7842=ORIENTED_EDGE('',*,*,#5611,.T.);
#7843=ORIENTED_EDGE('',*,*,#5612,.T.);
#7844=ORIENTED_EDGE('',*,*,#5611,.F.);
#7845=ORIENTED_EDGE('',*,*,#5613,.F.);
#7846=ORIENTED_EDGE('',*,*,#5612,.F.);
#7847=ORIENTED_EDGE('',*,*,#5610,.F.);
#7848=ORIENTED_EDGE('',*,*,#5614,.T.);
#7849=ORIENTED_EDGE('',*,*,#5615,.T.);
#7850=ORIENTED_EDGE('',*,*,#5614,.F.);
#7851=ORIENTED_EDGE('',*,*,#5607,.T.);
#7852=ORIENTED_EDGE('',*,*,#5616,.T.);
#7853=ORIENTED_EDGE('',*,*,#5615,.F.);
#7854=ORIENTED_EDGE('',*,*,#5616,.F.);
#7855=ORIENTED_EDGE('',*,*,#5617,.T.);
#7856=ORIENTED_EDGE('',*,*,#5618,.T.);
#7857=ORIENTED_EDGE('',*,*,#5613,.T.);
#7858=ORIENTED_EDGE('',*,*,#5618,.F.);
#7859=ORIENTED_EDGE('',*,*,#5617,.F.);
#7860=ORIENTED_EDGE('',*,*,#5619,.T.);
#7861=ORIENTED_EDGE('',*,*,#5620,.F.);
#7862=ORIENTED_EDGE('',*,*,#5619,.F.);
#7863=ORIENTED_EDGE('',*,*,#5621,.F.);
#7864=ORIENTED_EDGE('',*,*,#5622,.T.);
#7865=ORIENTED_EDGE('',*,*,#5542,.T.);
#7866=ORIENTED_EDGE('',*,*,#5623,.T.);
#7867=ORIENTED_EDGE('',*,*,#5624,.F.);
#7868=ORIENTED_EDGE('',*,*,#5622,.F.);
#7869=ORIENTED_EDGE('',*,*,#5625,.F.);
#7870=ORIENTED_EDGE('',*,*,#5571,.F.);
#7871=ORIENTED_EDGE('',*,*,#5570,.F.);
#7872=ORIENTED_EDGE('',*,*,#5569,.F.);
#7873=ORIENTED_EDGE('',*,*,#5568,.F.);
#7874=ORIENTED_EDGE('',*,*,#5567,.F.);
#7875=ORIENTED_EDGE('',*,*,#5566,.F.);
#7876=ORIENTED_EDGE('',*,*,#5565,.F.);
#7877=ORIENTED_EDGE('',*,*,#5564,.F.);
#7878=ORIENTED_EDGE('',*,*,#5563,.F.);
#7879=ORIENTED_EDGE('',*,*,#5562,.F.);
#7880=ORIENTED_EDGE('',*,*,#5561,.F.);
#7881=ORIENTED_EDGE('',*,*,#5626,.F.);
#7882=ORIENTED_EDGE('',*,*,#5553,.T.);
#7883=ORIENTED_EDGE('',*,*,#5552,.T.);
#7884=ORIENTED_EDGE('',*,*,#5551,.T.);
#7885=ORIENTED_EDGE('',*,*,#5550,.T.);
#7886=ORIENTED_EDGE('',*,*,#5549,.T.);
#7887=ORIENTED_EDGE('',*,*,#5548,.T.);
#7888=ORIENTED_EDGE('',*,*,#5547,.T.);
#7889=ORIENTED_EDGE('',*,*,#5546,.T.);
#7890=ORIENTED_EDGE('',*,*,#5545,.T.);
#7891=ORIENTED_EDGE('',*,*,#5544,.T.);
#7892=ORIENTED_EDGE('',*,*,#5543,.T.);
#7893=ORIENTED_EDGE('',*,*,#5573,.F.);
#7894=ORIENTED_EDGE('',*,*,#5623,.F.);
#7895=ORIENTED_EDGE('',*,*,#5541,.F.);
#7896=ORIENTED_EDGE('',*,*,#5540,.F.);
#7897=ORIENTED_EDGE('',*,*,#5539,.F.);
#7898=ORIENTED_EDGE('',*,*,#5538,.F.);
#7899=ORIENTED_EDGE('',*,*,#5537,.F.);
#7900=ORIENTED_EDGE('',*,*,#5536,.F.);
#7901=ORIENTED_EDGE('',*,*,#5535,.F.);
#7902=ORIENTED_EDGE('',*,*,#5534,.F.);
#7903=ORIENTED_EDGE('',*,*,#5533,.F.);
#7904=ORIENTED_EDGE('',*,*,#5532,.F.);
#7905=ORIENTED_EDGE('',*,*,#5555,.F.);
#7906=ORIENTED_EDGE('',*,*,#5627,.F.);
#7907=ORIENTED_EDGE('',*,*,#5559,.F.);
#7908=ORIENTED_EDGE('',*,*,#5558,.F.);
#7909=ORIENTED_EDGE('',*,*,#5557,.F.);
#7910=ORIENTED_EDGE('',*,*,#5556,.F.);
#7911=ORIENTED_EDGE('',*,*,#5574,.F.);
#7912=ORIENTED_EDGE('',*,*,#5621,.T.);
#7913=ORIENTED_EDGE('',*,*,#5628,.T.);
#7914=ORIENTED_EDGE('',*,*,#5629,.T.);
#7915=ORIENTED_EDGE('',*,*,#5628,.F.);
#7916=ORIENTED_EDGE('',*,*,#5624,.T.);
#7917=ORIENTED_EDGE('',*,*,#5572,.T.);
#7918=ORIENTED_EDGE('',*,*,#5625,.T.);
#7919=ORIENTED_EDGE('',*,*,#5629,.F.);
#7920=ORIENTED_EDGE('',*,*,#5620,.T.);
#7921=ORIENTED_EDGE('',*,*,#5630,.F.);
#7922=ORIENTED_EDGE('',*,*,#5592,.F.);
#7923=ORIENTED_EDGE('',*,*,#5591,.F.);
#7924=ORIENTED_EDGE('',*,*,#5590,.F.);
#7925=ORIENTED_EDGE('',*,*,#5603,.F.);
#7926=ORIENTED_EDGE('',*,*,#5602,.F.);
#7927=ORIENTED_EDGE('',*,*,#5601,.F.);
#7928=ORIENTED_EDGE('',*,*,#5631,.F.);
#7929=ORIENTED_EDGE('',*,*,#5587,.T.);
#7930=ORIENTED_EDGE('',*,*,#5586,.T.);
#7931=ORIENTED_EDGE('',*,*,#5585,.T.);
#7932=ORIENTED_EDGE('',*,*,#5584,.T.);
#7933=ORIENTED_EDGE('',*,*,#5583,.T.);
#7934=ORIENTED_EDGE('',*,*,#5582,.T.);
#7935=ORIENTED_EDGE('',*,*,#5632,.F.);
#7936=ORIENTED_EDGE('',*,*,#5633,.T.);
#7937=ORIENTED_EDGE('',*,*,#5588,.T.);
#7938=ORIENTED_EDGE('',*,*,#5631,.T.);
#7939=ORIENTED_EDGE('',*,*,#5634,.F.);
#7940=ORIENTED_EDGE('',*,*,#5635,.F.);
#7941=ORIENTED_EDGE('',*,*,#5580,.F.);
#7942=ORIENTED_EDGE('',*,*,#5579,.F.);
#7943=ORIENTED_EDGE('',*,*,#5578,.F.);
#7944=ORIENTED_EDGE('',*,*,#5577,.F.);
#7945=ORIENTED_EDGE('',*,*,#5576,.F.);
#7946=ORIENTED_EDGE('',*,*,#5589,.F.);
#7947=ORIENTED_EDGE('',*,*,#5633,.F.);
#7948=ORIENTED_EDGE('',*,*,#5599,.F.);
#7949=ORIENTED_EDGE('',*,*,#5598,.F.);
#7950=ORIENTED_EDGE('',*,*,#5597,.F.);
#7951=ORIENTED_EDGE('',*,*,#5596,.F.);
#7952=ORIENTED_EDGE('',*,*,#5595,.F.);
#7953=ORIENTED_EDGE('',*,*,#5594,.F.);
#7954=ORIENTED_EDGE('',*,*,#5630,.T.);
#7955=ORIENTED_EDGE('',*,*,#5581,.T.);
#7956=ORIENTED_EDGE('',*,*,#5635,.T.);
#7957=ORIENTED_EDGE('',*,*,#5593,.T.);
#7958=ORIENTED_EDGE('',*,*,#5636,.T.);
#7959=ORIENTED_EDGE('',*,*,#5632,.T.);
#7960=ORIENTED_EDGE('',*,*,#5637,.T.);
#7961=ORIENTED_EDGE('',*,*,#5609,.T.);
#7962=ORIENTED_EDGE('',*,*,#5637,.F.);
#7963=ORIENTED_EDGE('',*,*,#5634,.T.);
#7964=ORIENTED_EDGE('',*,*,#5600,.T.);
#7965=ORIENTED_EDGE('',*,*,#5626,.T.);
#7966=ORIENTED_EDGE('',*,*,#5560,.F.);
#7967=ORIENTED_EDGE('',*,*,#5627,.T.);
#7968=ORIENTED_EDGE('',*,*,#5554,.T.);
#7969=ORIENTED_EDGE('',*,*,#5638,.T.);
#7970=ORIENTED_EDGE('',*,*,#5638,.F.);
#7971=ORIENTED_EDGE('',*,*,#5639,.T.);
#7972=ORIENTED_EDGE('',*,*,#5636,.F.);
#7973=ORIENTED_EDGE('',*,*,#5639,.F.);
#7974=ORIENTED_EDGE('',*,*,#5640,.T.);
#7975=ORIENTED_EDGE('',*,*,#5641,.T.);
#7976=ORIENTED_EDGE('',*,*,#5642,.T.);
#7977=ORIENTED_EDGE('',*,*,#5641,.F.);
#7978=ORIENTED_EDGE('',*,*,#5643,.F.);
#7979=ORIENTED_EDGE('',*,*,#5644,.T.);
#7980=ORIENTED_EDGE('',*,*,#5640,.F.);
#7981=ORIENTED_EDGE('',*,*,#5644,.F.);
#7982=ORIENTED_EDGE('',*,*,#5642,.F.);
#7983=ORIENTED_EDGE('',*,*,#5643,.T.);
#7984=ORIENTED_EDGE('',*,*,#5645,.T.);
#7985=ORIENTED_EDGE('',*,*,#5646,.T.);
#7986=ORIENTED_EDGE('',*,*,#5645,.F.);
#7987=ORIENTED_EDGE('',*,*,#5646,.F.);
#7988=ORIENTED_EDGE('',*,*,#5647,.F.);
#7989=ORIENTED_EDGE('',*,*,#5648,.T.);
#7990=ORIENTED_EDGE('',*,*,#5649,.F.);
#7991=ORIENTED_EDGE('',*,*,#5650,.T.);
#7992=ORIENTED_EDGE('',*,*,#5651,.F.);
#7993=ORIENTED_EDGE('',*,*,#5652,.T.);
#7994=ORIENTED_EDGE('',*,*,#5653,.T.);
#7995=ORIENTED_EDGE('',*,*,#5647,.T.);
#7996=ORIENTED_EDGE('',*,*,#5654,.T.);
#7997=ORIENTED_EDGE('',*,*,#5655,.F.);
#7998=ORIENTED_EDGE('',*,*,#5656,.T.);
#7999=ORIENTED_EDGE('',*,*,#5651,.T.);
#8000=ORIENTED_EDGE('',*,*,#5657,.T.);
#8001=ORIENTED_EDGE('',*,*,#5658,.F.);
#8002=ORIENTED_EDGE('',*,*,#5659,.T.);
#8003=ORIENTED_EDGE('',*,*,#5655,.T.);
#8004=ORIENTED_EDGE('',*,*,#5660,.T.);
#8005=ORIENTED_EDGE('',*,*,#5661,.F.);
#8006=ORIENTED_EDGE('',*,*,#5662,.T.);
#8007=ORIENTED_EDGE('',*,*,#5658,.T.);
#8008=ORIENTED_EDGE('',*,*,#5663,.T.);
#8009=ORIENTED_EDGE('',*,*,#5664,.F.);
#8010=ORIENTED_EDGE('',*,*,#5665,.T.);
#8011=ORIENTED_EDGE('',*,*,#5666,.T.);
#8012=ORIENTED_EDGE('',*,*,#5667,.T.);
#8013=ORIENTED_EDGE('',*,*,#5668,.T.);
#8014=ORIENTED_EDGE('',*,*,#5669,.T.);
#8015=ORIENTED_EDGE('',*,*,#5670,.T.);
#8016=ORIENTED_EDGE('',*,*,#5665,.F.);
#8017=ORIENTED_EDGE('',*,*,#5671,.F.);
#8018=ORIENTED_EDGE('',*,*,#5672,.T.);
#8019=ORIENTED_EDGE('',*,*,#5673,.T.);
#8020=ORIENTED_EDGE('',*,*,#5674,.T.);
#8021=ORIENTED_EDGE('',*,*,#5668,.F.);
#8022=ORIENTED_EDGE('',*,*,#5675,.T.);
#8023=ORIENTED_EDGE('',*,*,#5661,.T.);
#8024=ORIENTED_EDGE('',*,*,#5676,.T.);
#8025=ORIENTED_EDGE('',*,*,#5677,.T.);
#8026=ORIENTED_EDGE('',*,*,#5678,.T.);
#8027=ORIENTED_EDGE('',*,*,#5679,.F.);
#8028=ORIENTED_EDGE('',*,*,#5680,.F.);
#8029=ORIENTED_EDGE('',*,*,#5681,.F.);
#8030=ORIENTED_EDGE('',*,*,#5682,.F.);
#8031=ORIENTED_EDGE('',*,*,#5683,.F.);
#8032=ORIENTED_EDGE('',*,*,#5684,.F.);
#8033=ORIENTED_EDGE('',*,*,#5685,.F.);
#8034=ORIENTED_EDGE('',*,*,#5686,.F.);
#8035=ORIENTED_EDGE('',*,*,#5687,.T.);
#8036=ORIENTED_EDGE('',*,*,#5688,.T.);
#8037=ORIENTED_EDGE('',*,*,#5671,.T.);
#8038=ORIENTED_EDGE('',*,*,#5689,.T.);
#8039=ORIENTED_EDGE('',*,*,#5673,.F.);
#8040=ORIENTED_EDGE('',*,*,#5690,.T.);
#8041=ORIENTED_EDGE('',*,*,#5691,.F.);
#8042=ORIENTED_EDGE('',*,*,#5692,.T.);
#8043=ORIENTED_EDGE('',*,*,#5693,.F.);
#8044=ORIENTED_EDGE('',*,*,#5694,.T.);
#8045=ORIENTED_EDGE('',*,*,#5695,.F.);
#8046=ORIENTED_EDGE('',*,*,#5696,.T.);
#8047=ORIENTED_EDGE('',*,*,#5697,.F.);
#8048=ORIENTED_EDGE('',*,*,#5698,.T.);
#8049=ORIENTED_EDGE('',*,*,#5699,.F.);
#8050=ORIENTED_EDGE('',*,*,#5700,.T.);
#8051=ORIENTED_EDGE('',*,*,#5701,.F.);
#8052=ORIENTED_EDGE('',*,*,#5702,.T.);
#8053=ORIENTED_EDGE('',*,*,#5690,.F.);
#8054=ORIENTED_EDGE('',*,*,#5672,.F.);
#8055=ORIENTED_EDGE('',*,*,#5674,.F.);
#8056=ORIENTED_EDGE('',*,*,#5689,.F.);
#8057=ORIENTED_EDGE('',*,*,#5703,.T.);
#8058=ORIENTED_EDGE('',*,*,#5704,.F.);
#8059=ORIENTED_EDGE('',*,*,#5703,.F.);
#8060=ORIENTED_EDGE('',*,*,#5705,.T.);
#8061=ORIENTED_EDGE('',*,*,#5706,.T.);
#8062=ORIENTED_EDGE('',*,*,#5707,.T.);
#8063=ORIENTED_EDGE('',*,*,#5691,.T.);
#8064=ORIENTED_EDGE('',*,*,#5705,.F.);
#8065=ORIENTED_EDGE('',*,*,#5702,.F.);
#8066=ORIENTED_EDGE('',*,*,#5708,.F.);
#8067=ORIENTED_EDGE('',*,*,#5709,.F.);
#8068=ORIENTED_EDGE('',*,*,#5710,.F.);
#8069=ORIENTED_EDGE('',*,*,#5711,.T.);
#8070=ORIENTED_EDGE('',*,*,#5712,.F.);
#8071=ORIENTED_EDGE('',*,*,#5713,.F.);
#8072=ORIENTED_EDGE('',*,*,#5714,.T.);
#8073=ORIENTED_EDGE('',*,*,#5715,.T.);
#8074=ORIENTED_EDGE('',*,*,#5716,.T.);
#8075=ORIENTED_EDGE('',*,*,#5717,.T.);
#8076=ORIENTED_EDGE('',*,*,#5693,.T.);
#8077=ORIENTED_EDGE('',*,*,#5717,.F.);
#8078=ORIENTED_EDGE('',*,*,#5718,.F.);
#8079=ORIENTED_EDGE('',*,*,#5719,.F.);
#8080=ORIENTED_EDGE('',*,*,#5720,.T.);
#8081=ORIENTED_EDGE('',*,*,#5721,.F.);
#8082=ORIENTED_EDGE('',*,*,#5722,.F.);
#8083=ORIENTED_EDGE('',*,*,#5723,.F.);
#8084=ORIENTED_EDGE('',*,*,#5694,.F.);
#8085=ORIENTED_EDGE('',*,*,#5724,.T.);
#8086=ORIENTED_EDGE('',*,*,#5723,.T.);
#8087=ORIENTED_EDGE('',*,*,#5725,.T.);
#8088=ORIENTED_EDGE('',*,*,#5726,.T.);
#8089=ORIENTED_EDGE('',*,*,#5695,.T.);
#8090=ORIENTED_EDGE('',*,*,#5727,.T.);
#8091=ORIENTED_EDGE('',*,*,#5728,.T.);
#8092=ORIENTED_EDGE('',*,*,#5729,.T.);
#8093=ORIENTED_EDGE('',*,*,#5697,.T.);
#8094=ORIENTED_EDGE('',*,*,#5729,.F.);
#8095=ORIENTED_EDGE('',*,*,#5730,.F.);
#8096=ORIENTED_EDGE('',*,*,#5731,.F.);
#8097=ORIENTED_EDGE('',*,*,#5732,.T.);
#8098=ORIENTED_EDGE('',*,*,#5733,.F.);
#8099=ORIENTED_EDGE('',*,*,#5734,.F.);
#8100=ORIENTED_EDGE('',*,*,#5735,.F.);
#8101=ORIENTED_EDGE('',*,*,#5698,.F.);
#8102=ORIENTED_EDGE('',*,*,#5735,.T.);
#8103=ORIENTED_EDGE('',*,*,#5736,.T.);
#8104=ORIENTED_EDGE('',*,*,#5737,.T.);
#8105=ORIENTED_EDGE('',*,*,#5699,.T.);
#8106=ORIENTED_EDGE('',*,*,#5738,.T.);
#8107=ORIENTED_EDGE('',*,*,#5739,.T.);
#8108=ORIENTED_EDGE('',*,*,#5708,.T.);
#8109=ORIENTED_EDGE('',*,*,#5701,.T.);
#8110=ORIENTED_EDGE('',*,*,#5710,.T.);
#8111=ORIENTED_EDGE('',*,*,#5740,.T.);
#8112=ORIENTED_EDGE('',*,*,#5741,.T.);
#8113=ORIENTED_EDGE('',*,*,#5742,.T.);
#8114=ORIENTED_EDGE('',*,*,#5742,.F.);
#8115=ORIENTED_EDGE('',*,*,#5743,.F.);
#8116=ORIENTED_EDGE('',*,*,#5744,.F.);
#8117=ORIENTED_EDGE('',*,*,#5732,.F.);
#8118=ORIENTED_EDGE('',*,*,#5745,.F.);
#8119=ORIENTED_EDGE('',*,*,#5746,.F.);
#8120=ORIENTED_EDGE('',*,*,#5747,.F.);
#8121=ORIENTED_EDGE('',*,*,#5720,.F.);
#8122=ORIENTED_EDGE('',*,*,#5748,.F.);
#8123=ORIENTED_EDGE('',*,*,#5749,.F.);
#8124=ORIENTED_EDGE('',*,*,#5750,.F.);
#8125=ORIENTED_EDGE('',*,*,#5711,.F.);
#8126=ORIENTED_EDGE('',*,*,#5751,.F.);
#8127=ORIENTED_EDGE('',*,*,#5752,.T.);
#8128=ORIENTED_EDGE('',*,*,#5753,.T.);
#8129=ORIENTED_EDGE('',*,*,#5733,.T.);
#8130=ORIENTED_EDGE('',*,*,#5744,.T.);
#8131=ORIENTED_EDGE('',*,*,#5731,.T.);
#8132=ORIENTED_EDGE('',*,*,#5754,.T.);
#8133=ORIENTED_EDGE('',*,*,#5755,.T.);
#8134=ORIENTED_EDGE('',*,*,#5745,.T.);
#8135=ORIENTED_EDGE('',*,*,#5756,.T.);
#8136=ORIENTED_EDGE('',*,*,#5757,.T.);
#8137=ORIENTED_EDGE('',*,*,#5721,.T.);
#8138=ORIENTED_EDGE('',*,*,#5747,.T.);
#8139=ORIENTED_EDGE('',*,*,#5719,.T.);
#8140=ORIENTED_EDGE('',*,*,#5758,.T.);
#8141=ORIENTED_EDGE('',*,*,#5759,.T.);
#8142=ORIENTED_EDGE('',*,*,#5748,.T.);
#8143=ORIENTED_EDGE('',*,*,#5707,.F.);
#8144=ORIENTED_EDGE('',*,*,#5760,.F.);
#8145=ORIENTED_EDGE('',*,*,#5761,.F.);
#8146=ORIENTED_EDGE('',*,*,#5749,.T.);
#8147=ORIENTED_EDGE('',*,*,#5759,.F.);
#8148=ORIENTED_EDGE('',*,*,#5762,.F.);
#8149=ORIENTED_EDGE('',*,*,#5715,.F.);
#8150=ORIENTED_EDGE('',*,*,#5692,.F.);
#8151=ORIENTED_EDGE('',*,*,#5763,.T.);
#8152=ORIENTED_EDGE('',*,*,#5716,.F.);
#8153=ORIENTED_EDGE('',*,*,#5762,.T.);
#8154=ORIENTED_EDGE('',*,*,#5758,.F.);
#8155=ORIENTED_EDGE('',*,*,#5718,.T.);
#8156=ORIENTED_EDGE('',*,*,#5725,.F.);
#8157=ORIENTED_EDGE('',*,*,#5722,.T.);
#8158=ORIENTED_EDGE('',*,*,#5757,.F.);
#8159=ORIENTED_EDGE('',*,*,#5764,.T.);
#8160=ORIENTED_EDGE('',*,*,#5726,.F.);
#8161=ORIENTED_EDGE('',*,*,#5764,.F.);
#8162=ORIENTED_EDGE('',*,*,#5756,.F.);
#8163=ORIENTED_EDGE('',*,*,#5746,.T.);
#8164=ORIENTED_EDGE('',*,*,#5755,.F.);
#8165=ORIENTED_EDGE('',*,*,#5765,.F.);
#8166=ORIENTED_EDGE('',*,*,#5727,.F.);
#8167=ORIENTED_EDGE('',*,*,#5696,.F.);
#8168=ORIENTED_EDGE('',*,*,#5728,.F.);
#8169=ORIENTED_EDGE('',*,*,#5765,.T.);
#8170=ORIENTED_EDGE('',*,*,#5754,.F.);
#8171=ORIENTED_EDGE('',*,*,#5730,.T.);
#8172=ORIENTED_EDGE('',*,*,#5736,.F.);
#8173=ORIENTED_EDGE('',*,*,#5734,.T.);
#8174=ORIENTED_EDGE('',*,*,#5753,.F.);
#8175=ORIENTED_EDGE('',*,*,#5766,.T.);
#8176=ORIENTED_EDGE('',*,*,#5737,.F.);
#8177=ORIENTED_EDGE('',*,*,#5766,.F.);
#8178=ORIENTED_EDGE('',*,*,#5752,.F.);
#8179=ORIENTED_EDGE('',*,*,#5743,.T.);
#8180=ORIENTED_EDGE('',*,*,#5741,.F.);
#8181=ORIENTED_EDGE('',*,*,#5767,.F.);
#8182=ORIENTED_EDGE('',*,*,#5738,.F.);
#8183=ORIENTED_EDGE('',*,*,#5700,.F.);
#8184=ORIENTED_EDGE('',*,*,#5739,.F.);
#8185=ORIENTED_EDGE('',*,*,#5767,.T.);
#8186=ORIENTED_EDGE('',*,*,#5740,.F.);
#8187=ORIENTED_EDGE('',*,*,#5709,.T.);
#8188=ORIENTED_EDGE('',*,*,#5761,.T.);
#8189=ORIENTED_EDGE('',*,*,#5768,.T.);
#8190=ORIENTED_EDGE('',*,*,#5712,.T.);
#8191=ORIENTED_EDGE('',*,*,#5750,.T.);
#8192=ORIENTED_EDGE('',*,*,#5706,.F.);
#8193=ORIENTED_EDGE('',*,*,#5713,.T.);
#8194=ORIENTED_EDGE('',*,*,#5768,.F.);
#8195=ORIENTED_EDGE('',*,*,#5760,.T.);
#8196=ORIENTED_EDGE('',*,*,#5664,.T.);
#8197=ORIENTED_EDGE('',*,*,#5769,.T.);
#8198=ORIENTED_EDGE('',*,*,#5751,.T.);
#8199=ORIENTED_EDGE('',*,*,#5769,.F.);
#8200=ORIENTED_EDGE('',*,*,#5770,.T.);
#8201=ORIENTED_EDGE('',*,*,#5724,.F.);
#8202=ORIENTED_EDGE('',*,*,#5770,.F.);
#8203=ORIENTED_EDGE('',*,*,#5771,.T.);
#8204=ORIENTED_EDGE('',*,*,#5763,.F.);
#8205=ORIENTED_EDGE('',*,*,#5771,.F.);
#8206=ORIENTED_EDGE('',*,*,#5772,.T.);
#8207=ORIENTED_EDGE('',*,*,#5714,.F.);
#8208=ORIENTED_EDGE('',*,*,#5772,.F.);
#8209=ORIENTED_EDGE('',*,*,#5773,.T.);
#8210=ORIENTED_EDGE('',*,*,#5774,.T.);
#8211=ORIENTED_EDGE('',*,*,#5775,.F.);
#8212=ORIENTED_EDGE('',*,*,#5776,.F.);
#8213=ORIENTED_EDGE('',*,*,#5774,.F.);
#8214=ORIENTED_EDGE('',*,*,#5777,.F.);
#8215=ORIENTED_EDGE('',*,*,#5778,.T.);
#8216=ORIENTED_EDGE('',*,*,#5773,.F.);
#8217=ORIENTED_EDGE('',*,*,#5778,.F.);
#8218=ORIENTED_EDGE('',*,*,#5779,.T.);
#8219=ORIENTED_EDGE('',*,*,#5780,.T.);
#8220=ORIENTED_EDGE('',*,*,#5781,.T.);
#8221=ORIENTED_EDGE('',*,*,#5780,.F.);
#8222=ORIENTED_EDGE('',*,*,#5782,.F.);
#8223=ORIENTED_EDGE('',*,*,#5781,.F.);
#8224=ORIENTED_EDGE('',*,*,#5779,.F.);
#8225=ORIENTED_EDGE('',*,*,#5783,.T.);
#8226=ORIENTED_EDGE('',*,*,#5775,.T.);
#8227=ORIENTED_EDGE('',*,*,#5776,.T.);
#8228=ORIENTED_EDGE('',*,*,#5783,.F.);
#8229=ORIENTED_EDGE('',*,*,#5784,.T.);
#8230=ORIENTED_EDGE('',*,*,#5785,.T.);
#8231=ORIENTED_EDGE('',*,*,#5782,.T.);
#8232=ORIENTED_EDGE('',*,*,#5785,.F.);
#8233=ORIENTED_EDGE('',*,*,#5786,.T.);
#8234=ORIENTED_EDGE('',*,*,#5649,.T.);
#8235=ORIENTED_EDGE('',*,*,#5787,.T.);
#8236=ORIENTED_EDGE('',*,*,#5670,.F.);
#8237=ORIENTED_EDGE('',*,*,#5788,.T.);
#8238=ORIENTED_EDGE('',*,*,#5679,.T.);
#8239=ORIENTED_EDGE('',*,*,#5789,.T.);
#8240=ORIENTED_EDGE('',*,*,#5666,.F.);
#8241=ORIENTED_EDGE('',*,*,#5788,.F.);
#8242=ORIENTED_EDGE('',*,*,#5669,.F.);
#8243=ORIENTED_EDGE('',*,*,#5676,.F.);
#8244=ORIENTED_EDGE('',*,*,#5663,.F.);
#8245=ORIENTED_EDGE('',*,*,#5660,.F.);
#8246=ORIENTED_EDGE('',*,*,#5657,.F.);
#8247=ORIENTED_EDGE('',*,*,#5654,.F.);
#8248=ORIENTED_EDGE('',*,*,#5650,.F.);
#8249=ORIENTED_EDGE('',*,*,#5790,.F.);
#8250=ORIENTED_EDGE('',*,*,#5685,.T.);
#8251=ORIENTED_EDGE('',*,*,#5684,.T.);
#8252=ORIENTED_EDGE('',*,*,#5683,.T.);
#8253=ORIENTED_EDGE('',*,*,#5682,.T.);
#8254=ORIENTED_EDGE('',*,*,#5681,.T.);
#8255=ORIENTED_EDGE('',*,*,#5680,.T.);
#8256=ORIENTED_EDGE('',*,*,#5784,.F.);
#8257=ORIENTED_EDGE('',*,*,#5791,.T.);
#8258=ORIENTED_EDGE('',*,*,#5686,.T.);
#8259=ORIENTED_EDGE('',*,*,#5790,.T.);
#8260=ORIENTED_EDGE('',*,*,#5786,.F.);
#8261=ORIENTED_EDGE('',*,*,#5789,.F.);
#8262=ORIENTED_EDGE('',*,*,#5678,.F.);
#8263=ORIENTED_EDGE('',*,*,#5677,.F.);
#8264=ORIENTED_EDGE('',*,*,#5688,.F.);
#8265=ORIENTED_EDGE('',*,*,#5687,.F.);
#8266=ORIENTED_EDGE('',*,*,#5791,.F.);
#8267=ORIENTED_EDGE('',*,*,#5787,.F.);
#8268=ORIENTED_EDGE('',*,*,#5648,.F.);
#8269=ORIENTED_EDGE('',*,*,#5653,.F.);
#8270=ORIENTED_EDGE('',*,*,#5652,.F.);
#8271=ORIENTED_EDGE('',*,*,#5656,.F.);
#8272=ORIENTED_EDGE('',*,*,#5659,.F.);
#8273=ORIENTED_EDGE('',*,*,#5662,.F.);
#8274=ORIENTED_EDGE('',*,*,#5675,.F.);
#8275=ORIENTED_EDGE('',*,*,#5667,.F.);
#8276=ORIENTED_EDGE('',*,*,#5704,.T.);
#8277=ORIENTED_EDGE('',*,*,#5777,.T.);
#8278=ORIENTED_EDGE('',*,*,#5792,.F.);
#8279=ORIENTED_EDGE('',*,*,#5793,.T.);
#8280=ORIENTED_EDGE('',*,*,#5794,.T.);
#8281=ORIENTED_EDGE('',*,*,#5795,.F.);
#8282=ORIENTED_EDGE('',*,*,#5793,.F.);
#8283=ORIENTED_EDGE('',*,*,#5796,.T.);
#8284=ORIENTED_EDGE('',*,*,#5797,.F.);
#8285=ORIENTED_EDGE('',*,*,#5798,.T.);
#8286=ORIENTED_EDGE('',*,*,#5796,.F.);
#8287=ORIENTED_EDGE('',*,*,#5799,.T.);
#8288=ORIENTED_EDGE('',*,*,#5800,.T.);
#8289=ORIENTED_EDGE('',*,*,#5801,.F.);
#8290=ORIENTED_EDGE('',*,*,#5799,.F.);
#8291=ORIENTED_EDGE('',*,*,#5802,.T.);
#8292=ORIENTED_EDGE('',*,*,#5803,.F.);
#8293=ORIENTED_EDGE('',*,*,#5804,.T.);
#8294=ORIENTED_EDGE('',*,*,#5802,.F.);
#8295=ORIENTED_EDGE('',*,*,#5805,.T.);
#8296=ORIENTED_EDGE('',*,*,#5806,.T.);
#8297=ORIENTED_EDGE('',*,*,#5807,.F.);
#8298=ORIENTED_EDGE('',*,*,#5808,.F.);
#8299=ORIENTED_EDGE('',*,*,#5809,.T.);
#8300=ORIENTED_EDGE('',*,*,#5810,.T.);
#8301=ORIENTED_EDGE('',*,*,#5811,.F.);
#8302=ORIENTED_EDGE('',*,*,#5809,.F.);
#8303=ORIENTED_EDGE('',*,*,#5812,.T.);
#8304=ORIENTED_EDGE('',*,*,#5813,.F.);
#8305=ORIENTED_EDGE('',*,*,#5814,.T.);
#8306=ORIENTED_EDGE('',*,*,#5812,.F.);
#8307=ORIENTED_EDGE('',*,*,#5815,.T.);
#8308=ORIENTED_EDGE('',*,*,#5816,.T.);
#8309=ORIENTED_EDGE('',*,*,#5817,.F.);
#8310=ORIENTED_EDGE('',*,*,#5815,.F.);
#8311=ORIENTED_EDGE('',*,*,#5818,.T.);
#8312=ORIENTED_EDGE('',*,*,#5819,.F.);
#8313=ORIENTED_EDGE('',*,*,#5820,.T.);
#8314=ORIENTED_EDGE('',*,*,#5818,.F.);
#8315=ORIENTED_EDGE('',*,*,#5821,.T.);
#8316=ORIENTED_EDGE('',*,*,#5822,.T.);
#8317=ORIENTED_EDGE('',*,*,#5823,.F.);
#8318=ORIENTED_EDGE('',*,*,#5824,.F.);
#8319=ORIENTED_EDGE('',*,*,#5825,.T.);
#8320=ORIENTED_EDGE('',*,*,#5826,.T.);
#8321=ORIENTED_EDGE('',*,*,#5827,.F.);
#8322=ORIENTED_EDGE('',*,*,#5825,.F.);
#8323=ORIENTED_EDGE('',*,*,#5828,.T.);
#8324=ORIENTED_EDGE('',*,*,#5829,.F.);
#8325=ORIENTED_EDGE('',*,*,#5830,.T.);
#8326=ORIENTED_EDGE('',*,*,#5828,.F.);
#8327=ORIENTED_EDGE('',*,*,#5831,.T.);
#8328=ORIENTED_EDGE('',*,*,#5832,.T.);
#8329=ORIENTED_EDGE('',*,*,#5833,.F.);
#8330=ORIENTED_EDGE('',*,*,#5831,.F.);
#8331=ORIENTED_EDGE('',*,*,#5834,.T.);
#8332=ORIENTED_EDGE('',*,*,#5835,.F.);
#8333=ORIENTED_EDGE('',*,*,#5836,.T.);
#8334=ORIENTED_EDGE('',*,*,#5834,.F.);
#8335=ORIENTED_EDGE('',*,*,#5837,.T.);
#8336=ORIENTED_EDGE('',*,*,#5838,.T.);
#8337=ORIENTED_EDGE('',*,*,#5839,.F.);
#8338=ORIENTED_EDGE('',*,*,#5840,.F.);
#8339=ORIENTED_EDGE('',*,*,#5841,.T.);
#8340=ORIENTED_EDGE('',*,*,#5842,.T.);
#8341=ORIENTED_EDGE('',*,*,#5843,.F.);
#8342=ORIENTED_EDGE('',*,*,#5841,.F.);
#8343=ORIENTED_EDGE('',*,*,#5844,.T.);
#8344=ORIENTED_EDGE('',*,*,#5845,.F.);
#8345=ORIENTED_EDGE('',*,*,#5846,.T.);
#8346=ORIENTED_EDGE('',*,*,#5844,.F.);
#8347=ORIENTED_EDGE('',*,*,#5847,.T.);
#8348=ORIENTED_EDGE('',*,*,#5848,.T.);
#8349=ORIENTED_EDGE('',*,*,#5849,.F.);
#8350=ORIENTED_EDGE('',*,*,#5847,.F.);
#8351=ORIENTED_EDGE('',*,*,#5850,.T.);
#8352=ORIENTED_EDGE('',*,*,#5851,.F.);
#8353=ORIENTED_EDGE('',*,*,#5852,.T.);
#8354=ORIENTED_EDGE('',*,*,#5850,.F.);
#8355=ORIENTED_EDGE('',*,*,#5853,.T.);
#8356=ORIENTED_EDGE('',*,*,#5854,.T.);
#8357=ORIENTED_EDGE('',*,*,#5855,.F.);
#8358=ORIENTED_EDGE('',*,*,#5840,.T.);
#8359=ORIENTED_EDGE('',*,*,#5856,.F.);
#8360=ORIENTED_EDGE('',*,*,#5857,.T.);
#8361=ORIENTED_EDGE('',*,*,#5853,.F.);
#8362=ORIENTED_EDGE('',*,*,#5858,.T.);
#8363=ORIENTED_EDGE('',*,*,#5859,.T.);
#8364=ORIENTED_EDGE('',*,*,#5856,.T.);
#8365=ORIENTED_EDGE('',*,*,#5843,.T.);
#8366=ORIENTED_EDGE('',*,*,#5860,.T.);
#8367=ORIENTED_EDGE('',*,*,#5824,.T.);
#8368=ORIENTED_EDGE('',*,*,#5861,.F.);
#8369=ORIENTED_EDGE('',*,*,#5862,.T.);
#8370=ORIENTED_EDGE('',*,*,#5837,.F.);
#8371=ORIENTED_EDGE('',*,*,#5863,.T.);
#8372=ORIENTED_EDGE('',*,*,#5864,.T.);
#8373=ORIENTED_EDGE('',*,*,#5861,.T.);
#8374=ORIENTED_EDGE('',*,*,#5827,.T.);
#8375=ORIENTED_EDGE('',*,*,#5865,.T.);
#8376=ORIENTED_EDGE('',*,*,#5845,.T.);
#8377=ORIENTED_EDGE('',*,*,#5849,.T.);
#8378=ORIENTED_EDGE('',*,*,#5866,.T.);
#8379=ORIENTED_EDGE('',*,*,#5835,.T.);
#8380=ORIENTED_EDGE('',*,*,#5839,.T.);
#8381=ORIENTED_EDGE('',*,*,#5867,.T.);
#8382=ORIENTED_EDGE('',*,*,#5808,.T.);
#8383=ORIENTED_EDGE('',*,*,#5868,.F.);
#8384=ORIENTED_EDGE('',*,*,#5869,.T.);
#8385=ORIENTED_EDGE('',*,*,#5821,.F.);
#8386=ORIENTED_EDGE('',*,*,#5870,.T.);
#8387=ORIENTED_EDGE('',*,*,#5871,.T.);
#8388=ORIENTED_EDGE('',*,*,#5813,.T.);
#8389=ORIENTED_EDGE('',*,*,#5817,.T.);
#8390=ORIENTED_EDGE('',*,*,#5872,.T.);
#8391=ORIENTED_EDGE('',*,*,#5792,.T.);
#8392=ORIENTED_EDGE('',*,*,#5873,.F.);
#8393=ORIENTED_EDGE('',*,*,#5874,.T.);
#8394=ORIENTED_EDGE('',*,*,#5805,.F.);
#8395=ORIENTED_EDGE('',*,*,#5875,.T.);
#8396=ORIENTED_EDGE('',*,*,#5876,.T.);
#8397=ORIENTED_EDGE('',*,*,#5803,.T.);
#8398=ORIENTED_EDGE('',*,*,#5807,.T.);
#8399=ORIENTED_EDGE('',*,*,#5877,.T.);
#8400=ORIENTED_EDGE('',*,*,#5829,.T.);
#8401=ORIENTED_EDGE('',*,*,#5833,.T.);
#8402=ORIENTED_EDGE('',*,*,#5878,.T.);
#8403=ORIENTED_EDGE('',*,*,#5797,.T.);
#8404=ORIENTED_EDGE('',*,*,#5801,.T.);
#8405=ORIENTED_EDGE('',*,*,#5879,.T.);
#8406=ORIENTED_EDGE('',*,*,#5873,.T.);
#8407=ORIENTED_EDGE('',*,*,#5795,.T.);
#8408=ORIENTED_EDGE('',*,*,#5880,.T.);
#8409=ORIENTED_EDGE('',*,*,#5868,.T.);
#8410=ORIENTED_EDGE('',*,*,#5811,.T.);
#8411=ORIENTED_EDGE('',*,*,#5881,.T.);
#8412=ORIENTED_EDGE('',*,*,#5819,.T.);
#8413=ORIENTED_EDGE('',*,*,#5823,.T.);
#8414=ORIENTED_EDGE('',*,*,#5882,.T.);
#8415=ORIENTED_EDGE('',*,*,#5851,.T.);
#8416=ORIENTED_EDGE('',*,*,#5855,.T.);
#8417=ORIENTED_EDGE('',*,*,#5883,.T.);
#8418=ORIENTED_EDGE('',*,*,#5860,.F.);
#8419=ORIENTED_EDGE('',*,*,#5842,.F.);
#8420=ORIENTED_EDGE('',*,*,#5846,.F.);
#8421=ORIENTED_EDGE('',*,*,#5867,.F.);
#8422=ORIENTED_EDGE('',*,*,#5838,.F.);
#8423=ORIENTED_EDGE('',*,*,#5862,.F.);
#8424=ORIENTED_EDGE('',*,*,#5864,.F.);
#8425=ORIENTED_EDGE('',*,*,#5884,.F.);
#8426=ORIENTED_EDGE('',*,*,#5885,.T.);
#8427=ORIENTED_EDGE('',*,*,#5886,.T.);
#8428=ORIENTED_EDGE('',*,*,#5887,.T.);
#8429=ORIENTED_EDGE('',*,*,#5888,.F.);
#8430=ORIENTED_EDGE('',*,*,#5889,.F.);
#8431=ORIENTED_EDGE('',*,*,#5890,.T.);
#8432=ORIENTED_EDGE('',*,*,#5891,.T.);
#8433=ORIENTED_EDGE('',*,*,#5892,.T.);
#8434=ORIENTED_EDGE('',*,*,#5863,.F.);
#8435=ORIENTED_EDGE('',*,*,#5893,.F.);
#8436=ORIENTED_EDGE('',*,*,#5894,.T.);
#8437=ORIENTED_EDGE('',*,*,#5895,.F.);
#8438=ORIENTED_EDGE('',*,*,#5896,.T.);
#8439=ORIENTED_EDGE('',*,*,#5897,.T.);
#8440=ORIENTED_EDGE('',*,*,#5884,.T.);
#8441=ORIENTED_EDGE('',*,*,#5865,.F.);
#8442=ORIENTED_EDGE('',*,*,#5826,.F.);
#8443=ORIENTED_EDGE('',*,*,#5830,.F.);
#8444=ORIENTED_EDGE('',*,*,#5879,.F.);
#8445=ORIENTED_EDGE('',*,*,#5800,.F.);
#8446=ORIENTED_EDGE('',*,*,#5804,.F.);
#8447=ORIENTED_EDGE('',*,*,#5876,.F.);
#8448=ORIENTED_EDGE('',*,*,#5898,.T.);
#8449=ORIENTED_EDGE('',*,*,#5899,.T.);
#8450=ORIENTED_EDGE('',*,*,#5900,.F.);
#8451=ORIENTED_EDGE('',*,*,#5901,.F.);
#8452=ORIENTED_EDGE('',*,*,#5902,.T.);
#8453=ORIENTED_EDGE('',*,*,#5903,.T.);
#8454=ORIENTED_EDGE('',*,*,#5904,.F.);
#8455=ORIENTED_EDGE('',*,*,#5905,.F.);
#8456=ORIENTED_EDGE('',*,*,#5893,.T.);
#8457=ORIENTED_EDGE('',*,*,#5875,.F.);
#8458=ORIENTED_EDGE('',*,*,#5906,.F.);
#8459=ORIENTED_EDGE('',*,*,#5907,.F.);
#8460=ORIENTED_EDGE('',*,*,#5908,.F.);
#8461=ORIENTED_EDGE('',*,*,#5909,.F.);
#8462=ORIENTED_EDGE('',*,*,#5910,.T.);
#8463=ORIENTED_EDGE('',*,*,#5898,.F.);
#8464=ORIENTED_EDGE('',*,*,#5798,.F.);
#8465=ORIENTED_EDGE('',*,*,#5878,.F.);
#8466=ORIENTED_EDGE('',*,*,#5832,.F.);
#8467=ORIENTED_EDGE('',*,*,#5836,.F.);
#8468=ORIENTED_EDGE('',*,*,#5866,.F.);
#8469=ORIENTED_EDGE('',*,*,#5848,.F.);
#8470=ORIENTED_EDGE('',*,*,#5852,.F.);
#8471=ORIENTED_EDGE('',*,*,#5882,.F.);
#8472=ORIENTED_EDGE('',*,*,#5822,.F.);
#8473=ORIENTED_EDGE('',*,*,#5869,.F.);
#8474=ORIENTED_EDGE('',*,*,#5880,.F.);
#8475=ORIENTED_EDGE('',*,*,#5794,.F.);
#8476=ORIENTED_EDGE('',*,*,#5911,.F.);
#8477=ORIENTED_EDGE('',*,*,#5912,.T.);
#8478=ORIENTED_EDGE('',*,*,#5913,.T.);
#8479=ORIENTED_EDGE('',*,*,#5914,.T.);
#8480=ORIENTED_EDGE('',*,*,#5915,.T.);
#8481=ORIENTED_EDGE('',*,*,#5916,.T.);
#8482=ORIENTED_EDGE('',*,*,#5914,.F.);
#8483=ORIENTED_EDGE('',*,*,#5917,.T.);
#8484=ORIENTED_EDGE('',*,*,#5900,.T.);
#8485=ORIENTED_EDGE('',*,*,#5918,.T.);
#8486=ORIENTED_EDGE('',*,*,#5913,.F.);
#8487=ORIENTED_EDGE('',*,*,#5919,.F.);
#8488=ORIENTED_EDGE('',*,*,#5920,.T.);
#8489=ORIENTED_EDGE('',*,*,#5921,.F.);
#8490=ORIENTED_EDGE('',*,*,#5901,.T.);
#8491=ORIENTED_EDGE('',*,*,#5917,.F.);
#8492=ORIENTED_EDGE('',*,*,#5922,.T.);
#8493=ORIENTED_EDGE('',*,*,#5923,.T.);
#8494=ORIENTED_EDGE('',*,*,#5924,.T.);
#8495=ORIENTED_EDGE('',*,*,#5925,.T.);
#8496=ORIENTED_EDGE('',*,*,#5923,.F.);
#8497=ORIENTED_EDGE('',*,*,#5926,.T.);
#8498=ORIENTED_EDGE('',*,*,#5904,.T.);
#8499=ORIENTED_EDGE('',*,*,#5927,.T.);
#8500=ORIENTED_EDGE('',*,*,#5922,.F.);
#8501=ORIENTED_EDGE('',*,*,#5928,.F.);
#8502=ORIENTED_EDGE('',*,*,#5929,.F.);
#8503=ORIENTED_EDGE('',*,*,#5894,.F.);
#8504=ORIENTED_EDGE('',*,*,#5905,.T.);
#8505=ORIENTED_EDGE('',*,*,#5926,.F.);
#8506=ORIENTED_EDGE('',*,*,#5930,.T.);
#8507=ORIENTED_EDGE('',*,*,#5931,.T.);
#8508=ORIENTED_EDGE('',*,*,#5932,.T.);
#8509=ORIENTED_EDGE('',*,*,#5933,.T.);
#8510=ORIENTED_EDGE('',*,*,#5932,.F.);
#8511=ORIENTED_EDGE('',*,*,#5934,.F.);
#8512=ORIENTED_EDGE('',*,*,#5887,.F.);
#8513=ORIENTED_EDGE('',*,*,#5935,.F.);
#8514=ORIENTED_EDGE('',*,*,#5936,.T.);
#8515=ORIENTED_EDGE('',*,*,#5937,.T.);
#8516=ORIENTED_EDGE('',*,*,#5938,.T.);
#8517=ORIENTED_EDGE('',*,*,#5931,.F.);
#8518=ORIENTED_EDGE('',*,*,#5939,.T.);
#8519=ORIENTED_EDGE('',*,*,#5888,.T.);
#8520=ORIENTED_EDGE('',*,*,#5934,.T.);
#8521=ORIENTED_EDGE('',*,*,#5940,.T.);
#8522=ORIENTED_EDGE('',*,*,#5941,.T.);
#8523=ORIENTED_EDGE('',*,*,#5942,.T.);
#8524=ORIENTED_EDGE('',*,*,#5943,.T.);
#8525=ORIENTED_EDGE('',*,*,#5942,.F.);
#8526=ORIENTED_EDGE('',*,*,#5944,.F.);
#8527=ORIENTED_EDGE('',*,*,#5945,.F.);
#8528=ORIENTED_EDGE('',*,*,#5946,.F.);
#8529=ORIENTED_EDGE('',*,*,#5947,.T.);
#8530=ORIENTED_EDGE('',*,*,#5948,.F.);
#8531=ORIENTED_EDGE('',*,*,#5949,.T.);
#8532=ORIENTED_EDGE('',*,*,#5941,.F.);
#8533=ORIENTED_EDGE('',*,*,#5950,.T.);
#8534=ORIENTED_EDGE('',*,*,#5951,.T.);
#8535=ORIENTED_EDGE('',*,*,#5944,.T.);
#8536=ORIENTED_EDGE('',*,*,#5952,.T.);
#8537=ORIENTED_EDGE('',*,*,#5953,.T.);
#8538=ORIENTED_EDGE('',*,*,#5954,.T.);
#8539=ORIENTED_EDGE('',*,*,#5955,.T.);
#8540=ORIENTED_EDGE('',*,*,#5953,.F.);
#8541=ORIENTED_EDGE('',*,*,#5956,.T.);
#8542=ORIENTED_EDGE('',*,*,#5957,.T.);
#8543=ORIENTED_EDGE('',*,*,#5958,.T.);
#8544=ORIENTED_EDGE('',*,*,#5952,.F.);
#8545=ORIENTED_EDGE('',*,*,#5959,.F.);
#8546=ORIENTED_EDGE('',*,*,#5960,.F.);
#8547=ORIENTED_EDGE('',*,*,#5961,.F.);
#8548=ORIENTED_EDGE('',*,*,#5962,.T.);
#8549=ORIENTED_EDGE('',*,*,#5956,.F.);
#8550=ORIENTED_EDGE('',*,*,#5963,.F.);
#8551=ORIENTED_EDGE('',*,*,#5960,.T.);
#8552=ORIENTED_EDGE('',*,*,#5964,.T.);
#8553=ORIENTED_EDGE('',*,*,#5965,.T.);
#8554=ORIENTED_EDGE('',*,*,#5955,.F.);
#8555=ORIENTED_EDGE('',*,*,#5966,.F.);
#8556=ORIENTED_EDGE('',*,*,#5964,.F.);
#8557=ORIENTED_EDGE('',*,*,#5959,.T.);
#8558=ORIENTED_EDGE('',*,*,#5954,.F.);
#8559=ORIENTED_EDGE('',*,*,#5958,.F.);
#8560=ORIENTED_EDGE('',*,*,#5967,.F.);
#8561=ORIENTED_EDGE('',*,*,#5968,.F.);
#8562=ORIENTED_EDGE('',*,*,#5965,.F.);
#8563=ORIENTED_EDGE('',*,*,#5966,.T.);
#8564=ORIENTED_EDGE('',*,*,#5870,.F.);
#8565=ORIENTED_EDGE('',*,*,#5969,.F.);
#8566=ORIENTED_EDGE('',*,*,#5961,.T.);
#8567=ORIENTED_EDGE('',*,*,#5970,.F.);
#8568=ORIENTED_EDGE('',*,*,#5971,.F.);
#8569=ORIENTED_EDGE('',*,*,#5972,.T.);
#8570=ORIENTED_EDGE('',*,*,#5973,.T.);
#8571=ORIENTED_EDGE('',*,*,#5858,.F.);
#8572=ORIENTED_EDGE('',*,*,#5892,.F.);
#8573=ORIENTED_EDGE('',*,*,#5974,.F.);
#8574=ORIENTED_EDGE('',*,*,#5975,.T.);
#8575=ORIENTED_EDGE('',*,*,#5976,.F.);
#8576=ORIENTED_EDGE('',*,*,#5968,.T.);
#8577=ORIENTED_EDGE('',*,*,#5977,.F.);
#8578=ORIENTED_EDGE('',*,*,#5916,.F.);
#8579=ORIENTED_EDGE('',*,*,#5978,.F.);
#8580=ORIENTED_EDGE('',*,*,#5979,.T.);
#8581=ORIENTED_EDGE('',*,*,#5919,.T.);
#8582=ORIENTED_EDGE('',*,*,#5915,.F.);
#8583=ORIENTED_EDGE('',*,*,#5918,.F.);
#8584=ORIENTED_EDGE('',*,*,#5899,.F.);
#8585=ORIENTED_EDGE('',*,*,#5910,.F.);
#8586=ORIENTED_EDGE('',*,*,#5980,.T.);
#8587=ORIENTED_EDGE('',*,*,#5978,.T.);
#8588=ORIENTED_EDGE('',*,*,#5981,.F.);
#8589=ORIENTED_EDGE('',*,*,#5920,.F.);
#8590=ORIENTED_EDGE('',*,*,#5979,.F.);
#8591=ORIENTED_EDGE('',*,*,#5980,.F.);
#8592=ORIENTED_EDGE('',*,*,#5921,.T.);
#8593=ORIENTED_EDGE('',*,*,#5982,.F.);
#8594=ORIENTED_EDGE('',*,*,#5983,.T.);
#8595=ORIENTED_EDGE('',*,*,#5902,.F.);
#8596=ORIENTED_EDGE('',*,*,#5943,.F.);
#8597=ORIENTED_EDGE('',*,*,#5949,.F.);
#8598=ORIENTED_EDGE('',*,*,#5984,.F.);
#8599=ORIENTED_EDGE('',*,*,#5985,.T.);
#8600=ORIENTED_EDGE('',*,*,#5986,.F.);
#8601=ORIENTED_EDGE('',*,*,#5987,.T.);
#8602=ORIENTED_EDGE('',*,*,#5984,.T.);
#8603=ORIENTED_EDGE('',*,*,#5948,.T.);
#8604=ORIENTED_EDGE('',*,*,#5988,.F.);
#8605=ORIENTED_EDGE('',*,*,#5929,.T.);
#8606=ORIENTED_EDGE('',*,*,#5989,.T.);
#8607=ORIENTED_EDGE('',*,*,#5990,.T.);
#8608=ORIENTED_EDGE('',*,*,#5925,.F.);
#8609=ORIENTED_EDGE('',*,*,#5991,.F.);
#8610=ORIENTED_EDGE('',*,*,#5989,.F.);
#8611=ORIENTED_EDGE('',*,*,#5928,.T.);
#8612=ORIENTED_EDGE('',*,*,#5924,.F.);
#8613=ORIENTED_EDGE('',*,*,#5927,.F.);
#8614=ORIENTED_EDGE('',*,*,#5903,.F.);
#8615=ORIENTED_EDGE('',*,*,#5983,.F.);
#8616=ORIENTED_EDGE('',*,*,#5990,.F.);
#8617=ORIENTED_EDGE('',*,*,#5991,.T.);
#8618=ORIENTED_EDGE('',*,*,#5933,.F.);
#8619=ORIENTED_EDGE('',*,*,#5938,.F.);
#8620=ORIENTED_EDGE('',*,*,#5992,.T.);
#8621=ORIENTED_EDGE('',*,*,#5993,.T.);
#8622=ORIENTED_EDGE('',*,*,#5994,.T.);
#8623=ORIENTED_EDGE('',*,*,#5995,.F.);
#8624=ORIENTED_EDGE('',*,*,#5992,.F.);
#8625=ORIENTED_EDGE('',*,*,#5937,.F.);
#8626=ORIENTED_EDGE('',*,*,#5911,.T.);
#8627=ORIENTED_EDGE('',*,*,#5996,.T.);
#8628=ORIENTED_EDGE('',*,*,#5997,.F.);
#8629=ORIENTED_EDGE('',*,*,#5996,.F.);
#8630=ORIENTED_EDGE('',*,*,#5998,.F.);
#8631=ORIENTED_EDGE('',*,*,#5999,.T.);
#8632=ORIENTED_EDGE('',*,*,#6000,.F.);
#8633=ORIENTED_EDGE('',*,*,#5999,.F.);
#8634=ORIENTED_EDGE('',*,*,#5997,.T.);
#8635=ORIENTED_EDGE('',*,*,#6000,.T.);
#8636=ORIENTED_EDGE('',*,*,#6001,.T.);
#8637=ORIENTED_EDGE('',*,*,#6002,.F.);
#8638=ORIENTED_EDGE('',*,*,#6003,.F.);
#8639=ORIENTED_EDGE('',*,*,#6004,.F.);
#8640=ORIENTED_EDGE('',*,*,#6005,.T.);
#8641=ORIENTED_EDGE('',*,*,#6006,.F.);
#8642=ORIENTED_EDGE('',*,*,#5998,.T.);
#8643=ORIENTED_EDGE('',*,*,#6001,.F.);
#8644=ORIENTED_EDGE('',*,*,#6007,.T.);
#8645=ORIENTED_EDGE('',*,*,#5912,.F.);
#8646=ORIENTED_EDGE('',*,*,#6007,.F.);
#8647=ORIENTED_EDGE('',*,*,#6008,.F.);
#8648=ORIENTED_EDGE('',*,*,#5970,.T.);
#8649=ORIENTED_EDGE('',*,*,#5963,.T.);
#8650=ORIENTED_EDGE('',*,*,#5976,.T.);
#8651=ORIENTED_EDGE('',*,*,#6009,.T.);
#8652=ORIENTED_EDGE('',*,*,#6004,.T.);
#8653=ORIENTED_EDGE('',*,*,#5859,.F.);
#8654=ORIENTED_EDGE('',*,*,#5977,.T.);
#8655=ORIENTED_EDGE('',*,*,#5967,.T.);
#8656=ORIENTED_EDGE('',*,*,#5957,.F.);
#8657=ORIENTED_EDGE('',*,*,#5962,.F.);
#8658=ORIENTED_EDGE('',*,*,#5969,.T.);
#8659=ORIENTED_EDGE('',*,*,#5872,.F.);
#8660=ORIENTED_EDGE('',*,*,#5816,.F.);
#8661=ORIENTED_EDGE('',*,*,#5820,.F.);
#8662=ORIENTED_EDGE('',*,*,#5883,.F.);
#8663=ORIENTED_EDGE('',*,*,#5854,.F.);
#8664=ORIENTED_EDGE('',*,*,#5857,.F.);
#8665=ORIENTED_EDGE('',*,*,#6010,.F.);
#8666=ORIENTED_EDGE('',*,*,#5994,.F.);
#8667=ORIENTED_EDGE('',*,*,#5936,.F.);
#8668=ORIENTED_EDGE('',*,*,#6011,.F.);
#8669=ORIENTED_EDGE('',*,*,#6012,.F.);
#8670=ORIENTED_EDGE('',*,*,#5896,.F.);
#8671=ORIENTED_EDGE('',*,*,#6013,.F.);
#8672=ORIENTED_EDGE('',*,*,#6005,.F.);
#8673=ORIENTED_EDGE('',*,*,#6009,.F.);
#8674=ORIENTED_EDGE('',*,*,#5975,.F.);
#8675=ORIENTED_EDGE('',*,*,#6014,.F.);
#8676=ORIENTED_EDGE('',*,*,#6015,.F.);
#8677=ORIENTED_EDGE('',*,*,#6012,.T.);
#8678=ORIENTED_EDGE('',*,*,#6016,.T.);
#8679=ORIENTED_EDGE('',*,*,#5885,.F.);
#8680=ORIENTED_EDGE('',*,*,#5897,.F.);
#8681=ORIENTED_EDGE('',*,*,#6011,.T.);
#8682=ORIENTED_EDGE('',*,*,#5935,.T.);
#8683=ORIENTED_EDGE('',*,*,#5886,.F.);
#8684=ORIENTED_EDGE('',*,*,#6016,.F.);
#8685=ORIENTED_EDGE('',*,*,#5930,.F.);
#8686=ORIENTED_EDGE('',*,*,#5993,.F.);
#8687=ORIENTED_EDGE('',*,*,#5995,.T.);
#8688=ORIENTED_EDGE('',*,*,#6010,.T.);
#8689=ORIENTED_EDGE('',*,*,#6017,.T.);
#8690=ORIENTED_EDGE('',*,*,#5889,.T.);
#8691=ORIENTED_EDGE('',*,*,#5939,.F.);
#8692=ORIENTED_EDGE('',*,*,#6014,.T.);
#8693=ORIENTED_EDGE('',*,*,#5974,.T.);
#8694=ORIENTED_EDGE('',*,*,#5891,.F.);
#8695=ORIENTED_EDGE('',*,*,#6018,.F.);
#8696=ORIENTED_EDGE('',*,*,#6015,.T.);
#8697=ORIENTED_EDGE('',*,*,#6018,.T.);
#8698=ORIENTED_EDGE('',*,*,#5890,.F.);
#8699=ORIENTED_EDGE('',*,*,#6017,.F.);
#8700=ORIENTED_EDGE('',*,*,#6013,.T.);
#8701=ORIENTED_EDGE('',*,*,#5895,.T.);
#8702=ORIENTED_EDGE('',*,*,#5988,.T.);
#8703=ORIENTED_EDGE('',*,*,#5982,.T.);
#8704=ORIENTED_EDGE('',*,*,#5981,.T.);
#8705=ORIENTED_EDGE('',*,*,#5909,.T.);
#8706=ORIENTED_EDGE('',*,*,#6019,.F.);
#8707=ORIENTED_EDGE('',*,*,#6002,.T.);
#8708=ORIENTED_EDGE('',*,*,#6006,.T.);
#8709=ORIENTED_EDGE('',*,*,#6020,.F.);
#8710=ORIENTED_EDGE('',*,*,#5946,.T.);
#8711=ORIENTED_EDGE('',*,*,#6021,.F.);
#8712=ORIENTED_EDGE('',*,*,#6022,.F.);
#8713=ORIENTED_EDGE('',*,*,#6023,.F.);
#8714=ORIENTED_EDGE('',*,*,#6022,.T.);
#8715=ORIENTED_EDGE('',*,*,#6024,.F.);
#8716=ORIENTED_EDGE('',*,*,#5972,.F.);
#8717=ORIENTED_EDGE('',*,*,#6025,.T.);
#8718=ORIENTED_EDGE('',*,*,#5907,.T.);
#8719=ORIENTED_EDGE('',*,*,#6026,.F.);
#8720=ORIENTED_EDGE('',*,*,#6027,.F.);
#8721=ORIENTED_EDGE('',*,*,#6028,.F.);
#8722=ORIENTED_EDGE('',*,*,#6027,.T.);
#8723=ORIENTED_EDGE('',*,*,#6029,.F.);
#8724=ORIENTED_EDGE('',*,*,#6030,.F.);
#8725=ORIENTED_EDGE('',*,*,#5940,.F.);
#8726=ORIENTED_EDGE('',*,*,#5985,.F.);
#8727=ORIENTED_EDGE('',*,*,#5987,.F.);
#8728=ORIENTED_EDGE('',*,*,#6031,.F.);
#8729=ORIENTED_EDGE('',*,*,#6030,.T.);
#8730=ORIENTED_EDGE('',*,*,#6032,.T.);
#8731=ORIENTED_EDGE('',*,*,#5950,.F.);
#8732=ORIENTED_EDGE('',*,*,#5871,.F.);
#8733=ORIENTED_EDGE('',*,*,#5973,.F.);
#8734=ORIENTED_EDGE('',*,*,#6024,.T.);
#8735=ORIENTED_EDGE('',*,*,#6021,.T.);
#8736=ORIENTED_EDGE('',*,*,#5945,.T.);
#8737=ORIENTED_EDGE('',*,*,#5951,.F.);
#8738=ORIENTED_EDGE('',*,*,#6032,.F.);
#8739=ORIENTED_EDGE('',*,*,#6029,.T.);
#8740=ORIENTED_EDGE('',*,*,#6026,.T.);
#8741=ORIENTED_EDGE('',*,*,#5906,.T.);
#8742=ORIENTED_EDGE('',*,*,#5877,.F.);
#8743=ORIENTED_EDGE('',*,*,#5806,.F.);
#8744=ORIENTED_EDGE('',*,*,#5874,.F.);
#8745=ORIENTED_EDGE('',*,*,#5881,.F.);
#8746=ORIENTED_EDGE('',*,*,#5810,.F.);
#8747=ORIENTED_EDGE('',*,*,#5814,.F.);
#8748=ORIENTED_EDGE('',*,*,#5947,.F.);
#8749=ORIENTED_EDGE('',*,*,#6020,.T.);
#8750=ORIENTED_EDGE('',*,*,#6023,.T.);
#8751=ORIENTED_EDGE('',*,*,#5971,.T.);
#8752=ORIENTED_EDGE('',*,*,#6008,.T.);
#8753=ORIENTED_EDGE('',*,*,#6003,.T.);
#8754=ORIENTED_EDGE('',*,*,#6019,.T.);
#8755=ORIENTED_EDGE('',*,*,#5908,.T.);
#8756=ORIENTED_EDGE('',*,*,#6025,.F.);
#8757=ORIENTED_EDGE('',*,*,#6028,.T.);
#8758=ORIENTED_EDGE('',*,*,#6031,.T.);
#8759=ORIENTED_EDGE('',*,*,#5986,.T.);
#8760=ORIENTED_EDGE('',*,*,#6033,.T.);
#8761=ORIENTED_EDGE('',*,*,#6034,.T.);
#8762=ORIENTED_EDGE('',*,*,#6035,.T.);
#8763=ORIENTED_EDGE('',*,*,#6034,.F.);
#8764=ORIENTED_EDGE('',*,*,#6036,.F.);
#8765=ORIENTED_EDGE('',*,*,#6037,.T.);
#8766=ORIENTED_EDGE('',*,*,#6033,.F.);
#8767=ORIENTED_EDGE('',*,*,#6037,.F.);
#8768=ORIENTED_EDGE('',*,*,#6035,.F.);
#8769=ORIENTED_EDGE('',*,*,#6036,.T.);
#8770=ORIENTED_EDGE('',*,*,#6038,.F.);
#8771=ORIENTED_EDGE('',*,*,#6039,.T.);
#8772=ORIENTED_EDGE('',*,*,#6040,.T.);
#8773=ORIENTED_EDGE('',*,*,#6041,.F.);
#8774=ORIENTED_EDGE('',*,*,#6042,.F.);
#8775=ORIENTED_EDGE('',*,*,#6043,.T.);
#8776=ORIENTED_EDGE('',*,*,#6038,.T.);
#8777=ORIENTED_EDGE('',*,*,#6044,.F.);
#8778=ORIENTED_EDGE('',*,*,#6045,.F.);
#8779=ORIENTED_EDGE('',*,*,#6046,.T.);
#8780=ORIENTED_EDGE('',*,*,#6042,.T.);
#8781=ORIENTED_EDGE('',*,*,#6047,.F.);
#8782=ORIENTED_EDGE('',*,*,#6048,.F.);
#8783=ORIENTED_EDGE('',*,*,#6049,.T.);
#8784=ORIENTED_EDGE('',*,*,#6045,.T.);
#8785=ORIENTED_EDGE('',*,*,#6050,.F.);
#8786=ORIENTED_EDGE('',*,*,#6051,.F.);
#8787=ORIENTED_EDGE('',*,*,#6052,.T.);
#8788=ORIENTED_EDGE('',*,*,#6048,.T.);
#8789=ORIENTED_EDGE('',*,*,#6053,.F.);
#8790=ORIENTED_EDGE('',*,*,#6054,.F.);
#8791=ORIENTED_EDGE('',*,*,#6055,.T.);
#8792=ORIENTED_EDGE('',*,*,#6051,.T.);
#8793=ORIENTED_EDGE('',*,*,#6056,.F.);
#8794=ORIENTED_EDGE('',*,*,#6057,.F.);
#8795=ORIENTED_EDGE('',*,*,#6058,.T.);
#8796=ORIENTED_EDGE('',*,*,#6054,.T.);
#8797=ORIENTED_EDGE('',*,*,#6059,.F.);
#8798=ORIENTED_EDGE('',*,*,#6060,.F.);
#8799=ORIENTED_EDGE('',*,*,#6061,.T.);
#8800=ORIENTED_EDGE('',*,*,#6057,.T.);
#8801=ORIENTED_EDGE('',*,*,#6062,.F.);
#8802=ORIENTED_EDGE('',*,*,#6063,.F.);
#8803=ORIENTED_EDGE('',*,*,#6064,.T.);
#8804=ORIENTED_EDGE('',*,*,#6060,.T.);
#8805=ORIENTED_EDGE('',*,*,#6065,.F.);
#8806=ORIENTED_EDGE('',*,*,#6066,.F.);
#8807=ORIENTED_EDGE('',*,*,#6067,.T.);
#8808=ORIENTED_EDGE('',*,*,#6063,.T.);
#8809=ORIENTED_EDGE('',*,*,#6068,.F.);
#8810=ORIENTED_EDGE('',*,*,#6069,.F.);
#8811=ORIENTED_EDGE('',*,*,#6070,.T.);
#8812=ORIENTED_EDGE('',*,*,#6066,.T.);
#8813=ORIENTED_EDGE('',*,*,#6071,.F.);
#8814=ORIENTED_EDGE('',*,*,#6072,.F.);
#8815=ORIENTED_EDGE('',*,*,#6073,.T.);
#8816=ORIENTED_EDGE('',*,*,#6069,.T.);
#8817=ORIENTED_EDGE('',*,*,#6074,.F.);
#8818=ORIENTED_EDGE('',*,*,#6075,.F.);
#8819=ORIENTED_EDGE('',*,*,#6076,.T.);
#8820=ORIENTED_EDGE('',*,*,#6072,.T.);
#8821=ORIENTED_EDGE('',*,*,#6077,.F.);
#8822=ORIENTED_EDGE('',*,*,#6078,.F.);
#8823=ORIENTED_EDGE('',*,*,#6079,.T.);
#8824=ORIENTED_EDGE('',*,*,#6075,.T.);
#8825=ORIENTED_EDGE('',*,*,#6080,.F.);
#8826=ORIENTED_EDGE('',*,*,#6081,.F.);
#8827=ORIENTED_EDGE('',*,*,#6082,.T.);
#8828=ORIENTED_EDGE('',*,*,#6078,.T.);
#8829=ORIENTED_EDGE('',*,*,#6083,.F.);
#8830=ORIENTED_EDGE('',*,*,#6084,.F.);
#8831=ORIENTED_EDGE('',*,*,#6085,.F.);
#8832=ORIENTED_EDGE('',*,*,#6086,.F.);
#8833=ORIENTED_EDGE('',*,*,#6087,.T.);
#8834=ORIENTED_EDGE('',*,*,#6088,.F.);
#8835=ORIENTED_EDGE('',*,*,#6089,.F.);
#8836=ORIENTED_EDGE('',*,*,#6084,.T.);
#8837=ORIENTED_EDGE('',*,*,#6090,.T.);
#8838=ORIENTED_EDGE('',*,*,#6091,.F.);
#8839=ORIENTED_EDGE('',*,*,#6092,.F.);
#8840=ORIENTED_EDGE('',*,*,#6088,.T.);
#8841=ORIENTED_EDGE('',*,*,#6093,.T.);
#8842=ORIENTED_EDGE('',*,*,#6094,.F.);
#8843=ORIENTED_EDGE('',*,*,#6095,.F.);
#8844=ORIENTED_EDGE('',*,*,#6091,.T.);
#8845=ORIENTED_EDGE('',*,*,#6096,.T.);
#8846=ORIENTED_EDGE('',*,*,#6097,.F.);
#8847=ORIENTED_EDGE('',*,*,#6098,.F.);
#8848=ORIENTED_EDGE('',*,*,#6094,.T.);
#8849=ORIENTED_EDGE('',*,*,#6099,.T.);
#8850=ORIENTED_EDGE('',*,*,#6100,.F.);
#8851=ORIENTED_EDGE('',*,*,#6101,.F.);
#8852=ORIENTED_EDGE('',*,*,#6097,.T.);
#8853=ORIENTED_EDGE('',*,*,#6102,.T.);
#8854=ORIENTED_EDGE('',*,*,#6103,.F.);
#8855=ORIENTED_EDGE('',*,*,#6104,.F.);
#8856=ORIENTED_EDGE('',*,*,#6100,.T.);
#8857=ORIENTED_EDGE('',*,*,#6105,.T.);
#8858=ORIENTED_EDGE('',*,*,#6106,.F.);
#8859=ORIENTED_EDGE('',*,*,#6107,.F.);
#8860=ORIENTED_EDGE('',*,*,#6103,.T.);
#8861=ORIENTED_EDGE('',*,*,#6108,.T.);
#8862=ORIENTED_EDGE('',*,*,#6109,.F.);
#8863=ORIENTED_EDGE('',*,*,#6110,.F.);
#8864=ORIENTED_EDGE('',*,*,#6106,.T.);
#8865=ORIENTED_EDGE('',*,*,#6111,.T.);
#8866=ORIENTED_EDGE('',*,*,#6112,.F.);
#8867=ORIENTED_EDGE('',*,*,#6113,.F.);
#8868=ORIENTED_EDGE('',*,*,#6109,.T.);
#8869=ORIENTED_EDGE('',*,*,#6114,.T.);
#8870=ORIENTED_EDGE('',*,*,#6115,.F.);
#8871=ORIENTED_EDGE('',*,*,#6116,.F.);
#8872=ORIENTED_EDGE('',*,*,#6112,.T.);
#8873=ORIENTED_EDGE('',*,*,#6117,.T.);
#8874=ORIENTED_EDGE('',*,*,#6118,.F.);
#8875=ORIENTED_EDGE('',*,*,#6119,.F.);
#8876=ORIENTED_EDGE('',*,*,#6115,.T.);
#8877=ORIENTED_EDGE('',*,*,#6120,.T.);
#8878=ORIENTED_EDGE('',*,*,#6121,.F.);
#8879=ORIENTED_EDGE('',*,*,#6122,.F.);
#8880=ORIENTED_EDGE('',*,*,#6118,.T.);
#8881=ORIENTED_EDGE('',*,*,#6123,.T.);
#8882=ORIENTED_EDGE('',*,*,#6124,.F.);
#8883=ORIENTED_EDGE('',*,*,#6125,.F.);
#8884=ORIENTED_EDGE('',*,*,#6121,.T.);
#8885=ORIENTED_EDGE('',*,*,#6126,.T.);
#8886=ORIENTED_EDGE('',*,*,#6127,.F.);
#8887=ORIENTED_EDGE('',*,*,#6128,.F.);
#8888=ORIENTED_EDGE('',*,*,#6124,.T.);
#8889=ORIENTED_EDGE('',*,*,#6129,.T.);
#8890=ORIENTED_EDGE('',*,*,#6130,.F.);
#8891=ORIENTED_EDGE('',*,*,#6131,.F.);
#8892=ORIENTED_EDGE('',*,*,#6127,.T.);
#8893=ORIENTED_EDGE('',*,*,#6132,.T.);
#8894=ORIENTED_EDGE('',*,*,#6130,.T.);
#8895=ORIENTED_EDGE('',*,*,#6133,.T.);
#8896=ORIENTED_EDGE('',*,*,#6134,.T.);
#8897=ORIENTED_EDGE('',*,*,#6135,.F.);
#8898=ORIENTED_EDGE('',*,*,#6081,.T.);
#8899=ORIENTED_EDGE('',*,*,#6136,.F.);
#8900=ORIENTED_EDGE('',*,*,#6137,.T.);
#8901=ORIENTED_EDGE('',*,*,#6138,.T.);
#8902=ORIENTED_EDGE('',*,*,#6139,.F.);
#8903=ORIENTED_EDGE('',*,*,#6140,.T.);
#8904=ORIENTED_EDGE('',*,*,#6141,.F.);
#8905=ORIENTED_EDGE('',*,*,#6142,.T.);
#8906=ORIENTED_EDGE('',*,*,#6143,.T.);
#8907=ORIENTED_EDGE('',*,*,#6142,.F.);
#8908=ORIENTED_EDGE('',*,*,#6141,.T.);
#8909=ORIENTED_EDGE('',*,*,#6144,.F.);
#8910=ORIENTED_EDGE('',*,*,#6145,.T.);
#8911=ORIENTED_EDGE('',*,*,#6146,.T.);
#8912=ORIENTED_EDGE('',*,*,#6147,.F.);
#8913=ORIENTED_EDGE('',*,*,#6146,.F.);
#8914=ORIENTED_EDGE('',*,*,#6148,.T.);
#8915=ORIENTED_EDGE('',*,*,#6086,.T.);
#8916=ORIENTED_EDGE('',*,*,#6149,.T.);
#8917=ORIENTED_EDGE('',*,*,#6137,.F.);
#8918=ORIENTED_EDGE('',*,*,#6147,.T.);
#8919=ORIENTED_EDGE('',*,*,#6136,.T.);
#8920=ORIENTED_EDGE('',*,*,#6083,.T.);
#8921=ORIENTED_EDGE('',*,*,#6080,.T.);
#8922=ORIENTED_EDGE('',*,*,#6077,.T.);
#8923=ORIENTED_EDGE('',*,*,#6074,.T.);
#8924=ORIENTED_EDGE('',*,*,#6071,.T.);
#8925=ORIENTED_EDGE('',*,*,#6068,.T.);
#8926=ORIENTED_EDGE('',*,*,#6065,.T.);
#8927=ORIENTED_EDGE('',*,*,#6062,.T.);
#8928=ORIENTED_EDGE('',*,*,#6059,.T.);
#8929=ORIENTED_EDGE('',*,*,#6056,.T.);
#8930=ORIENTED_EDGE('',*,*,#6053,.T.);
#8931=ORIENTED_EDGE('',*,*,#6050,.T.);
#8932=ORIENTED_EDGE('',*,*,#6047,.T.);
#8933=ORIENTED_EDGE('',*,*,#6044,.T.);
#8934=ORIENTED_EDGE('',*,*,#6041,.T.);
#8935=ORIENTED_EDGE('',*,*,#6150,.T.);
#8936=ORIENTED_EDGE('',*,*,#6133,.F.);
#8937=ORIENTED_EDGE('',*,*,#6132,.F.);
#8938=ORIENTED_EDGE('',*,*,#6129,.F.);
#8939=ORIENTED_EDGE('',*,*,#6126,.F.);
#8940=ORIENTED_EDGE('',*,*,#6123,.F.);
#8941=ORIENTED_EDGE('',*,*,#6120,.F.);
#8942=ORIENTED_EDGE('',*,*,#6117,.F.);
#8943=ORIENTED_EDGE('',*,*,#6114,.F.);
#8944=ORIENTED_EDGE('',*,*,#6111,.F.);
#8945=ORIENTED_EDGE('',*,*,#6108,.F.);
#8946=ORIENTED_EDGE('',*,*,#6105,.F.);
#8947=ORIENTED_EDGE('',*,*,#6102,.F.);
#8948=ORIENTED_EDGE('',*,*,#6099,.F.);
#8949=ORIENTED_EDGE('',*,*,#6096,.F.);
#8950=ORIENTED_EDGE('',*,*,#6093,.F.);
#8951=ORIENTED_EDGE('',*,*,#6090,.F.);
#8952=ORIENTED_EDGE('',*,*,#6087,.F.);
#8953=ORIENTED_EDGE('',*,*,#6148,.F.);
#8954=ORIENTED_EDGE('',*,*,#6145,.F.);
#8955=ORIENTED_EDGE('',*,*,#6085,.T.);
#8956=ORIENTED_EDGE('',*,*,#6089,.T.);
#8957=ORIENTED_EDGE('',*,*,#6092,.T.);
#8958=ORIENTED_EDGE('',*,*,#6095,.T.);
#8959=ORIENTED_EDGE('',*,*,#6098,.T.);
#8960=ORIENTED_EDGE('',*,*,#6101,.T.);
#8961=ORIENTED_EDGE('',*,*,#6104,.T.);
#8962=ORIENTED_EDGE('',*,*,#6107,.T.);
#8963=ORIENTED_EDGE('',*,*,#6110,.T.);
#8964=ORIENTED_EDGE('',*,*,#6113,.T.);
#8965=ORIENTED_EDGE('',*,*,#6116,.T.);
#8966=ORIENTED_EDGE('',*,*,#6119,.T.);
#8967=ORIENTED_EDGE('',*,*,#6122,.T.);
#8968=ORIENTED_EDGE('',*,*,#6125,.T.);
#8969=ORIENTED_EDGE('',*,*,#6128,.T.);
#8970=ORIENTED_EDGE('',*,*,#6131,.T.);
#8971=ORIENTED_EDGE('',*,*,#6135,.T.);
#8972=ORIENTED_EDGE('',*,*,#6151,.T.);
#8973=ORIENTED_EDGE('',*,*,#6039,.F.);
#8974=ORIENTED_EDGE('',*,*,#6043,.F.);
#8975=ORIENTED_EDGE('',*,*,#6046,.F.);
#8976=ORIENTED_EDGE('',*,*,#6049,.F.);
#8977=ORIENTED_EDGE('',*,*,#6052,.F.);
#8978=ORIENTED_EDGE('',*,*,#6055,.F.);
#8979=ORIENTED_EDGE('',*,*,#6058,.F.);
#8980=ORIENTED_EDGE('',*,*,#6061,.F.);
#8981=ORIENTED_EDGE('',*,*,#6064,.F.);
#8982=ORIENTED_EDGE('',*,*,#6067,.F.);
#8983=ORIENTED_EDGE('',*,*,#6070,.F.);
#8984=ORIENTED_EDGE('',*,*,#6073,.F.);
#8985=ORIENTED_EDGE('',*,*,#6076,.F.);
#8986=ORIENTED_EDGE('',*,*,#6079,.F.);
#8987=ORIENTED_EDGE('',*,*,#6082,.F.);
#8988=ORIENTED_EDGE('',*,*,#6138,.F.);
#8989=ORIENTED_EDGE('',*,*,#6149,.F.);
#8990=ORIENTED_EDGE('',*,*,#6144,.T.);
#8991=ORIENTED_EDGE('',*,*,#6152,.F.);
#8992=ORIENTED_EDGE('',*,*,#6153,.F.);
#8993=ORIENTED_EDGE('',*,*,#6154,.F.);
#8994=ORIENTED_EDGE('',*,*,#6140,.F.);
#8995=ORIENTED_EDGE('',*,*,#6155,.F.);
#8996=ORIENTED_EDGE('',*,*,#6156,.F.);
#8997=ORIENTED_EDGE('',*,*,#6143,.F.);
#8998=ORIENTED_EDGE('',*,*,#6040,.F.);
#8999=ORIENTED_EDGE('',*,*,#6151,.F.);
#9000=ORIENTED_EDGE('',*,*,#6134,.F.);
#9001=ORIENTED_EDGE('',*,*,#6150,.F.);
#9002=ORIENTED_EDGE('',*,*,#6154,.T.);
#9003=ORIENTED_EDGE('',*,*,#6157,.F.);
#9004=ORIENTED_EDGE('',*,*,#6153,.T.);
#9005=ORIENTED_EDGE('',*,*,#6158,.F.);
#9006=ORIENTED_EDGE('',*,*,#6152,.T.);
#9007=ORIENTED_EDGE('',*,*,#6159,.F.);
#9008=ORIENTED_EDGE('',*,*,#6156,.T.);
#9009=ORIENTED_EDGE('',*,*,#6160,.F.);
#9010=ORIENTED_EDGE('',*,*,#6155,.T.);
#9011=ORIENTED_EDGE('',*,*,#6161,.F.);
#9012=ORIENTED_EDGE('',*,*,#6162,.T.);
#9013=ORIENTED_EDGE('',*,*,#6163,.T.);
#9014=ORIENTED_EDGE('',*,*,#6164,.T.);
#9015=ORIENTED_EDGE('',*,*,#6165,.T.);
#9016=ORIENTED_EDGE('',*,*,#6166,.T.);
#9017=ORIENTED_EDGE('',*,*,#6167,.T.);
#9018=ORIENTED_EDGE('',*,*,#6168,.T.);
#9019=ORIENTED_EDGE('',*,*,#6139,.T.);
#9020=ORIENTED_EDGE('',*,*,#6169,.F.);
#9021=ORIENTED_EDGE('',*,*,#6163,.F.);
#9022=ORIENTED_EDGE('',*,*,#6169,.T.);
#9023=ORIENTED_EDGE('',*,*,#6157,.T.);
#9024=ORIENTED_EDGE('',*,*,#6170,.F.);
#9025=ORIENTED_EDGE('',*,*,#6164,.F.);
#9026=ORIENTED_EDGE('',*,*,#6170,.T.);
#9027=ORIENTED_EDGE('',*,*,#6158,.T.);
#9028=ORIENTED_EDGE('',*,*,#6171,.F.);
#9029=ORIENTED_EDGE('',*,*,#6165,.F.);
#9030=ORIENTED_EDGE('',*,*,#6171,.T.);
#9031=ORIENTED_EDGE('',*,*,#6159,.T.);
#9032=ORIENTED_EDGE('',*,*,#6172,.F.);
#9033=ORIENTED_EDGE('',*,*,#6166,.F.);
#9034=ORIENTED_EDGE('',*,*,#6172,.T.);
#9035=ORIENTED_EDGE('',*,*,#6160,.T.);
#9036=ORIENTED_EDGE('',*,*,#6173,.F.);
#9037=ORIENTED_EDGE('',*,*,#6167,.F.);
#9038=ORIENTED_EDGE('',*,*,#6173,.T.);
#9039=ORIENTED_EDGE('',*,*,#6161,.T.);
#9040=ORIENTED_EDGE('',*,*,#6168,.F.);
#9041=ORIENTED_EDGE('',*,*,#6162,.F.);
#9042=ORIENTED_EDGE('',*,*,#6174,.F.);
#9043=ORIENTED_EDGE('',*,*,#6175,.F.);
#9044=ORIENTED_EDGE('',*,*,#6176,.T.);
#9045=ORIENTED_EDGE('',*,*,#6177,.T.);
#9046=ORIENTED_EDGE('',*,*,#6178,.T.);
#9047=ORIENTED_EDGE('',*,*,#6176,.F.);
#9048=ORIENTED_EDGE('',*,*,#6178,.F.);
#9049=ORIENTED_EDGE('',*,*,#6179,.T.);
#9050=ORIENTED_EDGE('',*,*,#6180,.T.);
#9051=ORIENTED_EDGE('',*,*,#6181,.T.);
#9052=ORIENTED_EDGE('',*,*,#6179,.F.);
#9053=ORIENTED_EDGE('',*,*,#6177,.F.);
#9054=ORIENTED_EDGE('',*,*,#6181,.F.);
#9055=ORIENTED_EDGE('',*,*,#6182,.T.);
#9056=ORIENTED_EDGE('',*,*,#6174,.T.);
#9057=ORIENTED_EDGE('',*,*,#6182,.F.);
#9058=ORIENTED_EDGE('',*,*,#6180,.F.);
#9059=ORIENTED_EDGE('',*,*,#6175,.T.);
#9060=ORIENTED_EDGE('',*,*,#6183,.F.);
#9061=ORIENTED_EDGE('',*,*,#6184,.T.);
#9062=ORIENTED_EDGE('',*,*,#6185,.T.);
#9063=ORIENTED_EDGE('',*,*,#6186,.T.);
#9064=ORIENTED_EDGE('',*,*,#6184,.F.);
#9065=ORIENTED_EDGE('',*,*,#6186,.F.);
#9066=ORIENTED_EDGE('',*,*,#6187,.T.);
#9067=ORIENTED_EDGE('',*,*,#6188,.T.);
#9068=ORIENTED_EDGE('',*,*,#6189,.T.);
#9069=ORIENTED_EDGE('',*,*,#6187,.F.);
#9070=ORIENTED_EDGE('',*,*,#6185,.F.);
#9071=ORIENTED_EDGE('',*,*,#6189,.F.);
#9072=ORIENTED_EDGE('',*,*,#6190,.T.);
#9073=ORIENTED_EDGE('',*,*,#6191,.T.);
#9074=ORIENTED_EDGE('',*,*,#6190,.F.);
#9075=ORIENTED_EDGE('',*,*,#6188,.F.);
#9076=ORIENTED_EDGE('',*,*,#6183,.T.);
#9077=ORIENTED_EDGE('',*,*,#6191,.F.);
#9078=ORIENTED_EDGE('',*,*,#6192,.F.);
#9079=ORIENTED_EDGE('',*,*,#6193,.T.);
#9080=ORIENTED_EDGE('',*,*,#6194,.T.);
#9081=ORIENTED_EDGE('',*,*,#6195,.T.);
#9082=ORIENTED_EDGE('',*,*,#6196,.F.);
#9083=ORIENTED_EDGE('',*,*,#6197,.F.);
#9084=ORIENTED_EDGE('',*,*,#6198,.F.);
#9085=ORIENTED_EDGE('',*,*,#6199,.F.);
#9086=ORIENTED_EDGE('',*,*,#6200,.T.);
#9087=ORIENTED_EDGE('',*,*,#6196,.T.);
#9088=ORIENTED_EDGE('',*,*,#6201,.T.);
#9089=ORIENTED_EDGE('',*,*,#6202,.T.);
#9090=ORIENTED_EDGE('',*,*,#6203,.F.);
#9091=ORIENTED_EDGE('',*,*,#6204,.F.);
#9092=ORIENTED_EDGE('',*,*,#6205,.F.);
#9093=ORIENTED_EDGE('',*,*,#6192,.T.);
#9094=ORIENTED_EDGE('',*,*,#6206,.T.);
#9095=ORIENTED_EDGE('',*,*,#6207,.F.);
#9096=ORIENTED_EDGE('',*,*,#6208,.T.);
#9097=ORIENTED_EDGE('',*,*,#6209,.T.);
#9098=ORIENTED_EDGE('',*,*,#6210,.T.);
#9099=ORIENTED_EDGE('',*,*,#6211,.T.);
#9100=ORIENTED_EDGE('',*,*,#6210,.F.);
#9101=ORIENTED_EDGE('',*,*,#6209,.F.);
#9102=ORIENTED_EDGE('',*,*,#6212,.T.);
#9103=ORIENTED_EDGE('',*,*,#6213,.F.);
#9104=ORIENTED_EDGE('',*,*,#6212,.F.);
#9105=ORIENTED_EDGE('',*,*,#6214,.T.);
#9106=ORIENTED_EDGE('',*,*,#6194,.F.);
#9107=ORIENTED_EDGE('',*,*,#6215,.T.);
#9108=ORIENTED_EDGE('',*,*,#6199,.T.);
#9109=ORIENTED_EDGE('',*,*,#6216,.F.);
#9110=ORIENTED_EDGE('',*,*,#6211,.F.);
#9111=ORIENTED_EDGE('',*,*,#6213,.T.);
#9112=ORIENTED_EDGE('',*,*,#6217,.T.);
#9113=ORIENTED_EDGE('',*,*,#6218,.T.);
#9114=ORIENTED_EDGE('',*,*,#6217,.F.);
#9115=ORIENTED_EDGE('',*,*,#6219,.F.);
#9116=ORIENTED_EDGE('',*,*,#6218,.F.);
#9117=ORIENTED_EDGE('',*,*,#6220,.F.);
#9118=ORIENTED_EDGE('',*,*,#6221,.T.);
#9119=ORIENTED_EDGE('',*,*,#6203,.T.);
#9120=ORIENTED_EDGE('',*,*,#6222,.T.);
#9121=ORIENTED_EDGE('',*,*,#6223,.F.);
#9122=ORIENTED_EDGE('',*,*,#6221,.F.);
#9123=ORIENTED_EDGE('',*,*,#6224,.F.);
#9124=ORIENTED_EDGE('',*,*,#6206,.F.);
#9125=ORIENTED_EDGE('',*,*,#6195,.F.);
#9126=ORIENTED_EDGE('',*,*,#6214,.F.);
#9127=ORIENTED_EDGE('',*,*,#6216,.T.);
#9128=ORIENTED_EDGE('',*,*,#6198,.T.);
#9129=ORIENTED_EDGE('',*,*,#6197,.T.);
#9130=ORIENTED_EDGE('',*,*,#6205,.T.);
#9131=ORIENTED_EDGE('',*,*,#6204,.T.);
#9132=ORIENTED_EDGE('',*,*,#6222,.F.);
#9133=ORIENTED_EDGE('',*,*,#6202,.F.);
#9134=ORIENTED_EDGE('',*,*,#6201,.F.);
#9135=ORIENTED_EDGE('',*,*,#6200,.F.);
#9136=ORIENTED_EDGE('',*,*,#6215,.F.);
#9137=ORIENTED_EDGE('',*,*,#6193,.F.);
#9138=ORIENTED_EDGE('',*,*,#6208,.F.);
#9139=ORIENTED_EDGE('',*,*,#6220,.T.);
#9140=ORIENTED_EDGE('',*,*,#6225,.T.);
#9141=ORIENTED_EDGE('',*,*,#6219,.T.);
#9142=ORIENTED_EDGE('',*,*,#6225,.F.);
#9143=ORIENTED_EDGE('',*,*,#6223,.T.);
#9144=ORIENTED_EDGE('',*,*,#6207,.T.);
#9145=ORIENTED_EDGE('',*,*,#6224,.T.);
#9146=CYLINDRICAL_SURFACE('',#10108,0.00125);
#9147=CYLINDRICAL_SURFACE('',#10116,0.000375);
#9148=CYLINDRICAL_SURFACE('',#10124,0.000375);
#9149=CYLINDRICAL_SURFACE('',#10129,0.000375);
#9150=CYLINDRICAL_SURFACE('',#10137,0.000375);
#9151=CYLINDRICAL_SURFACE('',#10146,0.00245);
#9152=CYLINDRICAL_SURFACE('',#10160,0.002);
#9153=CYLINDRICAL_SURFACE('',#10253,0.00345);
#9154=CYLINDRICAL_SURFACE('',#10255,0.00285);
#9155=CYLINDRICAL_SURFACE('',#10259,0.00285);
#9156=CYLINDRICAL_SURFACE('',#10261,0.00285);
#9157=CYLINDRICAL_SURFACE('',#10263,0.00285);
#9158=CYLINDRICAL_SURFACE('',#10266,0.0030735);
#9159=CYLINDRICAL_SURFACE('',#10269,0.0025175);
#9160=CYLINDRICAL_SURFACE('',#10278,0.004);
#9161=CYLINDRICAL_SURFACE('',#10284,0.008);
#9162=CYLINDRICAL_SURFACE('',#10292,0.0021);
#9163=CYLINDRICAL_SURFACE('',#10342,0.01115);
#9164=CYLINDRICAL_SURFACE('',#10344,0.01115);
#9165=CYLINDRICAL_SURFACE('',#10345,0.01115);
#9166=CYLINDRICAL_SURFACE('',#10346,0.01115);
#9167=CYLINDRICAL_SURFACE('',#10347,0.01115);
#9168=CYLINDRICAL_SURFACE('',#10348,0.01115);
#9169=CYLINDRICAL_SURFACE('',#10349,0.01115);
#9170=CYLINDRICAL_SURFACE('',#10350,0.01115);
#9171=CYLINDRICAL_SURFACE('',#10375,0.01115);
#9172=CYLINDRICAL_SURFACE('',#10380,0.01115);
#9173=CYLINDRICAL_SURFACE('',#10385,0.01115);
#9174=CYLINDRICAL_SURFACE('',#10390,0.008);
#9175=CYLINDRICAL_SURFACE('',#10396,0.008);
#9176=CYLINDRICAL_SURFACE('',#10399,0.006);
#9177=CYLINDRICAL_SURFACE('',#10409,0.003875);
#9178=CYLINDRICAL_SURFACE('',#10417,0.00245);
#9179=CYLINDRICAL_SURFACE('',#10420,0.003875);
#9180=CYLINDRICAL_SURFACE('',#10430,0.00075);
#9181=CYLINDRICAL_SURFACE('',#10438,0.00075);
#9182=CYLINDRICAL_SURFACE('',#10441,0.000375);
#9183=CYLINDRICAL_SURFACE('',#10449,0.000375);
#9184=CYLINDRICAL_SURFACE('',#10454,0.000375);
#9185=CYLINDRICAL_SURFACE('',#10462,0.000375);
#9186=CYLINDRICAL_SURFACE('',#10467,0.001543);
#9187=CYLINDRICAL_SURFACE('',#10468,0.001543);
#9188=CYLINDRICAL_SURFACE('',#10469,0.001543);
#9189=CYLINDRICAL_SURFACE('',#10470,0.001543);
#9190=CYLINDRICAL_SURFACE('',#10471,0.001543);
#9191=CYLINDRICAL_SURFACE('',#10472,0.001543);
#9192=CYLINDRICAL_SURFACE('',#10473,0.001543);
#9193=CYLINDRICAL_SURFACE('',#10474,0.001543);
#9194=CYLINDRICAL_SURFACE('',#10476,0.001543);
#9195=CYLINDRICAL_SURFACE('',#10478,0.001543);
#9196=CYLINDRICAL_SURFACE('',#10479,0.001543);
#9197=CYLINDRICAL_SURFACE('',#10480,0.001543);
#9198=CYLINDRICAL_SURFACE('',#10481,0.001543);
#9199=CYLINDRICAL_SURFACE('',#10482,0.001543);
#9200=CYLINDRICAL_SURFACE('',#10483,0.001543);
#9201=CYLINDRICAL_SURFACE('',#10484,0.001543);
#9202=CYLINDRICAL_SURFACE('',#10485,0.001543);
#9203=CYLINDRICAL_SURFACE('',#10486,0.001543);
#9204=CYLINDRICAL_SURFACE('',#10487,0.001543);
#9205=CYLINDRICAL_SURFACE('',#10488,0.001543);
#9206=CYLINDRICAL_SURFACE('',#10489,0.001543);
#9207=CYLINDRICAL_SURFACE('',#10491,0.0012645);
#9208=CYLINDRICAL_SURFACE('',#10492,0.0012645);
#9209=CYLINDRICAL_SURFACE('',#10493,0.0012645);
#9210=CYLINDRICAL_SURFACE('',#10494,0.0012645);
#9211=CYLINDRICAL_SURFACE('',#10495,0.0012645);
#9212=CYLINDRICAL_SURFACE('',#10496,0.0012645);
#9213=CYLINDRICAL_SURFACE('',#10497,0.0012645);
#9214=CYLINDRICAL_SURFACE('',#10499,0.0012645);
#9215=CYLINDRICAL_SURFACE('',#10501,0.0012645);
#9216=CYLINDRICAL_SURFACE('',#10502,0.0012645);
#9217=CYLINDRICAL_SURFACE('',#10503,0.0012645);
#9218=CYLINDRICAL_SURFACE('',#10504,0.0012645);
#9219=CYLINDRICAL_SURFACE('',#10505,0.0012645);
#9220=CYLINDRICAL_SURFACE('',#10506,0.0012645);
#9221=CYLINDRICAL_SURFACE('',#10507,0.0012645);
#9222=CYLINDRICAL_SURFACE('',#10508,0.0012645);
#9223=CYLINDRICAL_SURFACE('',#10509,0.0012645);
#9224=CYLINDRICAL_SURFACE('',#10510,0.0012645);
#9225=CYLINDRICAL_SURFACE('',#10511,0.0012645);
#9226=CYLINDRICAL_SURFACE('',#10513,0.0012645);
#9227=CYLINDRICAL_SURFACE('',#10514,0.0012645);
#9228=CYLINDRICAL_SURFACE('',#10532,0.0015);
#9229=CYLINDRICAL_SURFACE('',#10534,0.003);
#9230=CYLINDRICAL_SURFACE('',#10563,0.0025);
#9231=CYLINDRICAL_SURFACE('',#10577,0.001543);
#9232=CYLINDRICAL_SURFACE('',#10578,0.00155);
#9233=CYLINDRICAL_SURFACE('',#10588,0.003);
#9234=CYLINDRICAL_SURFACE('',#10590,0.001543);
#9235=CYLINDRICAL_SURFACE('',#10597,0.001543);
#9236=CYLINDRICAL_SURFACE('',#10601,0.0012645);
#9237=CYLINDRICAL_SURFACE('',#10602,0.001543);
#9238=CYLINDRICAL_SURFACE('',#10603,0.0012645);
#9239=CYLINDRICAL_SURFACE('',#10604,0.001543);
#9240=CYLINDRICAL_SURFACE('',#10608,0.00025);
#9241=CYLINDRICAL_SURFACE('',#10616,0.00025);
#9242=CYLINDRICAL_SURFACE('',#10621,0.0025);
#9243=CYLINDRICAL_SURFACE('',#10625,0.003);
#9244=CYLINDRICAL_SURFACE('',#10628,0.0025);
#9245=CYLINDRICAL_SURFACE('',#10632,0.003);
#9246=CYLINDRICAL_SURFACE('',#10638,0.001);
#9247=CYLINDRICAL_SURFACE('',#10647,0.0021);
#9248=CYLINDRICAL_SURFACE('',#10652,0.00275);
#9249=CYLINDRICAL_SURFACE('',#10668,0.001475);
#9250=CYLINDRICAL_SURFACE('',#10673,0.003);
#9251=CYLINDRICAL_SURFACE('',#10680,0.0025);
#9252=CYLINDRICAL_SURFACE('',#10682,0.0025);
#9253=CYLINDRICAL_SURFACE('',#10683,0.0025);
#9254=CYLINDRICAL_SURFACE('',#10684,0.0025);
#9255=CYLINDRICAL_SURFACE('',#10685,0.0025);
#9256=CYLINDRICAL_SURFACE('',#10686,0.0025);
#9257=CYLINDRICAL_SURFACE('',#10690,0.0025);
#9258=CYLINDRICAL_SURFACE('',#10691,0.002);
#9259=CYLINDRICAL_SURFACE('',#10734,0.0002);
#9260=CYLINDRICAL_SURFACE('',#10741,0.001);
#9261=CYLINDRICAL_SURFACE('',#10791,0.00075);
#9262=CYLINDRICAL_SURFACE('',#10795,0.00075);
#9263=CYLINDRICAL_SURFACE('',#10797,0.00075);
#9264=CYLINDRICAL_SURFACE('',#10800,0.00075);
#9265=CYLINDRICAL_SURFACE('',#10804,0.00075);
#9266=CYLINDRICAL_SURFACE('',#10806,0.00075);
#9267=CYLINDRICAL_SURFACE('',#10807,0.00075);
#9268=CYLINDRICAL_SURFACE('',#10808,0.00075);
#9269=CYLINDRICAL_SURFACE('',#10818,0.001);
#9270=CYLINDRICAL_SURFACE('',#10823,0.001);
#9271=CYLINDRICAL_SURFACE('',#10828,0.001);
#9272=CYLINDRICAL_SURFACE('',#10833,0.001);
#9273=CYLINDRICAL_SURFACE('',#10838,0.001);
#9274=CYLINDRICAL_SURFACE('',#10862,0.0041);
#9275=CYLINDRICAL_SURFACE('',#10868,0.0025);
#9276=CYLINDRICAL_SURFACE('',#10875,0.003);
#9277=CYLINDRICAL_SURFACE('',#10878,0.00155);
#9278=CYLINDRICAL_SURFACE('',#10880,0.00155);
#9279=CYLINDRICAL_SURFACE('',#10885,0.003);
#9280=CYLINDRICAL_SURFACE('',#10895,0.0015);
#9281=CYLINDRICAL_SURFACE('',#10900,0.0015);
#9282=CYLINDRICAL_SURFACE('',#10902,0.0015);
#9283=CYLINDRICAL_SURFACE('',#10903,0.0015);
#9284=CYLINDRICAL_SURFACE('',#10904,0.0015);
#9285=CYLINDRICAL_SURFACE('',#10905,0.0015);
#9286=CYLINDRICAL_SURFACE('',#10906,0.0015);
#9287=CYLINDRICAL_SURFACE('',#10907,0.0015);
#9288=CYLINDRICAL_SURFACE('',#10908,0.0015);
#9289=CYLINDRICAL_SURFACE('',#10909,0.0015);
#9290=CYLINDRICAL_SURFACE('',#10910,0.0015);
#9291=CYLINDRICAL_SURFACE('',#10911,0.0015);
#9292=CYLINDRICAL_SURFACE('',#10912,0.0015);
#9293=CYLINDRICAL_SURFACE('',#10913,0.0015);
#9294=CYLINDRICAL_SURFACE('',#10914,0.0015);
#9295=CYLINDRICAL_SURFACE('',#10915,0.0015);
#9296=CYLINDRICAL_SURFACE('',#10916,0.00117524047358083);
#9297=CYLINDRICAL_SURFACE('',#10918,0.00117524047358083);
#9298=CYLINDRICAL_SURFACE('',#10919,0.00117524047358083);
#9299=CYLINDRICAL_SURFACE('',#10920,0.00117524047358083);
#9300=CYLINDRICAL_SURFACE('',#10921,0.00117524047358083);
#9301=CYLINDRICAL_SURFACE('',#10922,0.00117524047358083);
#9302=CYLINDRICAL_SURFACE('',#10923,0.00117524047358083);
#9303=CYLINDRICAL_SURFACE('',#10924,0.00117524047358083);
#9304=CYLINDRICAL_SURFACE('',#10925,0.00117524047358083);
#9305=CYLINDRICAL_SURFACE('',#10926,0.00117524047358083);
#9306=CYLINDRICAL_SURFACE('',#10927,0.00117524047358083);
#9307=CYLINDRICAL_SURFACE('',#10928,0.00117524047358083);
#9308=CYLINDRICAL_SURFACE('',#10929,0.00117524047358083);
#9309=CYLINDRICAL_SURFACE('',#10930,0.00117524047358083);
#9310=CYLINDRICAL_SURFACE('',#10931,0.00117524047358083);
#9311=CYLINDRICAL_SURFACE('',#10932,0.00117524047358083);
#9312=CYLINDRICAL_SURFACE('',#10933,0.00117524047358083);
#9313=CYLINDRICAL_SURFACE('',#10935,0.0015);
#9314=CYLINDRICAL_SURFACE('',#10939,0.00285);
#9315=CYLINDRICAL_SURFACE('',#10969,0.00075);
#9316=CYLINDRICAL_SURFACE('',#10977,0.00075);
#9317=CYLINDRICAL_SURFACE('',#10980,0.00025);
#9318=CYLINDRICAL_SURFACE('',#10988,0.00025);
#9319=CYLINDRICAL_SURFACE('',#10993,0.004442);
#9320=CYLINDRICAL_SURFACE('',#10995,0.003872);
#9321=CYLINDRICAL_SURFACE('',#10997,0.003872);
#9322=CYLINDRICAL_SURFACE('',#10999,0.004442);
#9323=CYLINDRICAL_SURFACE('',#11004,0.0025);
#9324=ADVANCED_FACE('',(#1102),#9146,.T.);
#9325=ADVANCED_FACE('',(#1103),#860,.T.);
#9326=ADVANCED_FACE('',(#1104),#861,.F.);
#9327=ADVANCED_FACE('',(#1105),#862,.F.);
#9328=ADVANCED_FACE('',(#1106),#9147,.T.);
#9329=ADVANCED_FACE('',(#1107),#769,.T.);
#9330=ADVANCED_FACE('',(#1108),#9148,.T.);
#9331=ADVANCED_FACE('',(#1109),#863,.T.);
#9332=ADVANCED_FACE('',(#1110),#864,.F.);
#9333=ADVANCED_FACE('',(#1111),#9149,.T.);
#9334=ADVANCED_FACE('',(#1112),#770,.T.);
#9335=ADVANCED_FACE('',(#1113),#9150,.T.);
#9336=ADVANCED_FACE('',(#1114),#865,.T.);
#9337=ADVANCED_FACE('',(#1115),#771,.F.);
#9338=ADVANCED_FACE('',(#1116,#710),#866,.T.);
#9339=ADVANCED_FACE('',(#1117),#9151,.T.);
#9340=ADVANCED_FACE('',(#1118),#772,.T.);
#9341=ADVANCED_FACE('',(#1119),#9152,.F.);
#9342=ADVANCED_FACE('',(#1120,#711),#867,.F.);
#9343=ADVANCED_FACE('',(#1121),#868,.T.);
#9344=ADVANCED_FACE('',(#1122),#605,.T.);
#9345=ADVANCED_FACE('',(#1123),#869,.T.);
#9346=ADVANCED_FACE('',(#1124),#870,.T.);
#9347=ADVANCED_FACE('',(#1125),#871,.T.);
#9348=ADVANCED_FACE('',(#1126),#872,.T.);
#9349=ADVANCED_FACE('',(#1127),#873,.T.);
#9350=ADVANCED_FACE('',(#1128),#874,.T.);
#9351=ADVANCED_FACE('',(#1129),#875,.T.);
#9352=ADVANCED_FACE('',(#1130),#876,.T.);
#9353=ADVANCED_FACE('',(#1131),#877,.T.);
#9354=ADVANCED_FACE('',(#1132),#606,.T.);
#9355=ADVANCED_FACE('',(#1133),#878,.T.);
#9356=ADVANCED_FACE('',(#1134),#607,.T.);
#9357=ADVANCED_FACE('',(#1135),#879,.T.);
#9358=ADVANCED_FACE('',(#1136),#880,.T.);
#9359=ADVANCED_FACE('',(#1137),#881,.T.);
#9360=ADVANCED_FACE('',(#1138),#882,.F.);
#9361=ADVANCED_FACE('',(#1139),#608,.T.);
#9362=ADVANCED_FACE('',(#1140),#883,.T.);
#9363=ADVANCED_FACE('',(#1141),#609,.T.);
#9364=ADVANCED_FACE('',(#1142),#884,.F.);
#9365=ADVANCED_FACE('',(#1143),#885,.T.);
#9366=ADVANCED_FACE('',(#1144),#886,.T.);
#9367=ADVANCED_FACE('',(#1145),#887,.T.);
#9368=ADVANCED_FACE('',(#1146),#610,.T.);
#9369=ADVANCED_FACE('',(#1147),#888,.F.);
#9370=ADVANCED_FACE('',(#1148),#889,.T.);
#9371=ADVANCED_FACE('',(#1149),#890,.T.);
#9372=ADVANCED_FACE('',(#1150),#891,.T.);
#9373=ADVANCED_FACE('',(#1151),#611,.T.);
#9374=ADVANCED_FACE('',(#1152),#892,.F.);
#9375=ADVANCED_FACE('',(#1153),#893,.T.);
#9376=ADVANCED_FACE('',(#1154),#894,.T.);
#9377=ADVANCED_FACE('',(#1155),#895,.T.);
#9378=ADVANCED_FACE('',(#1156),#896,.T.);
#9379=ADVANCED_FACE('',(#1157),#897,.T.);
#9380=ADVANCED_FACE('',(#1158),#898,.T.);
#9381=ADVANCED_FACE('',(#1159),#899,.T.);
#9382=ADVANCED_FACE('',(#1160),#900,.T.);
#9383=ADVANCED_FACE('',(#1161),#901,.T.);
#9384=ADVANCED_FACE('',(#1162),#902,.T.);
#9385=ADVANCED_FACE('',(#1163),#903,.T.);
#9386=ADVANCED_FACE('',(#1164),#904,.T.);
#9387=ADVANCED_FACE('',(#1165),#905,.T.);
#9388=ADVANCED_FACE('',(#1166),#906,.T.);
#9389=ADVANCED_FACE('',(#1167),#9153,.T.);
#9390=ADVANCED_FACE('',(#1168),#907,.T.);
#9391=ADVANCED_FACE('',(#1169),#9154,.T.);
#9392=ADVANCED_FACE('',(#1170),#908,.T.);
#9393=ADVANCED_FACE('',(#1171),#612,.T.);
#9394=ADVANCED_FACE('',(#1172),#9155,.T.);
#9395=ADVANCED_FACE('',(#1173),#909,.T.);
#9396=ADVANCED_FACE('',(#1174),#9156,.T.);
#9397=ADVANCED_FACE('',(#1175),#910,.T.);
#9398=ADVANCED_FACE('',(#1176),#9157,.T.);
#9399=ADVANCED_FACE('',(#1177),#911,.T.);
#9400=ADVANCED_FACE('',(#1178),#9158,.F.);
#9401=ADVANCED_FACE('',(#1179,#712),#9159,.F.);
#9402=ADVANCED_FACE('',(#1180),#613,.F.);
#9403=ADVANCED_FACE('',(#1181,#713),#912,.F.);
#9404=ADVANCED_FACE('',(#1182),#9160,.F.);
#9405=ADVANCED_FACE('',(#1183),#614,.T.);
#9406=ADVANCED_FACE('',(#1184),#9161,.T.);
#9407=ADVANCED_FACE('',(#1185,#714),#913,.T.);
#9408=ADVANCED_FACE('',(#1186),#615,.T.);
#9409=ADVANCED_FACE('',(#1187),#616,.F.);
#9410=ADVANCED_FACE('',(#1188),#9162,.F.);
#9411=ADVANCED_FACE('',(#1189),#914,.F.);
#9412=ADVANCED_FACE('',(#1190),#94,.F.);
#9413=ADVANCED_FACE('',(#1191),#95,.F.);
#9414=ADVANCED_FACE('',(#1192),#617,.F.);
#9415=ADVANCED_FACE('',(#1193,#715),#915,.T.);
#9416=ADVANCED_FACE('',(#1194,#716),#916,.T.);
#9417=ADVANCED_FACE('',(#1195,#717),#917,.T.);
#9418=ADVANCED_FACE('',(#1196,#718),#918,.T.);
#9419=ADVANCED_FACE('',(#1197,#719),#919,.T.);
#9420=ADVANCED_FACE('',(#1198,#720),#920,.T.);
#9421=ADVANCED_FACE('',(#1199,#721),#921,.T.);
#9422=ADVANCED_FACE('',(#1200,#722),#922,.T.);
#9423=ADVANCED_FACE('',(#1201,#723),#923,.T.);
#9424=ADVANCED_FACE('',(#1202,#724),#924,.T.);
#9425=ADVANCED_FACE('',(#1203,#725),#925,.T.);
#9426=ADVANCED_FACE('',(#1204,#726),#926,.F.);
#9427=ADVANCED_FACE('',(#1205,#727),#927,.T.);
#9428=ADVANCED_FACE('',(#1206,#728),#928,.T.);
#9429=ADVANCED_FACE('',(#1207,#729),#929,.F.);
#9430=ADVANCED_FACE('',(#1208),#9163,.T.);
#9431=ADVANCED_FACE('',(#1209),#9164,.T.);
#9432=ADVANCED_FACE('',(#1210),#9165,.T.);
#9433=ADVANCED_FACE('',(#1211),#9166,.T.);
#9434=ADVANCED_FACE('',(#1212),#9167,.T.);
#9435=ADVANCED_FACE('',(#1213),#9168,.T.);
#9436=ADVANCED_FACE('',(#1214),#9169,.T.);
#9437=ADVANCED_FACE('',(#1215),#9170,.T.);
#9438=ADVANCED_FACE('',(#1216),#618,.T.);
#9439=ADVANCED_FACE('',(#1217),#619,.T.);
#9440=ADVANCED_FACE('',(#1218),#620,.T.);
#9441=ADVANCED_FACE('',(#1219),#621,.T.);
#9442=ADVANCED_FACE('',(#1220),#622,.T.);
#9443=ADVANCED_FACE('',(#1221),#623,.T.);
#9444=ADVANCED_FACE('',(#1222),#624,.T.);
#9445=ADVANCED_FACE('',(#1223,#730),#930,.T.);
#9446=ADVANCED_FACE('',(#1224),#625,.T.);
#9447=ADVANCED_FACE('',(#1225),#626,.T.);
#9448=ADVANCED_FACE('',(#1226),#627,.T.);
#9449=ADVANCED_FACE('',(#1227),#628,.T.);
#9450=ADVANCED_FACE('',(#1228),#629,.T.);
#9451=ADVANCED_FACE('',(#1229,#731),#931,.F.);
#9452=ADVANCED_FACE('',(#1230),#9171,.T.);
#9453=ADVANCED_FACE('',(#1231,#732),#932,.T.);
#9454=ADVANCED_FACE('',(#1232,#733),#933,.F.);
#9455=ADVANCED_FACE('',(#1233),#9172,.T.);
#9456=ADVANCED_FACE('',(#1234,#734),#934,.T.);
#9457=ADVANCED_FACE('',(#1235,#735),#935,.F.);
#9458=ADVANCED_FACE('',(#1236),#9173,.T.);
#9459=ADVANCED_FACE('',(#1237,#736),#936,.T.);
#9460=ADVANCED_FACE('',(#1238,#737),#937,.F.);
#9461=ADVANCED_FACE('',(#1239),#9174,.T.);
#9462=ADVANCED_FACE('',(#1240,#738),#938,.T.);
#9463=ADVANCED_FACE('',(#1241,#739),#939,.F.);
#9464=ADVANCED_FACE('',(#1242),#9175,.T.);
#9465=ADVANCED_FACE('',(#1243,#740),#940,.T.);
#9466=ADVANCED_FACE('',(#1244),#9176,.T.);
#9467=ADVANCED_FACE('',(#1245),#941,.T.);
#9468=ADVANCED_FACE('',(#1246),#942,.T.);
#9469=ADVANCED_FACE('',(#1247),#943,.T.);
#9470=ADVANCED_FACE('',(#1248),#944,.T.);
#9471=ADVANCED_FACE('',(#1249),#9177,.T.);
#9472=ADVANCED_FACE('',(#1250),#945,.T.);
#9473=ADVANCED_FACE('',(#1251),#946,.T.);
#9474=ADVANCED_FACE('',(#1252),#947,.T.);
#9475=ADVANCED_FACE('',(#1253),#948,.T.);
#9476=ADVANCED_FACE('',(#1254),#949,.T.);
#9477=ADVANCED_FACE('',(#1255),#9178,.F.);
#9478=ADVANCED_FACE('',(#1256),#9179,.T.);
#9479=ADVANCED_FACE('',(#1257),#950,.T.);
#9480=ADVANCED_FACE('',(#1258),#951,.T.);
#9481=ADVANCED_FACE('',(#1259),#952,.T.);
#9482=ADVANCED_FACE('',(#1260),#953,.F.);
#9483=ADVANCED_FACE('',(#1261),#954,.F.);
#9484=ADVANCED_FACE('',(#1262),#9180,.T.);
#9485=ADVANCED_FACE('',(#1263),#773,.T.);
#9486=ADVANCED_FACE('',(#1264),#9181,.T.);
#9487=ADVANCED_FACE('',(#1265),#955,.T.);
#9488=ADVANCED_FACE('',(#1266),#9182,.T.);
#9489=ADVANCED_FACE('',(#1267),#774,.T.);
#9490=ADVANCED_FACE('',(#1268),#9183,.T.);
#9491=ADVANCED_FACE('',(#1269),#956,.T.);
#9492=ADVANCED_FACE('',(#1270),#957,.F.);
#9493=ADVANCED_FACE('',(#1271),#9184,.T.);
#9494=ADVANCED_FACE('',(#1272),#775,.T.);
#9495=ADVANCED_FACE('',(#1273),#9185,.T.);
#9496=ADVANCED_FACE('',(#1274),#958,.T.);
#9497=ADVANCED_FACE('',(#1275),#959,.F.);
#9498=ADVANCED_FACE('',(#1276),#9186,.F.);
#9499=ADVANCED_FACE('',(#1277),#9187,.F.);
#9500=ADVANCED_FACE('',(#1278),#9188,.F.);
#9501=ADVANCED_FACE('',(#1279),#9189,.F.);
#9502=ADVANCED_FACE('',(#1280),#9190,.F.);
#9503=ADVANCED_FACE('',(#1281),#9191,.F.);
#9504=ADVANCED_FACE('',(#1282),#9192,.F.);
#9505=ADVANCED_FACE('',(#1283),#9193,.F.);
#9506=ADVANCED_FACE('',(#1284),#9194,.F.);
#9507=ADVANCED_FACE('',(#1285),#9195,.F.);
#9508=ADVANCED_FACE('',(#1286),#9196,.F.);
#9509=ADVANCED_FACE('',(#1287),#9197,.F.);
#9510=ADVANCED_FACE('',(#1288),#9198,.F.);
#9511=ADVANCED_FACE('',(#1289),#9199,.F.);
#9512=ADVANCED_FACE('',(#1290),#9200,.F.);
#9513=ADVANCED_FACE('',(#1291),#9201,.F.);
#9514=ADVANCED_FACE('',(#1292),#9202,.F.);
#9515=ADVANCED_FACE('',(#1293),#9203,.F.);
#9516=ADVANCED_FACE('',(#1294),#9204,.F.);
#9517=ADVANCED_FACE('',(#1295),#9205,.F.);
#9518=ADVANCED_FACE('',(#1296),#9206,.F.);
#9519=ADVANCED_FACE('',(#1297),#9207,.F.);
#9520=ADVANCED_FACE('',(#1298),#9208,.F.);
#9521=ADVANCED_FACE('',(#1299),#9209,.F.);
#9522=ADVANCED_FACE('',(#1300),#9210,.F.);
#9523=ADVANCED_FACE('',(#1301),#9211,.F.);
#9524=ADVANCED_FACE('',(#1302),#9212,.F.);
#9525=ADVANCED_FACE('',(#1303),#9213,.F.);
#9526=ADVANCED_FACE('',(#1304),#9214,.F.);
#9527=ADVANCED_FACE('',(#1305),#9215,.F.);
#9528=ADVANCED_FACE('',(#1306),#9216,.F.);
#9529=ADVANCED_FACE('',(#1307),#9217,.F.);
#9530=ADVANCED_FACE('',(#1308),#9218,.F.);
#9531=ADVANCED_FACE('',(#1309),#9219,.F.);
#9532=ADVANCED_FACE('',(#1310),#9220,.F.);
#9533=ADVANCED_FACE('',(#1311),#9221,.F.);
#9534=ADVANCED_FACE('',(#1312),#9222,.F.);
#9535=ADVANCED_FACE('',(#1313),#9223,.F.);
#9536=ADVANCED_FACE('',(#1314),#9224,.F.);
#9537=ADVANCED_FACE('',(#1315),#9225,.F.);
#9538=ADVANCED_FACE('',(#1316),#9226,.F.);
#9539=ADVANCED_FACE('',(#1317),#9227,.F.);
#9540=ADVANCED_FACE('',(#1318),#960,.T.);
#9541=ADVANCED_FACE('',(#1319),#961,.T.);
#9542=ADVANCED_FACE('',(#1320),#962,.T.);
#9543=ADVANCED_FACE('',(#1321,#741),#963,.F.);
#9544=ADVANCED_FACE('',(#1322),#964,.T.);
#9545=ADVANCED_FACE('',(#1323,#742,#743),#965,.F.);
#9546=ADVANCED_FACE('',(#1324),#966,.T.);
#9547=ADVANCED_FACE('',(#1325),#967,.T.);
#9548=ADVANCED_FACE('',(#1326),#968,.T.);
#9549=ADVANCED_FACE('',(#1327),#9228,.F.);
#9550=ADVANCED_FACE('',(#1328),#9229,.F.);
#9551=ADVANCED_FACE('',(#1329),#630,.F.);
#9552=ADVANCED_FACE('',(#1330),#969,.T.);
#9553=ADVANCED_FACE('',(#1331),#631,.F.);
#9554=ADVANCED_FACE('',(#1332),#632,.F.);
#9555=ADVANCED_FACE('',(#1333),#633,.F.);
#9556=ADVANCED_FACE('',(#1334),#634,.F.);
#9557=ADVANCED_FACE('',(#1335),#970,.T.);
#9558=ADVANCED_FACE('',(#1336),#971,.T.);
#9559=ADVANCED_FACE('',(#1337),#972,.T.);
#9560=ADVANCED_FACE('',(#1338),#973,.T.);
#9561=ADVANCED_FACE('',(#1339),#974,.T.);
#9562=ADVANCED_FACE('',(#1340),#975,.T.);
#9563=ADVANCED_FACE('',(#1341,#744),#976,.F.);
#9564=ADVANCED_FACE('',(#1342),#635,.F.);
#9565=ADVANCED_FACE('',(#1343),#977,.T.);
#9566=ADVANCED_FACE('',(#1344),#978,.T.);
#9567=ADVANCED_FACE('',(#1345),#979,.T.);
#9568=ADVANCED_FACE('',(#1346),#636,.F.);
#9569=ADVANCED_FACE('',(#1347),#9230,.F.);
#9570=ADVANCED_FACE('',(#1348),#980,.T.);
#9571=ADVANCED_FACE('',(#1349),#981,.T.);
#9572=ADVANCED_FACE('',(#1350),#982,.T.);
#9573=ADVANCED_FACE('',(#1351),#983,.T.);
#9574=ADVANCED_FACE('',(#1352),#984,.T.);
#9575=ADVANCED_FACE('',(#1353),#985,.T.);
#9576=ADVANCED_FACE('',(#1354,#745,#746),#986,.T.);
#9577=ADVANCED_FACE('',(#1355),#987,.T.);
#9578=ADVANCED_FACE('',(#1356),#988,.T.);
#9579=ADVANCED_FACE('',(#1357),#9231,.F.);
#9580=ADVANCED_FACE('',(#1358),#96,.F.);
#9581=ADVANCED_FACE('',(#1359),#97,.F.);
#9582=ADVANCED_FACE('',(#1360,#747),#9232,.F.);
#9583=ADVANCED_FACE('',(#1361),#989,.T.);
#9584=ADVANCED_FACE('',(#1362),#990,.T.);
#9585=ADVANCED_FACE('',(#1363),#98,.F.);
#9586=ADVANCED_FACE('',(#1364),#99,.F.);
#9587=ADVANCED_FACE('',(#1365),#637,.F.);
#9588=ADVANCED_FACE('',(#1366),#9233,.F.);
#9589=ADVANCED_FACE('',(#1367),#100,.F.);
#9590=ADVANCED_FACE('',(#1368),#101,.F.);
#9591=ADVANCED_FACE('',(#1369),#9234,.F.);
#9592=ADVANCED_FACE('',(#1370),#991,.T.);
#9593=ADVANCED_FACE('',(#1371),#638,.F.);
#9594=ADVANCED_FACE('',(#1372),#992,.T.);
#9595=ADVANCED_FACE('',(#1373),#993,.F.);
#9596=ADVANCED_FACE('',(#1374),#9235,.F.);
#9597=ADVANCED_FACE('',(#1375),#994,.F.);
#9598=ADVANCED_FACE('',(#1376),#102,.F.);
#9599=ADVANCED_FACE('',(#1377),#9236,.F.);
#9600=ADVANCED_FACE('',(#1378),#103,.F.);
#9601=ADVANCED_FACE('',(#1379),#9237,.F.);
#9602=ADVANCED_FACE('',(#1380),#9238,.F.);
#9603=ADVANCED_FACE('',(#1381),#104,.F.);
#9604=ADVANCED_FACE('',(#1382),#9239,.F.);
#9605=ADVANCED_FACE('',(#1383),#105,.F.);
#9606=ADVANCED_FACE('',(#1384),#995,.F.);
#9607=ADVANCED_FACE('',(#1385),#996,.F.);
#9608=ADVANCED_FACE('',(#1386),#9240,.T.);
#9609=ADVANCED_FACE('',(#1387),#776,.T.);
#9610=ADVANCED_FACE('',(#1388),#9241,.T.);
#9611=ADVANCED_FACE('',(#1389),#997,.T.);
#9612=ADVANCED_FACE('',(#1390),#998,.F.);
#9613=ADVANCED_FACE('',(#1391),#9242,.T.);
#9614=ADVANCED_FACE('',(#1392),#9243,.T.);
#9615=ADVANCED_FACE('',(#1393),#9244,.T.);
#9616=ADVANCED_FACE('',(#1394),#9245,.T.);
#9617=ADVANCED_FACE('',(#1395),#639,.F.);
#9618=ADVANCED_FACE('',(#1396),#9246,.F.);
#9619=ADVANCED_FACE('',(#1397,#748),#999,.F.);
#9620=ADVANCED_FACE('',(#1398),#640,.F.);
#9621=ADVANCED_FACE('',(#1399,#749),#1000,.T.);
#9622=ADVANCED_FACE('',(#1400),#9247,.F.);
#9623=ADVANCED_FACE('',(#1401),#641,.F.);
#9624=ADVANCED_FACE('',(#1402),#642,.T.);
#9625=ADVANCED_FACE('',(#1403),#9248,.T.);
#9626=ADVANCED_FACE('',(#1404),#1001,.F.);
#9627=ADVANCED_FACE('',(#1405),#106,.F.);
#9628=ADVANCED_FACE('',(#1406),#107,.F.);
#9629=ADVANCED_FACE('',(#1407),#643,.T.);
#9630=ADVANCED_FACE('',(#1408,#750),#1002,.T.);
#9631=ADVANCED_FACE('',(#1409),#108,.F.);
#9632=ADVANCED_FACE('',(#1410),#1003,.T.);
#9633=ADVANCED_FACE('',(#1411),#109,.F.);
#9634=ADVANCED_FACE('',(#1412,#751),#1004,.T.);
#9635=ADVANCED_FACE('',(#1413),#644,.T.);
#9636=ADVANCED_FACE('',(#1414,#752),#1005,.F.);
#9637=ADVANCED_FACE('',(#1415),#9249,.T.);
#9638=ADVANCED_FACE('',(#1416),#645,.T.);
#9639=ADVANCED_FACE('',(#1417),#9250,.T.);
#9640=ADVANCED_FACE('',(#1418),#1006,.F.);
#9641=ADVANCED_FACE('',(#1419),#646,.T.);
#9642=ADVANCED_FACE('',(#1420),#1007,.T.);
#9643=ADVANCED_FACE('',(#1421),#9251,.T.);
#9644=ADVANCED_FACE('',(#1422),#9252,.T.);
#9645=ADVANCED_FACE('',(#1423),#9253,.T.);
#9646=ADVANCED_FACE('',(#1424),#9254,.T.);
#9647=ADVANCED_FACE('',(#1425),#9255,.T.);
#9648=ADVANCED_FACE('',(#1426),#9256,.T.);
#9649=ADVANCED_FACE('',(#1427),#110,.T.);
#9650=ADVANCED_FACE('',(#1428),#9257,.T.);
#9651=ADVANCED_FACE('',(#1429),#9258,.T.);
#9652=ADVANCED_FACE('',(#1430),#111,.T.);
#9653=ADVANCED_FACE('',(#1431,#753),#1008,.T.);
#9654=ADVANCED_FACE('',(#1432),#647,.T.);
#9655=ADVANCED_FACE('',(#1433),#1009,.T.);
#9656=ADVANCED_FACE('',(#1434,#754),#1010,.T.);
#9657=ADVANCED_FACE('',(#1435),#1011,.T.);
#9658=ADVANCED_FACE('',(#1436,#755),#1012,.T.);
#9659=ADVANCED_FACE('',(#1437),#1013,.T.);
#9660=ADVANCED_FACE('',(#1438),#1014,.T.);
#9661=ADVANCED_FACE('',(#1439),#1015,.T.);
#9662=ADVANCED_FACE('',(#1440),#1016,.T.);
#9663=ADVANCED_FACE('',(#1441),#1017,.T.);
#9664=ADVANCED_FACE('',(#1442),#1018,.T.);
#9665=ADVANCED_FACE('',(#1443,#756),#1019,.F.);
#9666=ADVANCED_FACE('',(#1444),#1020,.T.);
#9667=ADVANCED_FACE('',(#1445),#1021,.T.);
#9668=ADVANCED_FACE('',(#1446),#1022,.T.);
#9669=ADVANCED_FACE('',(#1447),#1023,.T.);
#9670=ADVANCED_FACE('',(#1448,#757),#1024,.T.);
#9671=ADVANCED_FACE('',(#1449),#1025,.T.);
#9672=ADVANCED_FACE('',(#1450),#1026,.T.);
#9673=ADVANCED_FACE('',(#1451),#1027,.T.);
#9674=ADVANCED_FACE('',(#1452),#1028,.T.);
#9675=ADVANCED_FACE('',(#1453),#1029,.T.);
#9676=ADVANCED_FACE('',(#1454),#1030,.T.);
#9677=ADVANCED_FACE('',(#1455),#1031,.T.);
#9678=ADVANCED_FACE('',(#1456),#1032,.T.);
#9679=ADVANCED_FACE('',(#1457),#1033,.T.);
#9680=ADVANCED_FACE('',(#1458),#112,.T.);
#9681=ADVANCED_FACE('',(#1459),#648,.F.);
#9682=ADVANCED_FACE('',(#1460),#649,.F.);
#9683=ADVANCED_FACE('',(#1461),#650,.F.);
#9684=ADVANCED_FACE('',(#1462),#651,.F.);
#9685=ADVANCED_FACE('',(#1463),#9259,.F.);
#9686=ADVANCED_FACE('',(#1464),#652,.F.);
#9687=ADVANCED_FACE('',(#1465,#758),#1034,.F.);
#9688=ADVANCED_FACE('',(#1466),#9260,.F.);
#9689=ADVANCED_FACE('',(#1467),#653,.T.);
#9690=ADVANCED_FACE('',(#1468),#1035,.F.);
#9691=ADVANCED_FACE('',(#1469),#113,.F.);
#9692=ADVANCED_FACE('',(#1470),#1036,.T.);
#9693=ADVANCED_FACE('',(#1471),#114,.F.);
#9694=ADVANCED_FACE('',(#1472,#759),#1037,.T.);
#9695=ADVANCED_FACE('',(#1473),#115,.T.);
#9696=ADVANCED_FACE('',(#1474),#116,.T.);
#9697=ADVANCED_FACE('',(#1475),#117,.T.);
#9698=ADVANCED_FACE('',(#1476),#118,.T.);
#9699=ADVANCED_FACE('',(#1477),#119,.T.);
#9700=ADVANCED_FACE('',(#1478),#120,.T.);
#9701=ADVANCED_FACE('',(#1479),#121,.T.);
#9702=ADVANCED_FACE('',(#1480),#122,.T.);
#9703=ADVANCED_FACE('',(#1481),#123,.T.);
#9704=ADVANCED_FACE('',(#1482),#124,.T.);
#9705=ADVANCED_FACE('',(#1483),#125,.T.);
#9706=ADVANCED_FACE('',(#1484),#126,.T.);
#9707=ADVANCED_FACE('',(#1485),#127,.T.);
#9708=ADVANCED_FACE('',(#1486),#128,.T.);
#9709=ADVANCED_FACE('',(#1487),#129,.T.);
#9710=ADVANCED_FACE('',(#1488),#130,.T.);
#9711=ADVANCED_FACE('',(#1489),#131,.T.);
#9712=ADVANCED_FACE('',(#1490),#132,.T.);
#9713=ADVANCED_FACE('',(#1491),#133,.T.);
#9714=ADVANCED_FACE('',(#1492),#134,.T.);
#9715=ADVANCED_FACE('',(#1493),#135,.T.);
#9716=ADVANCED_FACE('',(#1494),#9261,.T.);
#9717=ADVANCED_FACE('',(#1495),#136,.T.);
#9718=ADVANCED_FACE('',(#1496),#9262,.T.);
#9719=ADVANCED_FACE('',(#1497),#9263,.T.);
#9720=ADVANCED_FACE('',(#1498),#137,.T.);
#9721=ADVANCED_FACE('',(#1499),#9264,.T.);
#9722=ADVANCED_FACE('',(#1500),#138,.T.);
#9723=ADVANCED_FACE('',(#1501),#9265,.T.);
#9724=ADVANCED_FACE('',(#1502),#9266,.T.);
#9725=ADVANCED_FACE('',(#1503),#9267,.T.);
#9726=ADVANCED_FACE('',(#1504),#9268,.T.);
#9727=ADVANCED_FACE('',(#1505),#1038,.T.);
#9728=ADVANCED_FACE('',(#1506),#1039,.T.);
#9729=ADVANCED_FACE('',(#1507),#1040,.T.);
#9730=ADVANCED_FACE('',(#1508),#1041,.T.);
#9731=ADVANCED_FACE('',(#1509,#760,#761),#1042,.F.);
#9732=ADVANCED_FACE('',(#1510),#9269,.T.);
#9733=ADVANCED_FACE('',(#1511),#1043,.T.);
#9734=ADVANCED_FACE('',(#1512),#1044,.T.);
#9735=ADVANCED_FACE('',(#1513),#9270,.T.);
#9736=ADVANCED_FACE('',(#1514),#1045,.T.);
#9737=ADVANCED_FACE('',(#1515),#1046,.T.);
#9738=ADVANCED_FACE('',(#1516),#9271,.T.);
#9739=ADVANCED_FACE('',(#1517),#1047,.T.);
#9740=ADVANCED_FACE('',(#1518),#1048,.T.);
#9741=ADVANCED_FACE('',(#1519),#9272,.T.);
#9742=ADVANCED_FACE('',(#1520),#1049,.T.);
#9743=ADVANCED_FACE('',(#1521),#1050,.T.);
#9744=ADVANCED_FACE('',(#1522),#9273,.T.);
#9745=ADVANCED_FACE('',(#1523),#1051,.T.);
#9746=ADVANCED_FACE('',(#1524),#1052,.T.);
#9747=ADVANCED_FACE('',(#1525),#1053,.F.);
#9748=ADVANCED_FACE('',(#1526),#1054,.T.);
#9749=ADVANCED_FACE('',(#1527),#1055,.T.);
#9750=ADVANCED_FACE('',(#1528),#1056,.T.);
#9751=ADVANCED_FACE('',(#1529),#1057,.T.);
#9752=ADVANCED_FACE('',(#1530),#1058,.T.);
#9753=ADVANCED_FACE('',(#1531),#1059,.T.);
#9754=ADVANCED_FACE('',(#1532),#1060,.F.);
#9755=ADVANCED_FACE('',(#1533),#1061,.T.);
#9756=ADVANCED_FACE('',(#1534),#1062,.T.);
#9757=ADVANCED_FACE('',(#1535),#1063,.F.);
#9758=ADVANCED_FACE('',(#1536),#1064,.F.);
#9759=ADVANCED_FACE('',(#1537),#1065,.T.);
#9760=ADVANCED_FACE('',(#1538),#1066,.T.);
#9761=ADVANCED_FACE('',(#1539),#1067,.T.);
#9762=ADVANCED_FACE('',(#1540),#1068,.F.);
#9763=ADVANCED_FACE('',(#1541),#777,.F.);
#9764=ADVANCED_FACE('',(#1542),#9274,.F.);
#9765=ADVANCED_FACE('',(#1543,#762),#1069,.T.);
#9766=ADVANCED_FACE('',(#1544,#763),#1070,.T.);
#9767=ADVANCED_FACE('',(#1545),#9275,.F.);
#9768=ADVANCED_FACE('',(#1546),#1071,.F.);
#9769=ADVANCED_FACE('',(#1547),#1072,.T.);
#9770=ADVANCED_FACE('',(#1548),#1073,.T.);
#9771=ADVANCED_FACE('',(#1549),#1074,.T.);
#9772=ADVANCED_FACE('',(#1550),#9276,.F.);
#9773=ADVANCED_FACE('',(#1551),#1075,.T.);
#9774=ADVANCED_FACE('',(#1552),#1076,.T.);
#9775=ADVANCED_FACE('',(#1553),#9277,.F.);
#9776=ADVANCED_FACE('',(#1554),#1077,.F.);
#9777=ADVANCED_FACE('',(#1555),#9278,.F.);
#9778=ADVANCED_FACE('',(#1556),#1078,.T.);
#9779=ADVANCED_FACE('',(#1557),#1079,.T.);
#9780=ADVANCED_FACE('',(#1558),#9279,.F.);
#9781=ADVANCED_FACE('',(#1559),#1080,.T.);
#9782=ADVANCED_FACE('',(#1560),#1081,.T.);
#9783=ADVANCED_FACE('',(#1561),#1082,.F.);
#9784=ADVANCED_FACE('',(#1562),#654,.T.);
#9785=ADVANCED_FACE('',(#1563),#9280,.T.);
#9786=ADVANCED_FACE('',(#1564),#1083,.F.);
#9787=ADVANCED_FACE('',(#1565),#1084,.T.);
#9788=ADVANCED_FACE('',(#1566),#9281,.T.);
#9789=ADVANCED_FACE('',(#1567),#9282,.T.);
#9790=ADVANCED_FACE('',(#1568),#9283,.T.);
#9791=ADVANCED_FACE('',(#1569),#9284,.T.);
#9792=ADVANCED_FACE('',(#1570),#9285,.T.);
#9793=ADVANCED_FACE('',(#1571),#9286,.T.);
#9794=ADVANCED_FACE('',(#1572),#9287,.T.);
#9795=ADVANCED_FACE('',(#1573),#9288,.T.);
#9796=ADVANCED_FACE('',(#1574),#9289,.T.);
#9797=ADVANCED_FACE('',(#1575),#9290,.T.);
#9798=ADVANCED_FACE('',(#1576),#9291,.T.);
#9799=ADVANCED_FACE('',(#1577),#9292,.T.);
#9800=ADVANCED_FACE('',(#1578),#9293,.T.);
#9801=ADVANCED_FACE('',(#1579),#9294,.T.);
#9802=ADVANCED_FACE('',(#1580),#9295,.T.);
#9803=ADVANCED_FACE('',(#1581),#9296,.T.);
#9804=ADVANCED_FACE('',(#1582),#9297,.T.);
#9805=ADVANCED_FACE('',(#1583),#9298,.T.);
#9806=ADVANCED_FACE('',(#1584),#9299,.T.);
#9807=ADVANCED_FACE('',(#1585),#9300,.T.);
#9808=ADVANCED_FACE('',(#1586),#9301,.T.);
#9809=ADVANCED_FACE('',(#1587),#9302,.T.);
#9810=ADVANCED_FACE('',(#1588),#9303,.T.);
#9811=ADVANCED_FACE('',(#1589),#9304,.T.);
#9812=ADVANCED_FACE('',(#1590),#9305,.T.);
#9813=ADVANCED_FACE('',(#1591),#9306,.T.);
#9814=ADVANCED_FACE('',(#1592),#9307,.T.);
#9815=ADVANCED_FACE('',(#1593),#9308,.T.);
#9816=ADVANCED_FACE('',(#1594),#9309,.T.);
#9817=ADVANCED_FACE('',(#1595),#9310,.T.);
#9818=ADVANCED_FACE('',(#1596),#9311,.T.);
#9819=ADVANCED_FACE('',(#1597),#9312,.T.);
#9820=ADVANCED_FACE('',(#1598),#9313,.T.);
#9821=ADVANCED_FACE('',(#1599),#655,.F.);
#9822=ADVANCED_FACE('',(#1600),#9314,.T.);
#9823=ADVANCED_FACE('',(#1601,#764),#93,.T.);
#9824=ADVANCED_FACE('',(#1602),#656,.T.);
#9825=ADVANCED_FACE('',(#1603),#1085,.T.);
#9826=ADVANCED_FACE('',(#1604),#91,.T.);
#9827=ADVANCED_FACE('',(#1605),#92,.T.);
#9828=ADVANCED_FACE('',(#1606,#765),#1086,.F.);
#9829=ADVANCED_FACE('',(#1607,#766),#1087,.F.);
#9830=ADVANCED_FACE('',(#1608),#657,.F.);
#9831=ADVANCED_FACE('',(#1609),#658,.F.);
#9832=ADVANCED_FACE('',(#1610),#659,.F.);
#9833=ADVANCED_FACE('',(#1611),#660,.F.);
#9834=ADVANCED_FACE('',(#1612),#661,.F.);
#9835=ADVANCED_FACE('',(#1613),#1088,.T.);
#9836=ADVANCED_FACE('',(#1614),#1089,.F.);
#9837=ADVANCED_FACE('',(#1615),#1090,.F.);
#9838=ADVANCED_FACE('',(#1616),#1091,.F.);
#9839=ADVANCED_FACE('',(#1617),#1092,.F.);
#9840=ADVANCED_FACE('',(#1618),#1093,.F.);
#9841=ADVANCED_FACE('',(#1619),#1094,.F.);
#9842=ADVANCED_FACE('',(#1620),#1095,.F.);
#9843=ADVANCED_FACE('',(#1621),#9315,.T.);
#9844=ADVANCED_FACE('',(#1622),#778,.T.);
#9845=ADVANCED_FACE('',(#1623),#9316,.T.);
#9846=ADVANCED_FACE('',(#1624),#1096,.T.);
#9847=ADVANCED_FACE('',(#1625),#9317,.T.);
#9848=ADVANCED_FACE('',(#1626),#779,.T.);
#9849=ADVANCED_FACE('',(#1627),#9318,.T.);
#9850=ADVANCED_FACE('',(#1628),#1097,.T.);
#9851=ADVANCED_FACE('',(#1629),#1098,.F.);
#9852=ADVANCED_FACE('',(#1630),#9319,.T.);
#9853=ADVANCED_FACE('',(#1631),#9320,.T.);
#9854=ADVANCED_FACE('',(#1632),#9321,.T.);
#9855=ADVANCED_FACE('',(#1633),#9322,.T.);
#9856=ADVANCED_FACE('',(#1634),#662,.F.);
#9857=ADVANCED_FACE('',(#1635),#9323,.F.);
#9858=ADVANCED_FACE('',(#1636,#767),#1099,.F.);
#9859=ADVANCED_FACE('',(#1637),#663,.F.);
#9860=ADVANCED_FACE('',(#1638,#768),#1100,.T.);
#9861=ADVANCED_FACE('',(#1639),#1101,.F.);
#9862=ADVANCED_FACE('',(#1640),#139,.F.);
#9863=ADVANCED_FACE('',(#1641),#140,.F.);
#9864=ADVANCED_FACE('',(#1642),#664,.T.);
#9865=CLOSED_SHELL('',(#9324,#9325,#9326));
#9866=CLOSED_SHELL('',(#9327,#9328,#9329,#9330,#9331));
#9867=CLOSED_SHELL('',(#9332,#9333,#9334,#9335,#9336));
#9868=CLOSED_SHELL('',(#9337,#9338,#9339,#9340,#9341,#9342,#9343,#9344,
#9345,#9346,#9347,#9348,#9349,#9350,#9351,#9352,#9353,#9354,#9355,#9356,
#9357,#9358,#9359,#9360,#9361,#9362,#9363,#9364,#9365,#9366,#9367,#9368,
#9369,#9370,#9371,#9372,#9373,#9374,#9375,#9376,#9377,#9378,#9379,#9380,
#9381,#9382,#9383,#9384,#9385,#9386,#9387,#9388,#9389,#9390,#9391,#9392,
#9393,#9394,#9395,#9396,#9397,#9398,#9399));
#9869=CLOSED_SHELL('',(#9400,#9401,#9402,#9403,#9404,#9405,#9406,#9407,
#9408,#9409,#9410,#9411,#9412,#9413,#9414,#9415,#9416,#9417,#9418,#9419,
#9420,#9421,#9422,#9423,#9424,#9425,#9426,#9427,#9428,#9429,#9430,#9431,
#9432,#9433,#9434,#9435,#9436,#9437,#9438,#9439,#9440,#9441,#9442,#9443,
#9444,#9445,#9446,#9447,#9448,#9449,#9450,#9451,#9452,#9453,#9454,#9455,
#9456,#9457,#9458,#9459,#9460,#9461,#9462,#9463,#9464,#9465,#9466));
#9870=CLOSED_SHELL('',(#9467,#9468,#9469,#9470,#9471,#9472,#9473,#9474,
#9475,#9476,#9477,#9478,#9479,#9480,#9481,#9482));
#9871=CLOSED_SHELL('',(#9483,#9484,#9485,#9486,#9487));
#9872=CLOSED_SHELL('',(#9488,#9489,#9490,#9491,#9492));
#9873=CLOSED_SHELL('',(#9493,#9494,#9495,#9496,#9497));
#9874=CLOSED_SHELL('',(#9498,#9499,#9500,#9501,#9502,#9503,#9504,#9505,
#9506,#9507,#9508,#9509,#9510,#9511,#9512,#9513,#9514,#9515,#9516,#9517,
#9518,#9519,#9520,#9521,#9522,#9523,#9524,#9525,#9526,#9527,#9528,#9529,
#9530,#9531,#9532,#9533,#9534,#9535,#9536,#9537,#9538,#9539,#9540,#9541,
#9542,#9543,#9544,#9545,#9546,#9547,#9548,#9549,#9550,#9551,#9552,#9553,
#9554,#9555,#9556,#9557,#9558,#9559,#9560,#9561,#9562,#9563,#9564,#9565,
#9566,#9567,#9568,#9569,#9570,#9571,#9572,#9573,#9574,#9575,#9576,#9577,
#9578,#9579,#9580,#9581,#9582,#9583,#9584,#9585,#9586,#9587,#9588,#9589,
#9590,#9591,#9592,#9593,#9594,#9595,#9596,#9597,#9598,#9599,#9600,#9601,
#9602,#9603,#9604,#9605,#9606,#9607));
#9875=CLOSED_SHELL('',(#9608,#9609,#9610,#9611,#9612));
#9876=CLOSED_SHELL('',(#9613,#9614,#9615,#9616,#9617,#9618,#9619,#9620,
#9621,#9622,#9623,#9624,#9625,#9626,#9627,#9628,#9629,#9630,#9631,#9632,
#9633,#9634,#9635,#9636,#9637));
#9877=CLOSED_SHELL('',(#9638,#9639,#9640,#9641,#9642));
#9878=CLOSED_SHELL('',(#9643,#9644,#9645,#9646,#9647,#9648,#9649,#9650,
#9651,#9652,#9653,#9654,#9655,#9656,#9657,#9658,#9659,#9660,#9661,#9662,
#9663,#9664,#9665,#9666,#9667,#9668,#9669,#9670,#9671,#9672,#9673,#9674,
#9675,#9676,#9677,#9678,#9679,#9680,#9681,#9682,#9683,#9684,#9685,#9686,
#9687,#9688,#9689,#9690,#9691,#9692,#9693,#9694));
#9879=CLOSED_SHELL('',(#9695,#9696,#9697,#9698,#9699,#9700,#9701,#9702,
#9703,#9704,#9705,#9706,#9707,#9708,#9709,#9710,#9711,#9712,#9713,#9714,
#9715,#9716,#9717,#9718,#9719,#9720,#9721,#9722,#9723,#9724,#9725,#9726,
#9727,#9728,#9729,#9730,#9731,#9732,#9733,#9734,#9735,#9736,#9737,#9738,
#9739,#9740,#9741,#9742,#9743,#9744,#9745,#9746,#9747,#9748,#9749,#9750,
#9751,#9752,#9753,#9754,#9755,#9756,#9757,#9758,#9759,#9760,#9761,#9762,
#9763,#9764,#9765,#9766,#9767,#9768,#9769,#9770,#9771,#9772,#9773,#9774,
#9775,#9776,#9777,#9778,#9779,#9780,#9781,#9782,#9783));
#9880=CLOSED_SHELL('',(#9784,#9785,#9786,#9787));
#9881=CLOSED_SHELL('',(#9788,#9789,#9790,#9791,#9792,#9793,#9794,#9795,
#9796,#9797,#9798,#9799,#9800,#9801,#9802,#9803,#9804,#9805,#9806,#9807,
#9808,#9809,#9810,#9811,#9812,#9813,#9814,#9815,#9816,#9817,#9818,#9819,
#9820,#9821,#9822,#9823,#9824,#9825,#9826,#9827,#9828,#9829,#9830,#9831,
#9832,#9833,#9834,#9835,#9836,#9837,#9838,#9839,#9840,#9841));
#9882=CLOSED_SHELL('',(#9842,#9843,#9844,#9845,#9846));
#9883=CLOSED_SHELL('',(#9847,#9848,#9849,#9850,#9851));
#9884=CLOSED_SHELL('',(#9852,#9853,#9854,#9855,#9856,#9857,#9858,#9859,
#9860,#9861,#9862,#9863,#9864));
#9885=DERIVED_UNIT_ELEMENT(#9925,1.);
#9886=DERIVED_UNIT_ELEMENT(#50082,-3.);
#9887=DERIVED_UNIT_ELEMENT(#9925,1.);
#9888=DERIVED_UNIT_ELEMENT(#50082,-3.);
#9889=DERIVED_UNIT_ELEMENT(#9925,1.);
#9890=DERIVED_UNIT_ELEMENT(#50082,-3.);
#9891=DERIVED_UNIT_ELEMENT(#9925,1.);
#9892=DERIVED_UNIT_ELEMENT(#50082,-3.);
#9893=DERIVED_UNIT_ELEMENT(#9925,1.);
#9894=DERIVED_UNIT_ELEMENT(#50082,-3.);
#9895=DERIVED_UNIT_ELEMENT(#9925,1.);
#9896=DERIVED_UNIT_ELEMENT(#50082,-3.);
#9897=DERIVED_UNIT_ELEMENT(#9925,1.);
#9898=DERIVED_UNIT_ELEMENT(#50082,-3.);
#9899=DERIVED_UNIT_ELEMENT(#9925,1.);
#9900=DERIVED_UNIT_ELEMENT(#50082,-3.);
#9901=DERIVED_UNIT_ELEMENT(#9925,1.);
#9902=DERIVED_UNIT_ELEMENT(#50082,-3.);
#9903=DERIVED_UNIT_ELEMENT(#9925,1.);
#9904=DERIVED_UNIT_ELEMENT(#50082,-3.);
#9905=DERIVED_UNIT_ELEMENT(#9925,1.);
#9906=DERIVED_UNIT_ELEMENT(#50082,-3.);
#9907=DERIVED_UNIT_ELEMENT(#9925,1.);
#9908=DERIVED_UNIT_ELEMENT(#50082,-3.);
#9909=DERIVED_UNIT_ELEMENT(#9925,1.);
#9910=DERIVED_UNIT_ELEMENT(#50082,-3.);
#9911=DERIVED_UNIT_ELEMENT(#9925,1.);
#9912=DERIVED_UNIT_ELEMENT(#50082,-3.);
#9913=DERIVED_UNIT_ELEMENT(#9925,1.);
#9914=DERIVED_UNIT_ELEMENT(#50082,-3.);
#9915=DERIVED_UNIT_ELEMENT(#9925,1.);
#9916=DERIVED_UNIT_ELEMENT(#50082,-3.);
#9917=DERIVED_UNIT_ELEMENT(#9925,1.);
#9918=DERIVED_UNIT_ELEMENT(#50082,-3.);
#9919=DERIVED_UNIT_ELEMENT(#9925,1.);
#9920=DERIVED_UNIT_ELEMENT(#50082,-3.);
#9921=DERIVED_UNIT_ELEMENT(#9925,1.);
#9922=DERIVED_UNIT_ELEMENT(#50082,-3.);
#9923=DERIVED_UNIT_ELEMENT(#9925,1.);
#9924=DERIVED_UNIT_ELEMENT(#50082,-3.);
#9925=(
MASS_UNIT()
NAMED_UNIT(*)
SI_UNIT(.KILO.,.GRAM.)
);
#9926=DERIVED_UNIT((#9885,#9886));
#9927=DERIVED_UNIT((#9887,#9888));
#9928=DERIVED_UNIT((#9889,#9890));
#9929=DERIVED_UNIT((#9891,#9892));
#9930=DERIVED_UNIT((#9893,#9894));
#9931=DERIVED_UNIT((#9895,#9896));
#9932=DERIVED_UNIT((#9897,#9898));
#9933=DERIVED_UNIT((#9899,#9900));
#9934=DERIVED_UNIT((#9901,#9902));
#9935=DERIVED_UNIT((#9903,#9904));
#9936=DERIVED_UNIT((#9905,#9906));
#9937=DERIVED_UNIT((#9907,#9908));
#9938=DERIVED_UNIT((#9909,#9910));
#9939=DERIVED_UNIT((#9911,#9912));
#9940=DERIVED_UNIT((#9913,#9914));
#9941=DERIVED_UNIT((#9915,#9916));
#9942=DERIVED_UNIT((#9917,#9918));
#9943=DERIVED_UNIT((#9919,#9920));
#9944=DERIVED_UNIT((#9921,#9922));
#9945=DERIVED_UNIT((#9923,#9924));
#9946=MEASURE_REPRESENTATION_ITEM('density measure',
POSITIVE_RATIO_MEASURE(7850.),#9926);
#9947=MEASURE_REPRESENTATION_ITEM('density measure',
POSITIVE_RATIO_MEASURE(7850.),#9927);
#9948=MEASURE_REPRESENTATION_ITEM('density measure',
POSITIVE_RATIO_MEASURE(7850.),#9928);
#9949=MEASURE_REPRESENTATION_ITEM('density measure',
POSITIVE_RATIO_MEASURE(7850.),#9929);
#9950=MEASURE_REPRESENTATION_ITEM('density measure',
POSITIVE_RATIO_MEASURE(7850.),#9930);
#9951=MEASURE_REPRESENTATION_ITEM('density measure',
POSITIVE_RATIO_MEASURE(7850.),#9931);
#9952=MEASURE_REPRESENTATION_ITEM('density measure',
POSITIVE_RATIO_MEASURE(7850.),#9932);
#9953=MEASURE_REPRESENTATION_ITEM('density measure',
POSITIVE_RATIO_MEASURE(7850.),#9933);
#9954=MEASURE_REPRESENTATION_ITEM('density measure',
POSITIVE_RATIO_MEASURE(7850.),#9934);
#9955=MEASURE_REPRESENTATION_ITEM('density measure',
POSITIVE_RATIO_MEASURE(7850.),#9935);
#9956=MEASURE_REPRESENTATION_ITEM('density measure',
POSITIVE_RATIO_MEASURE(7850.),#9936);
#9957=MEASURE_REPRESENTATION_ITEM('density measure',
POSITIVE_RATIO_MEASURE(7850.),#9937);
#9958=MEASURE_REPRESENTATION_ITEM('density measure',
POSITIVE_RATIO_MEASURE(7850.),#9938);
#9959=MEASURE_REPRESENTATION_ITEM('density measure',
POSITIVE_RATIO_MEASURE(7850.),#9939);
#9960=MEASURE_REPRESENTATION_ITEM('density measure',
POSITIVE_RATIO_MEASURE(7850.),#9940);
#9961=MEASURE_REPRESENTATION_ITEM('density measure',
POSITIVE_RATIO_MEASURE(7850.),#9941);
#9962=MEASURE_REPRESENTATION_ITEM('density measure',
POSITIVE_RATIO_MEASURE(7850.),#9942);
#9963=MEASURE_REPRESENTATION_ITEM('density measure',
POSITIVE_RATIO_MEASURE(7850.),#9943);
#9964=MEASURE_REPRESENTATION_ITEM('density measure',
POSITIVE_RATIO_MEASURE(7850.),#9944);
#9965=MEASURE_REPRESENTATION_ITEM('density measure',
POSITIVE_RATIO_MEASURE(7850.),#9945);
#9966=PROPERTY_DEFINITION_REPRESENTATION(#10066,#10006);
#9967=PROPERTY_DEFINITION_REPRESENTATION(#10067,#10007);
#9968=PROPERTY_DEFINITION_REPRESENTATION(#10068,#10008);
#9969=PROPERTY_DEFINITION_REPRESENTATION(#10069,#10009);
#9970=PROPERTY_DEFINITION_REPRESENTATION(#10070,#10010);
#9971=PROPERTY_DEFINITION_REPRESENTATION(#10071,#10011);
#9972=PROPERTY_DEFINITION_REPRESENTATION(#10072,#10012);
#9973=PROPERTY_DEFINITION_REPRESENTATION(#10073,#10013);
#9974=PROPERTY_DEFINITION_REPRESENTATION(#10074,#10014);
#9975=PROPERTY_DEFINITION_REPRESENTATION(#10075,#10015);
#9976=PROPERTY_DEFINITION_REPRESENTATION(#10076,#10016);
#9977=PROPERTY_DEFINITION_REPRESENTATION(#10077,#10017);
#9978=PROPERTY_DEFINITION_REPRESENTATION(#10078,#10018);
#9979=PROPERTY_DEFINITION_REPRESENTATION(#10079,#10019);
#9980=PROPERTY_DEFINITION_REPRESENTATION(#10080,#10020);
#9981=PROPERTY_DEFINITION_REPRESENTATION(#10081,#10021);
#9982=PROPERTY_DEFINITION_REPRESENTATION(#10082,#10022);
#9983=PROPERTY_DEFINITION_REPRESENTATION(#10083,#10023);
#9984=PROPERTY_DEFINITION_REPRESENTATION(#10084,#10024);
#9985=PROPERTY_DEFINITION_REPRESENTATION(#10085,#10025);
#9986=PROPERTY_DEFINITION_REPRESENTATION(#10086,#10026);
#9987=PROPERTY_DEFINITION_REPRESENTATION(#10087,#10027);
#9988=PROPERTY_DEFINITION_REPRESENTATION(#10088,#10028);
#9989=PROPERTY_DEFINITION_REPRESENTATION(#10089,#10029);
#9990=PROPERTY_DEFINITION_REPRESENTATION(#10090,#10030);
#9991=PROPERTY_DEFINITION_REPRESENTATION(#10091,#10031);
#9992=PROPERTY_DEFINITION_REPRESENTATION(#10092,#10032);
#9993=PROPERTY_DEFINITION_REPRESENTATION(#10093,#10033);
#9994=PROPERTY_DEFINITION_REPRESENTATION(#10094,#10034);
#9995=PROPERTY_DEFINITION_REPRESENTATION(#10095,#10035);
#9996=PROPERTY_DEFINITION_REPRESENTATION(#10096,#10036);
#9997=PROPERTY_DEFINITION_REPRESENTATION(#10097,#10037);
#9998=PROPERTY_DEFINITION_REPRESENTATION(#10098,#10038);
#9999=PROPERTY_DEFINITION_REPRESENTATION(#10099,#10039);
#10000=PROPERTY_DEFINITION_REPRESENTATION(#10100,#10040);
#10001=PROPERTY_DEFINITION_REPRESENTATION(#10101,#10041);
#10002=PROPERTY_DEFINITION_REPRESENTATION(#10102,#10042);
#10003=PROPERTY_DEFINITION_REPRESENTATION(#10103,#10043);
#10004=PROPERTY_DEFINITION_REPRESENTATION(#10104,#10044);
#10005=PROPERTY_DEFINITION_REPRESENTATION(#10105,#10045);
#10006=REPRESENTATION('material name',(#10046),#50061);
#10007=REPRESENTATION('density',(#9946),#50061);
#10008=REPRESENTATION('material name',(#10047),#50062);
#10009=REPRESENTATION('density',(#9947),#50062);
#10010=REPRESENTATION('material name',(#10048),#50063);
#10011=REPRESENTATION('density',(#9948),#50063);
#10012=REPRESENTATION('material name',(#10049),#50064);
#10013=REPRESENTATION('density',(#9949),#50064);
#10014=REPRESENTATION('material name',(#10050),#50065);
#10015=REPRESENTATION('density',(#9950),#50065);
#10016=REPRESENTATION('material name',(#10051),#50066);
#10017=REPRESENTATION('density',(#9951),#50066);
#10018=REPRESENTATION('material name',(#10052),#50067);
#10019=REPRESENTATION('density',(#9952),#50067);
#10020=REPRESENTATION('material name',(#10053),#50068);
#10021=REPRESENTATION('density',(#9953),#50068);
#10022=REPRESENTATION('material name',(#10054),#50069);
#10023=REPRESENTATION('density',(#9954),#50069);
#10024=REPRESENTATION('material name',(#10055),#50070);
#10025=REPRESENTATION('density',(#9955),#50070);
#10026=REPRESENTATION('material name',(#10056),#50071);
#10027=REPRESENTATION('density',(#9956),#50071);
#10028=REPRESENTATION('material name',(#10057),#50072);
#10029=REPRESENTATION('density',(#9957),#50072);
#10030=REPRESENTATION('material name',(#10058),#50073);
#10031=REPRESENTATION('density',(#9958),#50073);
#10032=REPRESENTATION('material name',(#10059),#50074);
#10033=REPRESENTATION('density',(#9959),#50074);
#10034=REPRESENTATION('material name',(#10060),#50075);
#10035=REPRESENTATION('density',(#9960),#50075);
#10036=REPRESENTATION('material name',(#10061),#50076);
#10037=REPRESENTATION('density',(#9961),#50076);
#10038=REPRESENTATION('material name',(#10062),#50077);
#10039=REPRESENTATION('density',(#9962),#50077);
#10040=REPRESENTATION('material name',(#10063),#50078);
#10041=REPRESENTATION('density',(#9963),#50078);
#10042=REPRESENTATION('material name',(#10064),#50079);
#10043=REPRESENTATION('density',(#9964),#50079);
#10044=REPRESENTATION('material name',(#10065),#50080);
#10045=REPRESENTATION('density',(#9965),#50080);
#10046=DESCRIPTIVE_REPRESENTATION_ITEM('Steel','Steel');
#10047=DESCRIPTIVE_REPRESENTATION_ITEM('Steel','Steel');
#10048=DESCRIPTIVE_REPRESENTATION_ITEM('Steel','Steel');
#10049=DESCRIPTIVE_REPRESENTATION_ITEM('Steel','Steel');
#10050=DESCRIPTIVE_REPRESENTATION_ITEM('Steel','Steel');
#10051=DESCRIPTIVE_REPRESENTATION_ITEM('Steel','Steel');
#10052=DESCRIPTIVE_REPRESENTATION_ITEM('Steel','Steel');
#10053=DESCRIPTIVE_REPRESENTATION_ITEM('Steel','Steel');
#10054=DESCRIPTIVE_REPRESENTATION_ITEM('Steel','Steel');
#10055=DESCRIPTIVE_REPRESENTATION_ITEM('Steel','Steel');
#10056=DESCRIPTIVE_REPRESENTATION_ITEM('Steel','Steel');
#10057=DESCRIPTIVE_REPRESENTATION_ITEM('Steel','Steel');
#10058=DESCRIPTIVE_REPRESENTATION_ITEM('Steel','Steel');
#10059=DESCRIPTIVE_REPRESENTATION_ITEM('Steel','Steel');
#10060=DESCRIPTIVE_REPRESENTATION_ITEM('Steel','Steel');
#10061=DESCRIPTIVE_REPRESENTATION_ITEM('Steel','Steel');
#10062=DESCRIPTIVE_REPRESENTATION_ITEM('Steel','Steel');
#10063=DESCRIPTIVE_REPRESENTATION_ITEM('Steel','Steel');
#10064=DESCRIPTIVE_REPRESENTATION_ITEM('Steel','Steel');
#10065=DESCRIPTIVE_REPRESENTATION_ITEM('Steel','Steel');
#10066=PROPERTY_DEFINITION('material property','material name',#50170);
#10067=PROPERTY_DEFINITION('material property','density of part',#50170);
#10068=PROPERTY_DEFINITION('material property','material name',#50171);
#10069=PROPERTY_DEFINITION('material property','density of part',#50171);
#10070=PROPERTY_DEFINITION('material property','material name',#50172);
#10071=PROPERTY_DEFINITION('material property','density of part',#50172);
#10072=PROPERTY_DEFINITION('material property','material name',#50173);
#10073=PROPERTY_DEFINITION('material property','density of part',#50173);
#10074=PROPERTY_DEFINITION('material property','material name',#50174);
#10075=PROPERTY_DEFINITION('material property','density of part',#50174);
#10076=PROPERTY_DEFINITION('material property','material name',#50175);
#10077=PROPERTY_DEFINITION('material property','density of part',#50175);
#10078=PROPERTY_DEFINITION('material property','material name',#50176);
#10079=PROPERTY_DEFINITION('material property','density of part',#50176);
#10080=PROPERTY_DEFINITION('material property','material name',#50177);
#10081=PROPERTY_DEFINITION('material property','density of part',#50177);
#10082=PROPERTY_DEFINITION('material property','material name',#50178);
#10083=PROPERTY_DEFINITION('material property','density of part',#50178);
#10084=PROPERTY_DEFINITION('material property','material name',#50179);
#10085=PROPERTY_DEFINITION('material property','density of part',#50179);
#10086=PROPERTY_DEFINITION('material property','material name',#50180);
#10087=PROPERTY_DEFINITION('material property','density of part',#50180);
#10088=PROPERTY_DEFINITION('material property','material name',#50181);
#10089=PROPERTY_DEFINITION('material property','density of part',#50181);
#10090=PROPERTY_DEFINITION('material property','material name',#50182);
#10091=PROPERTY_DEFINITION('material property','density of part',#50182);
#10092=PROPERTY_DEFINITION('material property','material name',#50183);
#10093=PROPERTY_DEFINITION('material property','density of part',#50183);
#10094=PROPERTY_DEFINITION('material property','material name',#50184);
#10095=PROPERTY_DEFINITION('material property','density of part',#50184);
#10096=PROPERTY_DEFINITION('material property','material name',#50185);
#10097=PROPERTY_DEFINITION('material property','density of part',#50185);
#10098=PROPERTY_DEFINITION('material property','material name',#50186);
#10099=PROPERTY_DEFINITION('material property','density of part',#50186);
#10100=PROPERTY_DEFINITION('material property','material name',#50187);
#10101=PROPERTY_DEFINITION('material property','density of part',#50187);
#10102=PROPERTY_DEFINITION('material property','material name',#50188);
#10103=PROPERTY_DEFINITION('material property','density of part',#50188);
#10104=PROPERTY_DEFINITION('material property','material name',#50189);
#10105=PROPERTY_DEFINITION('material property','density of part',#50189);
#10106=AXIS2_PLACEMENT_3D('',#13471,#11035,#11036);
#10107=AXIS2_PLACEMENT_3D('',#13472,#11037,#11038);
#10108=AXIS2_PLACEMENT_3D('',#13473,#11039,#11040);
#10109=AXIS2_PLACEMENT_3D('',#13475,#11041,#11042);
#10110=AXIS2_PLACEMENT_3D('',#13478,#11044,#11045);
#10111=AXIS2_PLACEMENT_3D('',#13479,#11046,#11047);
#10112=AXIS2_PLACEMENT_3D('',#13480,#11048,#11049);
#10113=AXIS2_PLACEMENT_3D('',#13481,#11050,#11051);
#10114=AXIS2_PLACEMENT_3D('',#13482,#11052,#11053);
#10115=AXIS2_PLACEMENT_3D('',#13484,#11054,#11055);
#10116=AXIS2_PLACEMENT_3D('',#13485,#11056,#11057);
#10117=AXIS2_PLACEMENT_3D('',#13487,#11058,#11059);
#10118=AXIS2_PLACEMENT_3D('',#13491,#11061,#11062);
#10119=AXIS2_PLACEMENT_3D('',#13492,#11063,#11064);
#10120=AXIS2_PLACEMENT_3D('',#13493,#11065,#11066);
#10121=AXIS2_PLACEMENT_3D('',#13495,#11067,#11068);
#10122=AXIS2_PLACEMENT_3D('',#13497,#11069,#11070);
#10123=AXIS2_PLACEMENT_3D('',#13498,#11071,#11072);
#10124=AXIS2_PLACEMENT_3D('',#13499,#11073,#11074);
#10125=AXIS2_PLACEMENT_3D('',#13501,#11076,#11077);
#10126=AXIS2_PLACEMENT_3D('',#13502,#11078,#11079);
#10127=AXIS2_PLACEMENT_3D('',#13503,#11080,#11081);
#10128=AXIS2_PLACEMENT_3D('',#13505,#11082,#11083);
#10129=AXIS2_PLACEMENT_3D('',#13506,#11084,#11085);
#10130=AXIS2_PLACEMENT_3D('',#13508,#11086,#11087);
#10131=AXIS2_PLACEMENT_3D('',#13512,#11089,#11090);
#10132=AXIS2_PLACEMENT_3D('',#13513,#11091,#11092);
#10133=AXIS2_PLACEMENT_3D('',#13514,#11093,#11094);
#10134=AXIS2_PLACEMENT_3D('',#13516,#11095,#11096);
#10135=AXIS2_PLACEMENT_3D('',#13518,#11097,#11098);
#10136=AXIS2_PLACEMENT_3D('',#13519,#11099,#11100);
#10137=AXIS2_PLACEMENT_3D('',#13520,#11101,#11102);
#10138=AXIS2_PLACEMENT_3D('',#13522,#11104,#11105);
#10139=AXIS2_PLACEMENT_3D('',#13523,#11106,#11107);
#10140=AXIS2_PLACEMENT_3D('',#13524,#11108,#11109);
#10141=AXIS2_PLACEMENT_3D('',#13526,#11110,#11111);
#10142=AXIS2_PLACEMENT_3D('',#13528,#11112,#11113);
#10143=AXIS2_PLACEMENT_3D('',#13529,#11114,#11115);
#10144=AXIS2_PLACEMENT_3D('',#13530,#11116,#11117);
#10145=AXIS2_PLACEMENT_3D('',#13532,#11118,#11119);
#10146=AXIS2_PLACEMENT_3D('',#13533,#11120,#11121);
#10147=AXIS2_PLACEMENT_3D('',#13536,#11122,#11123);
#10148=AXIS2_PLACEMENT_3D('',#13540,#11125,#11126);
#10149=AXIS2_PLACEMENT_3D('',#13544,#11128,#11129);
#10150=AXIS2_PLACEMENT_3D('',#13548,#11131,#11132);
#10151=AXIS2_PLACEMENT_3D('',#13552,#11134,#11135);
#10152=AXIS2_PLACEMENT_3D('',#13556,#11137,#11138);
#10153=AXIS2_PLACEMENT_3D('',#13560,#11140,#11141);
#10154=AXIS2_PLACEMENT_3D('',#13564,#11143,#11144);
#10155=AXIS2_PLACEMENT_3D('',#13567,#11146,#11147);
#10156=AXIS2_PLACEMENT_3D('',#13569,#11149,#11150);
#10157=AXIS2_PLACEMENT_3D('',#13571,#11151,#11152);
#10158=AXIS2_PLACEMENT_3D('',#13573,#11153,#11154);
#10159=AXIS2_PLACEMENT_3D('',#13574,#11155,#11156);
#10160=AXIS2_PLACEMENT_3D('',#13575,#11157,#11158);
#10161=AXIS2_PLACEMENT_3D('',#13579,#11160,#11161);
#10162=AXIS2_PLACEMENT_3D('',#13581,#11162,#11163);
#10163=AXIS2_PLACEMENT_3D('',#13585,#11165,#11166);
#10164=AXIS2_PLACEMENT_3D('',#13589,#11168,#11169);
#10165=AXIS2_PLACEMENT_3D('',#13593,#11171,#11172);
#10166=AXIS2_PLACEMENT_3D('',#13597,#11174,#11175);
#10167=AXIS2_PLACEMENT_3D('',#13599,#11176,#11177);
#10168=AXIS2_PLACEMENT_3D('',#13601,#11178,#11179);
#10169=AXIS2_PLACEMENT_3D('',#13605,#11181,#11182);
#10170=AXIS2_PLACEMENT_3D('',#13609,#11184,#11185);
#10171=AXIS2_PLACEMENT_3D('',#13613,#11187,#11188);
#10172=AXIS2_PLACEMENT_3D('',#13617,#11190,#11191);
#10173=AXIS2_PLACEMENT_3D('',#13619,#11192,#11193);
#10174=AXIS2_PLACEMENT_3D('',#13621,#11194,#11195);
#10175=AXIS2_PLACEMENT_3D('',#13625,#11197,#11198);
#10176=AXIS2_PLACEMENT_3D('',#13629,#11200,#11201);
#10177=AXIS2_PLACEMENT_3D('',#13633,#11203,#11204);
#10178=AXIS2_PLACEMENT_3D('',#13637,#11206,#11207);
#10179=AXIS2_PLACEMENT_3D('',#13639,#11208,#11209);
#10180=AXIS2_PLACEMENT_3D('',#13641,#11210,#11211);
#10181=AXIS2_PLACEMENT_3D('',#13645,#11213,#11214);
#10182=AXIS2_PLACEMENT_3D('',#13649,#11216,#11217);
#10183=AXIS2_PLACEMENT_3D('',#13653,#11219,#11220);
#10184=AXIS2_PLACEMENT_3D('',#13657,#11222,#11223);
#10185=AXIS2_PLACEMENT_3D('',#13658,#11224,#11225);
#10186=AXIS2_PLACEMENT_3D('',#13659,#11226,#11227);
#10187=AXIS2_PLACEMENT_3D('',#13661,#11228,#11229);
#10188=AXIS2_PLACEMENT_3D('',#13662,#11230,#11231);
#10189=AXIS2_PLACEMENT_3D('',#13670,#11234,#11235);
#10190=AXIS2_PLACEMENT_3D('',#13672,#11236,#11237);
#10191=AXIS2_PLACEMENT_3D('',#13677,#11238,#11239);
#10192=AXIS2_PLACEMENT_3D('',#13678,#11240,#11241);
#10193=AXIS2_PLACEMENT_3D('',#13680,#11243,#11244);
#10194=AXIS2_PLACEMENT_3D('',#13682,#11246,#11247);
#10195=AXIS2_PLACEMENT_3D('',#13690,#11250,#11251);
#10196=AXIS2_PLACEMENT_3D('',#13693,#11253,#11254);
#10197=AXIS2_PLACEMENT_3D('',#13694,#11255,#11256);
#10198=AXIS2_PLACEMENT_3D('',#13702,#11259,#11260);
#10199=AXIS2_PLACEMENT_3D('',#13704,#11261,#11262);
#10200=AXIS2_PLACEMENT_3D('',#13706,#11264,#11265);
#10201=AXIS2_PLACEMENT_3D('',#13712,#11267,#11268);
#10202=AXIS2_PLACEMENT_3D('',#13720,#11271,#11272);
#10203=AXIS2_PLACEMENT_3D('',#13722,#11273,#11274);
#10204=AXIS2_PLACEMENT_3D('',#13724,#11276,#11277);
#10205=AXIS2_PLACEMENT_3D('',#13726,#11278,#11279);
#10206=AXIS2_PLACEMENT_3D('',#13730,#11280,#11281);
#10207=AXIS2_PLACEMENT_3D('',#13736,#11283,#11284);
#10208=AXIS2_PLACEMENT_3D('',#13737,#11285,#11286);
#10209=AXIS2_PLACEMENT_3D('',#13738,#11287,#11288);
#10210=AXIS2_PLACEMENT_3D('',#13740,#11290,#11291);
#10211=AXIS2_PLACEMENT_3D('',#13744,#11294,#11295);
#10212=AXIS2_PLACEMENT_3D('',#13748,#11297,#11298);
#10213=AXIS2_PLACEMENT_3D('',#13751,#11301,#11302);
#10214=AXIS2_PLACEMENT_3D('',#13753,#11303,#11304);
#10215=AXIS2_PLACEMENT_3D('',#13755,#11306,#11307);
#10216=AXIS2_PLACEMENT_3D('',#13757,#11308,#11309);
#10217=AXIS2_PLACEMENT_3D('',#13758,#11310,#11311);
#10218=AXIS2_PLACEMENT_3D('',#13759,#11312,#11313);
#10219=AXIS2_PLACEMENT_3D('',#13768,#11317,#11318);
#10220=AXIS2_PLACEMENT_3D('',#13770,#11319,#11320);
#10221=AXIS2_PLACEMENT_3D('',#13775,#11321,#11322);
#10222=AXIS2_PLACEMENT_3D('',#13776,#11323,#11324);
#10223=AXIS2_PLACEMENT_3D('',#13778,#11326,#11327);
#10224=AXIS2_PLACEMENT_3D('',#13781,#11330,#11331);
#10225=AXIS2_PLACEMENT_3D('',#13783,#11333,#11334);
#10226=AXIS2_PLACEMENT_3D('',#13786,#11335,#11336);
#10227=AXIS2_PLACEMENT_3D('',#13790,#11340,#11341);
#10228=AXIS2_PLACEMENT_3D('',#13792,#11342,#11343);
#10229=AXIS2_PLACEMENT_3D('',#13794,#11344,#11345);
#10230=AXIS2_PLACEMENT_3D('',#13795,#11346,#11347);
#10231=AXIS2_PLACEMENT_3D('',#13796,#11348,#11349);
#10232=AXIS2_PLACEMENT_3D('',#13798,#11351,#11352);
#10233=AXIS2_PLACEMENT_3D('',#13801,#11355,#11356);
#10234=AXIS2_PLACEMENT_3D('',#13803,#11358,#11359);
#10235=AXIS2_PLACEMENT_3D('',#13812,#11363,#11364);
#10236=AXIS2_PLACEMENT_3D('',#13814,#11365,#11366);
#10237=AXIS2_PLACEMENT_3D('',#13818,#11367,#11368);
#10238=AXIS2_PLACEMENT_3D('',#13819,#11369,#11370);
#10239=AXIS2_PLACEMENT_3D('',#13821,#11372,#11373);
#10240=AXIS2_PLACEMENT_3D('',#13824,#11376,#11377);
#10241=AXIS2_PLACEMENT_3D('',#13826,#11379,#11380);
#10242=AXIS2_PLACEMENT_3D('',#13828,#11382,#11383);
#10243=AXIS2_PLACEMENT_3D('',#13830,#11385,#11386);
#10244=AXIS2_PLACEMENT_3D('',#13832,#11388,#11389);
#10245=AXIS2_PLACEMENT_3D('',#13834,#11391,#11392);
#10246=AXIS2_PLACEMENT_3D('',#13836,#11394,#11395);
#10247=AXIS2_PLACEMENT_3D('',#13838,#11397,#11398);
#10248=AXIS2_PLACEMENT_3D('',#13840,#11400,#11401);
#10249=AXIS2_PLACEMENT_3D('',#13842,#11403,#11404);
#10250=AXIS2_PLACEMENT_3D('',#13843,#11405,#11406);
#10251=AXIS2_PLACEMENT_3D('',#13844,#11407,#11408);
#10252=AXIS2_PLACEMENT_3D('',#13845,#11409,#11410);
#10253=AXIS2_PLACEMENT_3D('',#13846,#11411,#11412);
#10254=AXIS2_PLACEMENT_3D('',#13848,#11414,#11415);
#10255=AXIS2_PLACEMENT_3D('',#13850,#11417,#11418);
#10256=AXIS2_PLACEMENT_3D('',#13852,#11420,#11421);
#10257=AXIS2_PLACEMENT_3D('',#13853,#11422,#11423);
#10258=AXIS2_PLACEMENT_3D('',#13854,#11424,#11425);
#10259=AXIS2_PLACEMENT_3D('',#13855,#11426,#11427);
#10260=AXIS2_PLACEMENT_3D('',#13857,#11429,#11430);
#10261=AXIS2_PLACEMENT_3D('',#13858,#11431,#11432);
#10262=AXIS2_PLACEMENT_3D('',#13860,#11434,#11435);
#10263=AXIS2_PLACEMENT_3D('',#13861,#11436,#11437);
#10264=AXIS2_PLACEMENT_3D('',#13863,#11439,#11440);
#10265=AXIS2_PLACEMENT_3D('',#13864,#11441,#11442);
#10266=AXIS2_PLACEMENT_3D('',#13865,#11443,#11444);
#10267=AXIS2_PLACEMENT_3D('',#14394,#11445,#11446);
#10268=AXIS2_PLACEMENT_3D('',#15155,#11447,#11448);
#10269=AXIS2_PLACEMENT_3D('',#15340,#11449,#11450);
#10270=AXIS2_PLACEMENT_3D('',#15832,#11451,#11452);
#10271=AXIS2_PLACEMENT_3D('',#16542,#11453,#11454);
#10272=AXIS2_PLACEMENT_3D('',#16778,#11455,#11456);
#10273=AXIS2_PLACEMENT_3D('',#16779,#11457,#11458);
#10274=AXIS2_PLACEMENT_3D('',#16781,#11459,#11460);
#10275=AXIS2_PLACEMENT_3D('',#16784,#11462,#11463);
#10276=AXIS2_PLACEMENT_3D('',#16785,#11464,#11465);
#10277=AXIS2_PLACEMENT_3D('',#16787,#11466,#11467);
#10278=AXIS2_PLACEMENT_3D('',#16788,#11468,#11469);
#10279=AXIS2_PLACEMENT_3D('',#16792,#11471,#11472);
#10280=AXIS2_PLACEMENT_3D('',#16793,#11473,#11474);
#10281=AXIS2_PLACEMENT_3D('',#16794,#11475,#11476);
#10282=AXIS2_PLACEMENT_3D('',#16796,#11477,#11478);
#10283=AXIS2_PLACEMENT_3D('',#16799,#11480,#11481);
#10284=AXIS2_PLACEMENT_3D('',#16800,#11482,#11483);
#10285=AXIS2_PLACEMENT_3D('',#16803,#11485,#11486);
#10286=AXIS2_PLACEMENT_3D('',#16804,#11487,#11488);
#10287=AXIS2_PLACEMENT_3D('',#16806,#11489,#11490);
#10288=AXIS2_PLACEMENT_3D('',#16807,#11491,#11492);
#10289=AXIS2_PLACEMENT_3D('',#16809,#11494,#11495);
#10290=AXIS2_PLACEMENT_3D('',#16812,#11496,#11497);
#10291=AXIS2_PLACEMENT_3D('',#16814,#11499,#11500);
#10292=AXIS2_PLACEMENT_3D('',#16815,#11501,#11502);
#10293=AXIS2_PLACEMENT_3D('',#16819,#11504,#11505);
#10294=AXIS2_PLACEMENT_3D('',#16820,#11506,#11507);
#10295=AXIS2_PLACEMENT_3D('',#16821,#11508,#11509);
#10296=AXIS2_PLACEMENT_3D('',#17807,#11510,#11511);
#10297=AXIS2_PLACEMENT_3D('',#17809,#11513,#11514);
#10298=AXIS2_PLACEMENT_3D('',#17811,#11515,#11516);
#10299=AXIS2_PLACEMENT_3D('',#17813,#11517,#11518);
#10300=AXIS2_PLACEMENT_3D('',#17814,#11519,#11520);
#10301=AXIS2_PLACEMENT_3D('',#17816,#11521,#11522);
#10302=AXIS2_PLACEMENT_3D('',#17818,#11523,#11524);
#10303=AXIS2_PLACEMENT_3D('',#17819,#11525,#11526);
#10304=AXIS2_PLACEMENT_3D('',#17821,#11527,#11528);
#10305=AXIS2_PLACEMENT_3D('',#17823,#11529,#11530);
#10306=AXIS2_PLACEMENT_3D('',#17824,#11531,#11532);
#10307=AXIS2_PLACEMENT_3D('',#17826,#11533,#11534);
#10308=AXIS2_PLACEMENT_3D('',#17828,#11535,#11536);
#10309=AXIS2_PLACEMENT_3D('',#17829,#11537,#11538);
#10310=AXIS2_PLACEMENT_3D('',#17831,#11539,#11540);
#10311=AXIS2_PLACEMENT_3D('',#17833,#11541,#11542);
#10312=AXIS2_PLACEMENT_3D('',#17834,#11543,#11544);
#10313=AXIS2_PLACEMENT_3D('',#17836,#11545,#11546);
#10314=AXIS2_PLACEMENT_3D('',#17838,#11547,#11548);
#10315=AXIS2_PLACEMENT_3D('',#17839,#11549,#11550);
#10316=AXIS2_PLACEMENT_3D('',#17841,#11551,#11552);
#10317=AXIS2_PLACEMENT_3D('',#17843,#11553,#11554);
#10318=AXIS2_PLACEMENT_3D('',#17844,#11555,#11556);
#10319=AXIS2_PLACEMENT_3D('',#17846,#11557,#11558);
#10320=AXIS2_PLACEMENT_3D('',#17848,#11559,#11560);
#10321=AXIS2_PLACEMENT_3D('',#17849,#11561,#11562);
#10322=AXIS2_PLACEMENT_3D('',#17851,#11563,#11564);
#10323=AXIS2_PLACEMENT_3D('',#17853,#11565,#11566);
#10324=AXIS2_PLACEMENT_3D('',#17854,#11567,#11568);
#10325=AXIS2_PLACEMENT_3D('',#17856,#11569,#11570);
#10326=AXIS2_PLACEMENT_3D('',#17858,#11571,#11572);
#10327=AXIS2_PLACEMENT_3D('',#17859,#11573,#11574);
#10328=AXIS2_PLACEMENT_3D('',#17861,#11575,#11576);
#10329=AXIS2_PLACEMENT_3D('',#17863,#11577,#11578);
#10330=AXIS2_PLACEMENT_3D('',#17864,#11579,#11580);
#10331=AXIS2_PLACEMENT_3D('',#17866,#11581,#11582);
#10332=AXIS2_PLACEMENT_3D('',#17868,#11583,#11584);
#10333=AXIS2_PLACEMENT_3D('',#17869,#11585,#11586);
#10334=AXIS2_PLACEMENT_3D('',#17871,#11587,#11588);
#10335=AXIS2_PLACEMENT_3D('',#17873,#11589,#11590);
#10336=AXIS2_PLACEMENT_3D('',#17874,#11591,#11592);
#10337=AXIS2_PLACEMENT_3D('',#17876,#11593,#11594);
#10338=AXIS2_PLACEMENT_3D('',#17878,#11595,#11596);
#10339=AXIS2_PLACEMENT_3D('',#17879,#11597,#11598);
#10340=AXIS2_PLACEMENT_3D('',#17881,#11599,#11600);
#10341=AXIS2_PLACEMENT_3D('',#17883,#11601,#11602);
#10342=AXIS2_PLACEMENT_3D('',#17884,#11603,#11604);
#10343=AXIS2_PLACEMENT_3D('',#17886,#11605,#11606);
#10344=AXIS2_PLACEMENT_3D('',#17888,#11608,#11609);
#10345=AXIS2_PLACEMENT_3D('',#17890,#11611,#11612);
#10346=AXIS2_PLACEMENT_3D('',#17892,#11614,#11615);
#10347=AXIS2_PLACEMENT_3D('',#17894,#11617,#11618);
#10348=AXIS2_PLACEMENT_3D('',#17896,#11620,#11621);
#10349=AXIS2_PLACEMENT_3D('',#17898,#11623,#11624);
#10350=AXIS2_PLACEMENT_3D('',#17900,#11626,#11627);
#10351=AXIS2_PLACEMENT_3D('',#17902,#11629,#11630);
#10352=AXIS2_PLACEMENT_3D('',#17905,#11632,#11633);
#10353=AXIS2_PLACEMENT_3D('',#17906,#11634,#11635);
#10354=AXIS2_PLACEMENT_3D('',#17908,#11637,#11638);
#10355=AXIS2_PLACEMENT_3D('',#17910,#11640,#11641);
#10356=AXIS2_PLACEMENT_3D('',#17912,#11643,#11644);
#10357=AXIS2_PLACEMENT_3D('',#17914,#11646,#11647);
#10358=AXIS2_PLACEMENT_3D('',#17916,#11649,#11650);
#10359=AXIS2_PLACEMENT_3D('',#17918,#11652,#11653);
#10360=AXIS2_PLACEMENT_3D('',#17919,#11654,#11655);
#10361=AXIS2_PLACEMENT_3D('',#17921,#11656,#11657);
#10362=AXIS2_PLACEMENT_3D('',#17924,#11659,#11660);
#10363=AXIS2_PLACEMENT_3D('',#17925,#11661,#11662);
#10364=AXIS2_PLACEMENT_3D('',#17927,#11663,#11664);
#10365=AXIS2_PLACEMENT_3D('',#17930,#11666,#11667);
#10366=AXIS2_PLACEMENT_3D('',#17931,#11668,#11669);
#10367=AXIS2_PLACEMENT_3D('',#17933,#11670,#11671);
#10368=AXIS2_PLACEMENT_3D('',#17936,#11673,#11674);
#10369=AXIS2_PLACEMENT_3D('',#17937,#11675,#11676);
#10370=AXIS2_PLACEMENT_3D('',#17939,#11677,#11678);
#10371=AXIS2_PLACEMENT_3D('',#17942,#11680,#11681);
#10372=AXIS2_PLACEMENT_3D('',#17943,#11682,#11683);
#10373=AXIS2_PLACEMENT_3D('',#17945,#11685,#11686);
#10374=AXIS2_PLACEMENT_3D('',#17947,#11687,#11688);
#10375=AXIS2_PLACEMENT_3D('',#17948,#11689,#11690);
#10376=AXIS2_PLACEMENT_3D('',#17950,#11691,#11692);
#10377=AXIS2_PLACEMENT_3D('',#17952,#11694,#11695);
#10378=AXIS2_PLACEMENT_3D('',#17953,#11696,#11697);
#10379=AXIS2_PLACEMENT_3D('',#17955,#11698,#11699);
#10380=AXIS2_PLACEMENT_3D('',#17956,#11700,#11701);
#10381=AXIS2_PLACEMENT_3D('',#17958,#11702,#11703);
#10382=AXIS2_PLACEMENT_3D('',#17960,#11705,#11706);
#10383=AXIS2_PLACEMENT_3D('',#17961,#11707,#11708);
#10384=AXIS2_PLACEMENT_3D('',#17963,#11709,#11710);
#10385=AXIS2_PLACEMENT_3D('',#17964,#11711,#11712);
#10386=AXIS2_PLACEMENT_3D('',#17966,#11713,#11714);
#10387=AXIS2_PLACEMENT_3D('',#17968,#11716,#11717);
#10388=AXIS2_PLACEMENT_3D('',#17969,#11718,#11719);
#10389=AXIS2_PLACEMENT_3D('',#17971,#11720,#11721);
#10390=AXIS2_PLACEMENT_3D('',#17972,#11722,#11723);
#10391=AXIS2_PLACEMENT_3D('',#17974,#11724,#11725);
#10392=AXIS2_PLACEMENT_3D('',#17976,#11727,#11728);
#10393=AXIS2_PLACEMENT_3D('',#17977,#11729,#11730);
#10394=AXIS2_PLACEMENT_3D('',#17979,#11731,#11732);
#10395=AXIS2_PLACEMENT_3D('',#17981,#11733,#11734);
#10396=AXIS2_PLACEMENT_3D('',#17982,#11735,#11736);
#10397=AXIS2_PLACEMENT_3D('',#17984,#11737,#11738);
#10398=AXIS2_PLACEMENT_3D('',#17986,#11740,#11741);
#10399=AXIS2_PLACEMENT_3D('',#17987,#11742,#11743);
#10400=AXIS2_PLACEMENT_3D('',#17989,#11745,#11746);
#10401=AXIS2_PLACEMENT_3D('',#17990,#11747,#11748);
#10402=AXIS2_PLACEMENT_3D('',#17997,#11751,#11752);
#10403=AXIS2_PLACEMENT_3D('',#17999,#11754,#11755);
#10404=AXIS2_PLACEMENT_3D('',#18002,#11757,#11758);
#10405=AXIS2_PLACEMENT_3D('',#18003,#11759,#11760);
#10406=AXIS2_PLACEMENT_3D('',#18006,#11761,#11762);
#10407=AXIS2_PLACEMENT_3D('',#18012,#11766,#11767);
#10408=AXIS2_PLACEMENT_3D('',#18014,#11768,#11769);
#10409=AXIS2_PLACEMENT_3D('',#18016,#11771,#11772);
#10410=AXIS2_PLACEMENT_3D('',#18020,#11774,#11775);
#10411=AXIS2_PLACEMENT_3D('',#18023,#11777,#11778);
#10412=AXIS2_PLACEMENT_3D('',#18024,#11779,#11780);
#10413=AXIS2_PLACEMENT_3D('',#18030,#11784,#11785);
#10414=AXIS2_PLACEMENT_3D('',#18038,#11790,#11791);
#10415=AXIS2_PLACEMENT_3D('',#18047,#11796,#11797);
#10416=AXIS2_PLACEMENT_3D('',#18056,#11802,#11803);
#10417=AXIS2_PLACEMENT_3D('',#18059,#11806,#11807);
#10418=AXIS2_PLACEMENT_3D('',#18060,#11808,#11809);
#10419=AXIS2_PLACEMENT_3D('',#18061,#11810,#11811);
#10420=AXIS2_PLACEMENT_3D('',#18062,#11812,#11813);
#10421=AXIS2_PLACEMENT_3D('',#18064,#11814,#11815);
#10422=AXIS2_PLACEMENT_3D('',#18067,#11817,#11818);
#10423=AXIS2_PLACEMENT_3D('',#18068,#11819,#11820);
#10424=AXIS2_PLACEMENT_3D('',#18071,#11823,#11824);
#10425=AXIS2_PLACEMENT_3D('',#18074,#11827,#11828);
#10426=AXIS2_PLACEMENT_3D('',#18075,#11829,#11830);
#10427=AXIS2_PLACEMENT_3D('',#18076,#11831,#11832);
#10428=AXIS2_PLACEMENT_3D('',#18077,#11833,#11834);
#10429=AXIS2_PLACEMENT_3D('',#18079,#11835,#11836);
#10430=AXIS2_PLACEMENT_3D('',#18080,#11837,#11838);
#10431=AXIS2_PLACEMENT_3D('',#18082,#11839,#11840);
#10432=AXIS2_PLACEMENT_3D('',#18086,#11842,#11843);
#10433=AXIS2_PLACEMENT_3D('',#18087,#11844,#11845);
#10434=AXIS2_PLACEMENT_3D('',#18088,#11846,#11847);
#10435=AXIS2_PLACEMENT_3D('',#18090,#11848,#11849);
#10436=AXIS2_PLACEMENT_3D('',#18092,#11850,#11851);
#10437=AXIS2_PLACEMENT_3D('',#18093,#11852,#11853);
#10438=AXIS2_PLACEMENT_3D('',#18094,#11854,#11855);
#10439=AXIS2_PLACEMENT_3D('',#18096,#11857,#11858);
#10440=AXIS2_PLACEMENT_3D('',#18097,#11859,#11860);
#10441=AXIS2_PLACEMENT_3D('',#18098,#11861,#11862);
#10442=AXIS2_PLACEMENT_3D('',#18100,#11863,#11864);
#10443=AXIS2_PLACEMENT_3D('',#18104,#11866,#11867);
#10444=AXIS2_PLACEMENT_3D('',#18105,#11868,#11869);
#10445=AXIS2_PLACEMENT_3D('',#18106,#11870,#11871);
#10446=AXIS2_PLACEMENT_3D('',#18108,#11872,#11873);
#10447=AXIS2_PLACEMENT_3D('',#18110,#11874,#11875);
#10448=AXIS2_PLACEMENT_3D('',#18111,#11876,#11877);
#10449=AXIS2_PLACEMENT_3D('',#18112,#11878,#11879);
#10450=AXIS2_PLACEMENT_3D('',#18115,#11881,#11882);
#10451=AXIS2_PLACEMENT_3D('',#18116,#11883,#11884);
#10452=AXIS2_PLACEMENT_3D('',#18117,#11885,#11886);
#10453=AXIS2_PLACEMENT_3D('',#18118,#11887,#11888);
#10454=AXIS2_PLACEMENT_3D('',#18119,#11889,#11890);
#10455=AXIS2_PLACEMENT_3D('',#18121,#11891,#11892);
#10456=AXIS2_PLACEMENT_3D('',#18125,#11894,#11895);
#10457=AXIS2_PLACEMENT_3D('',#18126,#11896,#11897);
#10458=AXIS2_PLACEMENT_3D('',#18127,#11898,#11899);
#10459=AXIS2_PLACEMENT_3D('',#18129,#11900,#11901);
#10460=AXIS2_PLACEMENT_3D('',#18131,#11902,#11903);
#10461=AXIS2_PLACEMENT_3D('',#18132,#11904,#11905);
#10462=AXIS2_PLACEMENT_3D('',#18133,#11906,#11907);
#10463=AXIS2_PLACEMENT_3D('',#18136,#11909,#11910);
#10464=AXIS2_PLACEMENT_3D('',#18137,#11911,#11912);
#10465=AXIS2_PLACEMENT_3D('',#18138,#11913,#11914);
#10466=AXIS2_PLACEMENT_3D('',#18139,#11915,#11916);
#10467=AXIS2_PLACEMENT_3D('',#18140,#11917,#11918);
#10468=AXIS2_PLACEMENT_3D('',#18220,#11920,#11921);
#10469=AXIS2_PLACEMENT_3D('',#18589,#11923,#11924);
#10470=AXIS2_PLACEMENT_3D('',#18954,#11926,#11927);
#10471=AXIS2_PLACEMENT_3D('',#19314,#11929,#11930);
#10472=AXIS2_PLACEMENT_3D('',#19674,#11932,#11933);
#10473=AXIS2_PLACEMENT_3D('',#20036,#11935,#11936);
#10474=AXIS2_PLACEMENT_3D('',#20409,#11938,#11939);
#10475=AXIS2_PLACEMENT_3D('',#20434,#11941,#11942);
#10476=AXIS2_PLACEMENT_3D('',#20533,#11943,#11944);
#10477=AXIS2_PLACEMENT_3D('',#20554,#11946,#11947);
#10478=AXIS2_PLACEMENT_3D('',#20643,#11948,#11949);
#10479=AXIS2_PLACEMENT_3D('',#21041,#11951,#11952);
#10480=AXIS2_PLACEMENT_3D('',#21463,#11954,#11955);
#10481=AXIS2_PLACEMENT_3D('',#21855,#11957,#11958);
#10482=AXIS2_PLACEMENT_3D('',#22277,#11960,#11961);
#10483=AXIS2_PLACEMENT_3D('',#22701,#11963,#11964);
#10484=AXIS2_PLACEMENT_3D('',#23107,#11966,#11967);
#10485=AXIS2_PLACEMENT_3D('',#23525,#11969,#11970);
#10486=AXIS2_PLACEMENT_3D('',#23927,#11972,#11973);
#10487=AXIS2_PLACEMENT_3D('',#24343,#11975,#11976);
#10488=AXIS2_PLACEMENT_3D('',#24742,#11978,#11979);
#10489=AXIS2_PLACEMENT_3D('',#25165,#11981,#11982);
#10490=AXIS2_PLACEMENT_3D('',#25190,#11984,#11985);
#10491=AXIS2_PLACEMENT_3D('',#25301,#11986,#11987);
#10492=AXIS2_PLACEMENT_3D('',#25354,#11989,#11990);
#10493=AXIS2_PLACEMENT_3D('',#25441,#11992,#11993);
#10494=AXIS2_PLACEMENT_3D('',#25656,#11995,#11996);
#10495=AXIS2_PLACEMENT_3D('',#25863,#11998,#11999);
#10496=AXIS2_PLACEMENT_3D('',#26070,#12001,#12002);
#10497=AXIS2_PLACEMENT_3D('',#26295,#12004,#12005);
#10498=AXIS2_PLACEMENT_3D('',#26326,#12007,#12008);
#10499=AXIS2_PLACEMENT_3D('',#26376,#12009,#12010);
#10500=AXIS2_PLACEMENT_3D('',#26407,#12012,#12013);
#10501=AXIS2_PLACEMENT_3D('',#26433,#12014,#12015);
#10502=AXIS2_PLACEMENT_3D('',#26535,#12017,#12018);
#10503=AXIS2_PLACEMENT_3D('',#26637,#12020,#12021);
#10504=AXIS2_PLACEMENT_3D('',#26739,#12023,#12024);
#10505=AXIS2_PLACEMENT_3D('',#26847,#12026,#12027);
#10506=AXIS2_PLACEMENT_3D('',#26949,#12029,#12030);
#10507=AXIS2_PLACEMENT_3D('',#27051,#12032,#12033);
#10508=AXIS2_PLACEMENT_3D('',#27165,#12035,#12036);
#10509=AXIS2_PLACEMENT_3D('',#27264,#12038,#12039);
#10510=AXIS2_PLACEMENT_3D('',#27366,#12041,#12042);
#10511=AXIS2_PLACEMENT_3D('',#27468,#12044,#12045);
#10512=AXIS2_PLACEMENT_3D('',#27499,#12047,#12048);
#10513=AXIS2_PLACEMENT_3D('',#27549,#12049,#12050);
#10514=AXIS2_PLACEMENT_3D('',#27633,#12051,#12052);
#10515=AXIS2_PLACEMENT_3D('',#27855,#12053,#12054);
#10516=AXIS2_PLACEMENT_3D('',#27864,#12059,#12060);
#10517=AXIS2_PLACEMENT_3D('',#27870,#12064,#12065);
#10518=AXIS2_PLACEMENT_3D('',#27876,#12069,#12070);
#10519=AXIS2_PLACEMENT_3D('',#27893,#12075,#12076);
#10520=AXIS2_PLACEMENT_3D('',#27894,#12077,#12078);
#10521=AXIS2_PLACEMENT_3D('',#27898,#12081,#12082);
#10522=AXIS2_PLACEMENT_3D('',#27908,#12087,#12088);
#10523=AXIS2_PLACEMENT_3D('',#27909,#12089,#12090);
#10524=AXIS2_PLACEMENT_3D('',#27911,#12091,#12092);
#10525=AXIS2_PLACEMENT_3D('',#27913,#12093,#12094);
#10526=AXIS2_PLACEMENT_3D('',#27914,#12095,#12096);
#10527=AXIS2_PLACEMENT_3D('',#27916,#12098,#12099);
#10528=AXIS2_PLACEMENT_3D('',#27918,#12101,#12102);
#10529=AXIS2_PLACEMENT_3D('',#27921,#12103,#12104);
#10530=AXIS2_PLACEMENT_3D('',#27926,#12107,#12108);
#10531=AXIS2_PLACEMENT_3D('',#27935,#12113,#12114);
#10532=AXIS2_PLACEMENT_3D('',#27936,#12115,#12116);
#10533=AXIS2_PLACEMENT_3D('',#27938,#12117,#12118);
#10534=AXIS2_PLACEMENT_3D('',#27940,#12120,#12121);
#10535=AXIS2_PLACEMENT_3D('',#27942,#12122,#12123);
#10536=AXIS2_PLACEMENT_3D('',#27944,#12124,#12125);
#10537=AXIS2_PLACEMENT_3D('',#27946,#12127,#12128);
#10538=AXIS2_PLACEMENT_3D('',#27948,#12129,#12130);
#10539=AXIS2_PLACEMENT_3D('',#27952,#12131,#12132);
#10540=AXIS2_PLACEMENT_3D('',#27955,#12133,#12134);
#10541=AXIS2_PLACEMENT_3D('',#27967,#12141,#12142);
#10542=AXIS2_PLACEMENT_3D('',#27968,#12143,#12144);
#10543=AXIS2_PLACEMENT_3D('',#27972,#12145,#12146);
#10544=AXIS2_PLACEMENT_3D('',#27974,#12148,#12149);
#10545=AXIS2_PLACEMENT_3D('',#27977,#12150,#12151);
#10546=AXIS2_PLACEMENT_3D('',#27978,#12152,#12153);
#10547=AXIS2_PLACEMENT_3D('',#27980,#12155,#12156);
#10548=AXIS2_PLACEMENT_3D('',#27981,#12157,#12158);
#10549=AXIS2_PLACEMENT_3D('',#27986,#12160,#12161);
#10550=AXIS2_PLACEMENT_3D('',#27992,#12165,#12166);
#10551=AXIS2_PLACEMENT_3D('',#27994,#12168,#12169);
#10552=AXIS2_PLACEMENT_3D('',#27996,#12171,#12172);
#10553=AXIS2_PLACEMENT_3D('',#28005,#12176,#12177);
#10554=AXIS2_PLACEMENT_3D('',#28011,#12181,#12182);
#10555=AXIS2_PLACEMENT_3D('',#28017,#12186,#12187);
#10556=AXIS2_PLACEMENT_3D('',#28074,#12190,#12191);
#10557=AXIS2_PLACEMENT_3D('',#28076,#12192,#12193);
#10558=AXIS2_PLACEMENT_3D('',#28078,#12195,#12196);
#10559=AXIS2_PLACEMENT_3D('',#28087,#12200,#12201);
#10560=AXIS2_PLACEMENT_3D('',#28091,#12204,#12205);
#10561=AXIS2_PLACEMENT_3D('',#28097,#12209,#12210);
#10562=AXIS2_PLACEMENT_3D('',#28099,#12211,#12212);
#10563=AXIS2_PLACEMENT_3D('',#28101,#12214,#12215);
#10564=AXIS2_PLACEMENT_3D('',#28652,#12216,#12217);
#10565=AXIS2_PLACEMENT_3D('',#29266,#12218,#12219);
#10566=AXIS2_PLACEMENT_3D('',#29269,#12220,#12221);
#10567=AXIS2_PLACEMENT_3D('',#29305,#12222,#12223);
#10568=AXIS2_PLACEMENT_3D('',#29353,#12224,#12225);
#10569=AXIS2_PLACEMENT_3D('',#29354,#12226,#12227);
#10570=AXIS2_PLACEMENT_3D('',#29356,#12229,#12230);
#10571=AXIS2_PLACEMENT_3D('',#29357,#12231,#12232);
#10572=AXIS2_PLACEMENT_3D('',#29359,#12234,#12235);
#10573=AXIS2_PLACEMENT_3D('',#29363,#12238,#12239);
#10574=AXIS2_PLACEMENT_3D('',#29365,#12240,#12241);
#10575=AXIS2_PLACEMENT_3D('',#29366,#12242,#12243);
#10576=AXIS2_PLACEMENT_3D('',#29368,#12245,#12246);
#10577=AXIS2_PLACEMENT_3D('',#29370,#12248,#12249);
#10578=AXIS2_PLACEMENT_3D('',#30511,#12250,#12251);
#10579=AXIS2_PLACEMENT_3D('',#30588,#12253,#12254);
#10580=AXIS2_PLACEMENT_3D('',#30608,#12256,#12257);
#10581=AXIS2_PLACEMENT_3D('',#30659,#12258,#12259);
#10582=AXIS2_PLACEMENT_3D('',#30683,#12261,#12262);
#10583=AXIS2_PLACEMENT_3D('',#30684,#12263,#12264);
#10584=AXIS2_PLACEMENT_3D('',#30686,#12266,#12267);
#10585=AXIS2_PLACEMENT_3D('',#33776,#12269,#12270);
#10586=AXIS2_PLACEMENT_3D('',#33778,#12271,#12272);
#10587=AXIS2_PLACEMENT_3D('',#33780,#12274,#12275);
#10588=AXIS2_PLACEMENT_3D('',#33781,#12276,#12277);
#10589=AXIS2_PLACEMENT_3D('',#33782,#12278,#12279);
#10590=AXIS2_PLACEMENT_3D('',#34588,#12280,#12281);
#10591=AXIS2_PLACEMENT_3D('',#34589,#12282,#12283);
#10592=AXIS2_PLACEMENT_3D('',#34590,#12284,#12285);
#10593=AXIS2_PLACEMENT_3D('',#34592,#12286,#12287);
#10594=AXIS2_PLACEMENT_3D('',#34594,#12289,#12290);
#10595=AXIS2_PLACEMENT_3D('',#34595,#12291,#12292);
#10596=AXIS2_PLACEMENT_3D('',#34596,#12293,#12294);
#10597=AXIS2_PLACEMENT_3D('',#34597,#12295,#12296);
#10598=AXIS2_PLACEMENT_3D('',#34599,#12297,#12298);
#10599=AXIS2_PLACEMENT_3D('',#34607,#12299,#12300);
#10600=AXIS2_PLACEMENT_3D('',#34608,#12301,#12302);
#10601=AXIS2_PLACEMENT_3D('',#34636,#12303,#12304);
#10602=AXIS2_PLACEMENT_3D('',#34677,#12305,#12306);
#10603=AXIS2_PLACEMENT_3D('',#34678,#12307,#12308);
#10604=AXIS2_PLACEMENT_3D('',#34726,#12309,#12310);
#10605=AXIS2_PLACEMENT_3D('',#34763,#12311,#12312);
#10606=AXIS2_PLACEMENT_3D('',#34764,#12313,#12314);
#10607=AXIS2_PLACEMENT_3D('',#34765,#12315,#12316);
#10608=AXIS2_PLACEMENT_3D('',#34766,#12317,#12318);
#10609=AXIS2_PLACEMENT_3D('',#34768,#12319,#12320);
#10610=AXIS2_PLACEMENT_3D('',#34772,#12322,#12323);
#10611=AXIS2_PLACEMENT_3D('',#34773,#12324,#12325);
#10612=AXIS2_PLACEMENT_3D('',#34774,#12326,#12327);
#10613=AXIS2_PLACEMENT_3D('',#34776,#12328,#12329);
#10614=AXIS2_PLACEMENT_3D('',#34778,#12330,#12331);
#10615=AXIS2_PLACEMENT_3D('',#34779,#12332,#12333);
#10616=AXIS2_PLACEMENT_3D('',#34780,#12334,#12335);
#10617=AXIS2_PLACEMENT_3D('',#34783,#12337,#12338);
#10618=AXIS2_PLACEMENT_3D('',#34784,#12339,#12340);
#10619=AXIS2_PLACEMENT_3D('',#34785,#12341,#12342);
#10620=AXIS2_PLACEMENT_3D('',#34786,#12343,#12344);
#10621=AXIS2_PLACEMENT_3D('',#34787,#12345,#12346);
#10622=AXIS2_PLACEMENT_3D('',#35273,#12347,#12348);
#10623=AXIS2_PLACEMENT_3D('',#35275,#12349,#12350);
#10624=AXIS2_PLACEMENT_3D('',#35785,#12351,#12352);
#10625=AXIS2_PLACEMENT_3D('',#35835,#12353,#12354);
#10626=AXIS2_PLACEMENT_3D('',#37329,#12355,#12356);
#10627=AXIS2_PLACEMENT_3D('',#37854,#12357,#12358);
#10628=AXIS2_PLACEMENT_3D('',#38209,#12359,#12360);
#10629=AXIS2_PLACEMENT_3D('',#38457,#12361,#12362);
#10630=AXIS2_PLACEMENT_3D('',#38459,#12363,#12364);
#10631=AXIS2_PLACEMENT_3D('',#38692,#12365,#12366);
#10632=AXIS2_PLACEMENT_3D('',#38742,#12367,#12368);
#10633=AXIS2_PLACEMENT_3D('',#38871,#12369,#12370);
#10634=AXIS2_PLACEMENT_3D('',#39110,#12371,#12372);
#10635=AXIS2_PLACEMENT_3D('',#39236,#12373,#12374);
#10636=AXIS2_PLACEMENT_3D('',#39238,#12375,#12376);
#10637=AXIS2_PLACEMENT_3D('',#39241,#12378,#12379);
#10638=AXIS2_PLACEMENT_3D('',#39242,#12380,#12381);
#10639=AXIS2_PLACEMENT_3D('',#39244,#12382,#12383);
#10640=AXIS2_PLACEMENT_3D('',#39246,#12385,#12386);
#10641=AXIS2_PLACEMENT_3D('',#39248,#12387,#12388);
#10642=AXIS2_PLACEMENT_3D('',#39249,#12389,#12390);
#10643=AXIS2_PLACEMENT_3D('',#39251,#12391,#12392);
#10644=AXIS2_PLACEMENT_3D('',#39254,#12394,#12395);
#10645=AXIS2_PLACEMENT_3D('',#39255,#12396,#12397);
#10646=AXIS2_PLACEMENT_3D('',#39257,#12398,#12399);
#10647=AXIS2_PLACEMENT_3D('',#39258,#12400,#12401);
#10648=AXIS2_PLACEMENT_3D('',#39261,#12403,#12404);
#10649=AXIS2_PLACEMENT_3D('',#39262,#12405,#12406);
#10650=AXIS2_PLACEMENT_3D('',#39264,#12408,#12409);
#10651=AXIS2_PLACEMENT_3D('',#39266,#12410,#12411);
#10652=AXIS2_PLACEMENT_3D('',#39268,#12413,#12414);
#10653=AXIS2_PLACEMENT_3D('',#39271,#12416,#12417);
#10654=AXIS2_PLACEMENT_3D('',#39272,#12418,#12419);
#10655=AXIS2_PLACEMENT_3D('',#39275,#12420,#12421);
#10656=AXIS2_PLACEMENT_3D('',#39359,#12422,#12423);
#10657=AXIS2_PLACEMENT_3D('',#40000,#12424,#12425);
#10658=AXIS2_PLACEMENT_3D('',#40003,#12427,#12428);
#10659=AXIS2_PLACEMENT_3D('',#40004,#12429,#12430);
#10660=AXIS2_PLACEMENT_3D('',#40234,#12431,#12432);
#10661=AXIS2_PLACEMENT_3D('',#40236,#12433,#12434);
#10662=AXIS2_PLACEMENT_3D('',#40283,#12435,#12436);
#10663=AXIS2_PLACEMENT_3D('',#40464,#12437,#12438);
#10664=AXIS2_PLACEMENT_3D('',#40466,#12439,#12440);
#10665=AXIS2_PLACEMENT_3D('',#40467,#12441,#12442);
#10666=AXIS2_PLACEMENT_3D('',#40469,#12444,#12445);
#10667=AXIS2_PLACEMENT_3D('',#40471,#12446,#12447);
#10668=AXIS2_PLACEMENT_3D('',#40472,#12448,#12449);
#10669=AXIS2_PLACEMENT_3D('',#40474,#12451,#12452);
#10670=AXIS2_PLACEMENT_3D('',#40475,#12453,#12454);
#10671=AXIS2_PLACEMENT_3D('',#40477,#12455,#12456);
#10672=AXIS2_PLACEMENT_3D('',#40480,#12458,#12459);
#10673=AXIS2_PLACEMENT_3D('',#40481,#12460,#12461);
#10674=AXIS2_PLACEMENT_3D('',#40483,#12462,#12463);
#10675=AXIS2_PLACEMENT_3D('',#40485,#12465,#12466);
#10676=AXIS2_PLACEMENT_3D('',#40486,#12467,#12468);
#10677=AXIS2_PLACEMENT_3D('',#40489,#12470,#12471);
#10678=AXIS2_PLACEMENT_3D('',#40490,#12472,#12473);
#10679=AXIS2_PLACEMENT_3D('',#40491,#12474,#12475);
#10680=AXIS2_PLACEMENT_3D('',#40492,#12476,#12477);
#10681=AXIS2_PLACEMENT_3D('',#40548,#12479,#12480);
#10682=AXIS2_PLACEMENT_3D('',#40579,#12481,#12482);
#10683=AXIS2_PLACEMENT_3D('',#40902,#12484,#12485);
#10684=AXIS2_PLACEMENT_3D('',#41220,#12487,#12488);
#10685=AXIS2_PLACEMENT_3D('',#41540,#12490,#12491);
#10686=AXIS2_PLACEMENT_3D('',#41858,#12493,#12494);
#10687=AXIS2_PLACEMENT_3D('',#41893,#12496,#12497);
#10688=AXIS2_PLACEMENT_3D('',#42023,#12499,#12500);
#10689=AXIS2_PLACEMENT_3D('',#42104,#12501,#12502);
#10690=AXIS2_PLACEMENT_3D('',#42135,#12503,#12504);
#10691=AXIS2_PLACEMENT_3D('',#42454,#12505,#12506);
#10692=AXIS2_PLACEMENT_3D('',#43028,#12507,#12508);
#10693=AXIS2_PLACEMENT_3D('',#43345,#12509,#12510);
#10694=AXIS2_PLACEMENT_3D('',#43609,#12511,#12512);
#10695=AXIS2_PLACEMENT_3D('',#43610,#12513,#12514);
#10696=AXIS2_PLACEMENT_3D('',#43635,#12527,#12528);
#10697=AXIS2_PLACEMENT_3D('',#43638,#12530,#12531);
#10698=AXIS2_PLACEMENT_3D('',#43639,#12532,#12533);
#10699=AXIS2_PLACEMENT_3D('',#43645,#12537,#12538);
#10700=AXIS2_PLACEMENT_3D('',#43658,#12545,#12546);
#10701=AXIS2_PLACEMENT_3D('',#43659,#12547,#12548);
#10702=AXIS2_PLACEMENT_3D('',#43665,#12552,#12553);
#10703=AXIS2_PLACEMENT_3D('',#43678,#12560,#12561);
#10704=AXIS2_PLACEMENT_3D('',#43679,#12562,#12563);
#10705=AXIS2_PLACEMENT_3D('',#43683,#12566,#12567);
#10706=AXIS2_PLACEMENT_3D('',#43689,#12571,#12572);
#10707=AXIS2_PLACEMENT_3D('',#43701,#12579,#12580);
#10708=AXIS2_PLACEMENT_3D('',#43705,#12583,#12584);
#10709=AXIS2_PLACEMENT_3D('',#43709,#12587,#12588);
#10710=AXIS2_PLACEMENT_3D('',#43715,#12592,#12593);
#10711=AXIS2_PLACEMENT_3D('',#43730,#12602,#12603);
#10712=AXIS2_PLACEMENT_3D('',#43731,#12604,#12605);
#10713=AXIS2_PLACEMENT_3D('',#43735,#12608,#12609);
#10714=AXIS2_PLACEMENT_3D('',#43739,#12612,#12613);
#10715=AXIS2_PLACEMENT_3D('',#43743,#12616,#12617);
#10716=AXIS2_PLACEMENT_3D('',#43747,#12620,#12621);
#10717=AXIS2_PLACEMENT_3D('',#43753,#12625,#12626);
#10718=AXIS2_PLACEMENT_3D('',#43754,#12627,#12628);
#10719=AXIS2_PLACEMENT_3D('',#43755,#12629,#12630);
#10720=AXIS2_PLACEMENT_3D('',#43757,#12632,#12633);
#10721=AXIS2_PLACEMENT_3D('',#43759,#12635,#12636);
#10722=AXIS2_PLACEMENT_3D('',#43760,#12637,#12638);
#10723=AXIS2_PLACEMENT_3D('',#43762,#12640,#12641);
#10724=AXIS2_PLACEMENT_3D('',#43764,#12643,#12644);
#10725=AXIS2_PLACEMENT_3D('',#43765,#12645,#12646);
#10726=AXIS2_PLACEMENT_3D('',#43767,#12648,#12649);
#10727=AXIS2_PLACEMENT_3D('',#43845,#12650,#12651);
#10728=AXIS2_PLACEMENT_3D('',#43848,#12653,#12654);
#10729=AXIS2_PLACEMENT_3D('',#43851,#12656,#12657);
#10730=AXIS2_PLACEMENT_3D('',#43854,#12659,#12660);
#10731=AXIS2_PLACEMENT_3D('',#43856,#12661,#12662);
#10732=AXIS2_PLACEMENT_3D('',#43860,#12664,#12665);
#10733=AXIS2_PLACEMENT_3D('',#43861,#12666,#12667);
#10734=AXIS2_PLACEMENT_3D('',#43862,#12668,#12669);
#10735=AXIS2_PLACEMENT_3D('',#43864,#12670,#12671);
#10736=AXIS2_PLACEMENT_3D('',#43866,#12673,#12674);
#10737=AXIS2_PLACEMENT_3D('',#43868,#12675,#12676);
#10738=AXIS2_PLACEMENT_3D('',#43871,#12678,#12679);
#10739=AXIS2_PLACEMENT_3D('',#43872,#12680,#12681);
#10740=AXIS2_PLACEMENT_3D('',#43874,#12682,#12683);
#10741=AXIS2_PLACEMENT_3D('',#43875,#12684,#12685);
#10742=AXIS2_PLACEMENT_3D('',#43877,#12687,#12688);
#10743=AXIS2_PLACEMENT_3D('',#43880,#12689,#12690);
#10744=AXIS2_PLACEMENT_3D('',#43882,#12692,#12693);
#10745=AXIS2_PLACEMENT_3D('',#43889,#12694,#12695);
#10746=AXIS2_PLACEMENT_3D('',#44208,#12696,#12697);
#10747=AXIS2_PLACEMENT_3D('',#44426,#12698,#12699);
#10748=AXIS2_PLACEMENT_3D('',#44427,#12700,#12701);
#10749=AXIS2_PLACEMENT_3D('',#44480,#12702,#12703);
#10750=AXIS2_PLACEMENT_3D('',#44481,#12704,#12705);
#10751=AXIS2_PLACEMENT_3D('',#44526,#12706,#12707);
#10752=AXIS2_PLACEMENT_3D('',#44527,#12708,#12709);
#10753=AXIS2_PLACEMENT_3D('',#44572,#12710,#12711);
#10754=AXIS2_PLACEMENT_3D('',#44573,#12712,#12713);
#10755=AXIS2_PLACEMENT_3D('',#44618,#12714,#12715);
#10756=AXIS2_PLACEMENT_3D('',#44619,#12716,#12717);
#10757=AXIS2_PLACEMENT_3D('',#44664,#12718,#12719);
#10758=AXIS2_PLACEMENT_3D('',#44665,#12720,#12721);
#10759=AXIS2_PLACEMENT_3D('',#44718,#12722,#12723);
#10760=AXIS2_PLACEMENT_3D('',#44719,#12724,#12725);
#10761=AXIS2_PLACEMENT_3D('',#44764,#12726,#12727);
#10762=AXIS2_PLACEMENT_3D('',#44765,#12728,#12729);
#10763=AXIS2_PLACEMENT_3D('',#44810,#12730,#12731);
#10764=AXIS2_PLACEMENT_3D('',#44811,#12732,#12733);
#10765=AXIS2_PLACEMENT_3D('',#44856,#12734,#12735);
#10766=AXIS2_PLACEMENT_3D('',#44857,#12736,#12737);
#10767=AXIS2_PLACEMENT_3D('',#44902,#12738,#12739);
#10768=AXIS2_PLACEMENT_3D('',#44903,#12740,#12741);
#10769=AXIS2_PLACEMENT_3D('',#44956,#12742,#12743);
#10770=AXIS2_PLACEMENT_3D('',#44957,#12744,#12745);
#10771=AXIS2_PLACEMENT_3D('',#45002,#12746,#12747);
#10772=AXIS2_PLACEMENT_3D('',#45003,#12748,#12749);
#10773=AXIS2_PLACEMENT_3D('',#45048,#12750,#12751);
#10774=AXIS2_PLACEMENT_3D('',#45049,#12752,#12753);
#10775=AXIS2_PLACEMENT_3D('',#45094,#12754,#12755);
#10776=AXIS2_PLACEMENT_3D('',#45095,#12756,#12757);
#10777=AXIS2_PLACEMENT_3D('',#45140,#12758,#12759);
#10778=AXIS2_PLACEMENT_3D('',#45141,#12760,#12761);
#10779=AXIS2_PLACEMENT_3D('',#45194,#12762,#12763);
#10780=AXIS2_PLACEMENT_3D('',#45195,#12764,#12765);
#10781=AXIS2_PLACEMENT_3D('',#45240,#12766,#12767);
#10782=AXIS2_PLACEMENT_3D('',#45241,#12768,#12769);
#10783=AXIS2_PLACEMENT_3D('',#45286,#12770,#12771);
#10784=AXIS2_PLACEMENT_3D('',#45287,#12772,#12773);
#10785=AXIS2_PLACEMENT_3D('',#45332,#12774,#12775);
#10786=AXIS2_PLACEMENT_3D('',#45333,#12776,#12777);
#10787=AXIS2_PLACEMENT_3D('',#45378,#12778,#12779);
#10788=AXIS2_PLACEMENT_3D('',#45379,#12780,#12781);
#10789=AXIS2_PLACEMENT_3D('',#45417,#12782,#12783);
#10790=AXIS2_PLACEMENT_3D('',#45418,#12784,#12785);
#10791=AXIS2_PLACEMENT_3D('',#45419,#12786,#12787);
#10792=AXIS2_PLACEMENT_3D('',#45422,#12788,#12789);
#10793=AXIS2_PLACEMENT_3D('',#45462,#12792,#12793);
#10794=AXIS2_PLACEMENT_3D('',#45463,#12794,#12795);
#10795=AXIS2_PLACEMENT_3D('',#45464,#12796,#12797);
#10796=AXIS2_PLACEMENT_3D('',#45467,#12798,#12799);
#10797=AXIS2_PLACEMENT_3D('',#45470,#12802,#12803);
#10798=AXIS2_PLACEMENT_3D('',#45510,#12806,#12807);
#10799=AXIS2_PLACEMENT_3D('',#45511,#12808,#12809);
#10800=AXIS2_PLACEMENT_3D('',#45512,#12810,#12811);
#10801=AXIS2_PLACEMENT_3D('',#45515,#12812,#12813);
#10802=AXIS2_PLACEMENT_3D('',#45555,#12816,#12817);
#10803=AXIS2_PLACEMENT_3D('',#45556,#12818,#12819);
#10804=AXIS2_PLACEMENT_3D('',#45557,#12820,#12821);
#10805=AXIS2_PLACEMENT_3D('',#45560,#12822,#12823);
#10806=AXIS2_PLACEMENT_3D('',#45563,#12826,#12827);
#10807=AXIS2_PLACEMENT_3D('',#45566,#12830,#12831);
#10808=AXIS2_PLACEMENT_3D('',#45569,#12834,#12835);
#10809=AXIS2_PLACEMENT_3D('',#45572,#12838,#12839);
#10810=AXIS2_PLACEMENT_3D('',#45578,#12842,#12843);
#10811=AXIS2_PLACEMENT_3D('',#45586,#12847,#12848);
#10812=AXIS2_PLACEMENT_3D('',#45590,#12851,#12852);
#10813=AXIS2_PLACEMENT_3D('',#45600,#12858,#12859);
#10814=AXIS2_PLACEMENT_3D('',#45616,#12868,#12869);
#10815=AXIS2_PLACEMENT_3D('',#45626,#12875,#12876);
#10816=AXIS2_PLACEMENT_3D('',#45628,#12877,#12878);
#10817=AXIS2_PLACEMENT_3D('',#45630,#12879,#12880);
#10818=AXIS2_PLACEMENT_3D('',#45631,#12881,#12882);
#10819=AXIS2_PLACEMENT_3D('',#45634,#12883,#12884);
#10820=AXIS2_PLACEMENT_3D('',#45638,#12886,#12887);
#10821=AXIS2_PLACEMENT_3D('',#45640,#12889,#12890);
#10822=AXIS2_PLACEMENT_3D('',#45643,#12893,#12894);
#10823=AXIS2_PLACEMENT_3D('',#45649,#12898,#12899);
#10824=AXIS2_PLACEMENT_3D('',#45652,#12900,#12901);
#10825=AXIS2_PLACEMENT_3D('',#45656,#12903,#12904);
#10826=AXIS2_PLACEMENT_3D('',#45658,#12906,#12907);
#10827=AXIS2_PLACEMENT_3D('',#45661,#12910,#12911);
#10828=AXIS2_PLACEMENT_3D('',#45665,#12914,#12915);
#10829=AXIS2_PLACEMENT_3D('',#45668,#12916,#12917);
#10830=AXIS2_PLACEMENT_3D('',#45672,#12919,#12920);
#10831=AXIS2_PLACEMENT_3D('',#45674,#12922,#12923);
#10832=AXIS2_PLACEMENT_3D('',#45683,#12929,#12930);
#10833=AXIS2_PLACEMENT_3D('',#45685,#12932,#12933);
#10834=AXIS2_PLACEMENT_3D('',#45688,#12934,#12935);
#10835=AXIS2_PLACEMENT_3D('',#45692,#12937,#12938);
#10836=AXIS2_PLACEMENT_3D('',#45694,#12940,#12941);
#10837=AXIS2_PLACEMENT_3D('',#45706,#12948,#12949);
#10838=AXIS2_PLACEMENT_3D('',#45710,#12952,#12953);
#10839=AXIS2_PLACEMENT_3D('',#45713,#12954,#12955);
#10840=AXIS2_PLACEMENT_3D('',#45717,#12957,#12958);
#10841=AXIS2_PLACEMENT_3D('',#45719,#12960,#12961);
#10842=AXIS2_PLACEMENT_3D('',#45725,#12965,#12966);
#10843=AXIS2_PLACEMENT_3D('',#45733,#12971,#12972);
#10844=AXIS2_PLACEMENT_3D('',#45739,#12976,#12977);
#10845=AXIS2_PLACEMENT_3D('',#45741,#12979,#12980);
#10846=AXIS2_PLACEMENT_3D('',#45745,#12983,#12984);
#10847=AXIS2_PLACEMENT_3D('',#45754,#12990,#12991);
#10848=AXIS2_PLACEMENT_3D('',#45761,#12996,#12997);
#10849=AXIS2_PLACEMENT_3D('',#45765,#13000,#13001);
#10850=AXIS2_PLACEMENT_3D('',#45767,#13003,#13004);
#10851=AXIS2_PLACEMENT_3D('',#45769,#13006,#13007);
#10852=AXIS2_PLACEMENT_3D('',#45773,#13010,#13011);
#10853=AXIS2_PLACEMENT_3D('',#45777,#13014,#13015);
#10854=AXIS2_PLACEMENT_3D('',#45781,#13018,#13019);
#10855=AXIS2_PLACEMENT_3D('',#45786,#13023,#13024);
#10856=AXIS2_PLACEMENT_3D('',#45788,#13026,#13027);
#10857=AXIS2_PLACEMENT_3D('',#45789,#13028,#13029);
#10858=AXIS2_PLACEMENT_3D('',#45793,#13032,#13033);
#10859=AXIS2_PLACEMENT_3D('',#45797,#13036,#13037);
#10860=AXIS2_PLACEMENT_3D('',#45799,#13038,#13039);
#10861=AXIS2_PLACEMENT_3D('',#45800,#13040,#13041);
#10862=AXIS2_PLACEMENT_3D('',#45801,#13042,#13043);
#10863=AXIS2_PLACEMENT_3D('',#45803,#13044,#13045);
#10864=AXIS2_PLACEMENT_3D('',#45806,#13047,#13048);
#10865=AXIS2_PLACEMENT_3D('',#45807,#13049,#13050);
#10866=AXIS2_PLACEMENT_3D('',#45808,#13051,#13052);
#10867=AXIS2_PLACEMENT_3D('',#45810,#13053,#13054);
#10868=AXIS2_PLACEMENT_3D('',#45820,#13060,#13061);
#10869=AXIS2_PLACEMENT_3D('',#45822,#13063,#13064);
#10870=AXIS2_PLACEMENT_3D('',#45825,#13067,#13068);
#10871=AXIS2_PLACEMENT_3D('',#45826,#13069,#13070);
#10872=AXIS2_PLACEMENT_3D('',#45830,#13072,#13073);
#10873=AXIS2_PLACEMENT_3D('',#45835,#13077,#13078);
#10874=AXIS2_PLACEMENT_3D('',#45836,#13079,#13080);
#10875=AXIS2_PLACEMENT_3D('',#45838,#13082,#13083);
#10876=AXIS2_PLACEMENT_3D('',#45839,#13084,#13085);
#10877=AXIS2_PLACEMENT_3D('',#45841,#13087,#13088);
#10878=AXIS2_PLACEMENT_3D('',#45843,#13090,#13091);
#10879=AXIS2_PLACEMENT_3D('',#45844,#13092,#13093);
#10880=AXIS2_PLACEMENT_3D('',#45846,#13095,#13096);
#10881=AXIS2_PLACEMENT_3D('',#45848,#13097,#13098);
#10882=AXIS2_PLACEMENT_3D('',#45850,#13099,#13100);
#10883=AXIS2_PLACEMENT_3D('',#45852,#13102,#13103);
#10884=AXIS2_PLACEMENT_3D('',#45855,#13106,#13107);
#10885=AXIS2_PLACEMENT_3D('',#45861,#13111,#13112);
#10886=AXIS2_PLACEMENT_3D('',#45863,#13113,#13114);
#10887=AXIS2_PLACEMENT_3D('',#45865,#13115,#13116);
#10888=AXIS2_PLACEMENT_3D('',#45867,#13118,#13119);
#10889=AXIS2_PLACEMENT_3D('',#45870,#13122,#13123);
#10890=AXIS2_PLACEMENT_3D('',#45871,#13124,#13125);
#10891=AXIS2_PLACEMENT_3D('',#45872,#13126,#13127);
#10892=AXIS2_PLACEMENT_3D('',#45873,#13128,#13129);
#10893=AXIS2_PLACEMENT_3D('',#45875,#13130,#13131);
#10894=AXIS2_PLACEMENT_3D('',#45878,#13133,#13134);
#10895=AXIS2_PLACEMENT_3D('',#45879,#13135,#13136);
#10896=AXIS2_PLACEMENT_3D('',#45881,#13137,#13138);
#10897=AXIS2_PLACEMENT_3D('',#45883,#13140,#13141);
#10898=AXIS2_PLACEMENT_3D('',#45884,#13142,#13143);
#10899=AXIS2_PLACEMENT_3D('',#45885,#13144,#13145);
#10900=AXIS2_PLACEMENT_3D('',#45886,#13146,#13147);
#10901=AXIS2_PLACEMENT_3D('',#45912,#13149,#13150);
#10902=AXIS2_PLACEMENT_3D('',#45929,#13151,#13152);
#10903=AXIS2_PLACEMENT_3D('',#46009,#13154,#13155);
#10904=AXIS2_PLACEMENT_3D('',#46085,#13157,#13158);
#10905=AXIS2_PLACEMENT_3D('',#46161,#13160,#13161);
#10906=AXIS2_PLACEMENT_3D('',#46237,#13163,#13164);
#10907=AXIS2_PLACEMENT_3D('',#46313,#13166,#13167);
#10908=AXIS2_PLACEMENT_3D('',#46389,#13169,#13170);
#10909=AXIS2_PLACEMENT_3D('',#46465,#13172,#13173);
#10910=AXIS2_PLACEMENT_3D('',#46545,#13175,#13176);
#10911=AXIS2_PLACEMENT_3D('',#46621,#13178,#13179);
#10912=AXIS2_PLACEMENT_3D('',#46697,#13181,#13182);
#10913=AXIS2_PLACEMENT_3D('',#46773,#13184,#13185);
#10914=AXIS2_PLACEMENT_3D('',#46849,#13187,#13188);
#10915=AXIS2_PLACEMENT_3D('',#46925,#13190,#13191);
#10916=AXIS2_PLACEMENT_3D('',#47003,#13193,#13194);
#10917=AXIS2_PLACEMENT_3D('',#47029,#13196,#13197);
#10918=AXIS2_PLACEMENT_3D('',#47048,#13198,#13199);
#10919=AXIS2_PLACEMENT_3D('',#47126,#13201,#13202);
#10920=AXIS2_PLACEMENT_3D('',#47202,#13204,#13205);
#10921=AXIS2_PLACEMENT_3D('',#47278,#13207,#13208);
#10922=AXIS2_PLACEMENT_3D('',#47354,#13210,#13211);
#10923=AXIS2_PLACEMENT_3D('',#47430,#13213,#13214);
#10924=AXIS2_PLACEMENT_3D('',#47508,#13216,#13217);
#10925=AXIS2_PLACEMENT_3D('',#47584,#13219,#13220);
#10926=AXIS2_PLACEMENT_3D('',#47662,#13222,#13223);
#10927=AXIS2_PLACEMENT_3D('',#47738,#13225,#13226);
#10928=AXIS2_PLACEMENT_3D('',#47814,#13228,#13229);
#10929=AXIS2_PLACEMENT_3D('',#47890,#13231,#13232);
#10930=AXIS2_PLACEMENT_3D('',#47966,#13234,#13235);
#10931=AXIS2_PLACEMENT_3D('',#48044,#13237,#13238);
#10932=AXIS2_PLACEMENT_3D('',#48120,#13240,#13241);
#10933=AXIS2_PLACEMENT_3D('',#48196,#13243,#13244);
#10934=AXIS2_PLACEMENT_3D('',#48219,#13245,#13246);
#10935=AXIS2_PLACEMENT_3D('',#48238,#13247,#13248);
#10936=AXIS2_PLACEMENT_3D('',#48273,#13249,#13250);
#10937=AXIS2_PLACEMENT_3D('',#48304,#13251,#13252);
#10938=AXIS2_PLACEMENT_3D('',#48310,#13253,#13254);
#10939=AXIS2_PLACEMENT_3D('',#48311,#13255,#13256);
#10940=AXIS2_PLACEMENT_3D('',#48313,#13257,#13258);
#10941=AXIS2_PLACEMENT_3D('',#48316,#13260,#13261);
#10942=AXIS2_PLACEMENT_3D('',#48317,#13262,#13263);
#10943=AXIS2_PLACEMENT_3D('',#48319,#13264,#13265);
#10944=AXIS2_PLACEMENT_3D('',#48320,#13266,#13267);
#10945=AXIS2_PLACEMENT_3D('',#48350,#13269,#13270);
#10946=AXIS2_PLACEMENT_3D('',#48379,#13271,#13272);
#10947=AXIS2_PLACEMENT_3D('',#49202,#13273,#13274);
#10948=AXIS2_PLACEMENT_3D('',#49205,#13275,#13276);
#10949=AXIS2_PLACEMENT_3D('',#49207,#13277,#13278);
#10950=AXIS2_PLACEMENT_3D('',#49208,#13279,#13280);
#10951=AXIS2_PLACEMENT_3D('',#49210,#13281,#13282);
#10952=AXIS2_PLACEMENT_3D('',#49211,#13283,#13284);
#10953=AXIS2_PLACEMENT_3D('',#49212,#13285,#13286);
#10954=AXIS2_PLACEMENT_3D('',#49213,#13287,#13288);
#10955=AXIS2_PLACEMENT_3D('',#49217,#13289,#13290);
#10956=AXIS2_PLACEMENT_3D('',#49221,#13291,#13292);
#10957=AXIS2_PLACEMENT_3D('',#49225,#13293,#13294);
#10958=AXIS2_PLACEMENT_3D('',#49229,#13295,#13296);
#10959=AXIS2_PLACEMENT_3D('',#49233,#13297,#13298);
#10960=AXIS2_PLACEMENT_3D('',#49246,#13305,#13306);
#10961=AXIS2_PLACEMENT_3D('',#49249,#13309,#13310);
#10962=AXIS2_PLACEMENT_3D('',#49251,#13312,#13313);
#10963=AXIS2_PLACEMENT_3D('',#49253,#13315,#13316);
#10964=AXIS2_PLACEMENT_3D('',#49255,#13318,#13319);
#10965=AXIS2_PLACEMENT_3D('',#49257,#13321,#13322);
#10966=AXIS2_PLACEMENT_3D('',#49258,#13323,#13324);
#10967=AXIS2_PLACEMENT_3D('',#49259,#13325,#13326);
#10968=AXIS2_PLACEMENT_3D('',#49261,#13327,#13328);
#10969=AXIS2_PLACEMENT_3D('',#49262,#13329,#13330);
#10970=AXIS2_PLACEMENT_3D('',#49264,#13331,#13332);
#10971=AXIS2_PLACEMENT_3D('',#49268,#13334,#13335);
#10972=AXIS2_PLACEMENT_3D('',#49269,#13336,#13337);
#10973=AXIS2_PLACEMENT_3D('',#49270,#13338,#13339);
#10974=AXIS2_PLACEMENT_3D('',#49272,#13340,#13341);
#10975=AXIS2_PLACEMENT_3D('',#49274,#13342,#13343);
#10976=AXIS2_PLACEMENT_3D('',#49275,#13344,#13345);
#10977=AXIS2_PLACEMENT_3D('',#49276,#13346,#13347);
#10978=AXIS2_PLACEMENT_3D('',#49278,#13349,#13350);
#10979=AXIS2_PLACEMENT_3D('',#49279,#13351,#13352);
#10980=AXIS2_PLACEMENT_3D('',#49280,#13353,#13354);
#10981=AXIS2_PLACEMENT_3D('',#49282,#13355,#13356);
#10982=AXIS2_PLACEMENT_3D('',#49286,#13358,#13359);
#10983=AXIS2_PLACEMENT_3D('',#49287,#13360,#13361);
#10984=AXIS2_PLACEMENT_3D('',#49288,#13362,#13363);
#10985=AXIS2_PLACEMENT_3D('',#49290,#13364,#13365);
#10986=AXIS2_PLACEMENT_3D('',#49292,#13366,#13367);
#10987=AXIS2_PLACEMENT_3D('',#49293,#13368,#13369);
#10988=AXIS2_PLACEMENT_3D('',#49294,#13370,#13371);
#10989=AXIS2_PLACEMENT_3D('',#49297,#13373,#13374);
#10990=AXIS2_PLACEMENT_3D('',#49298,#13375,#13376);
#10991=AXIS2_PLACEMENT_3D('',#49299,#13377,#13378);
#10992=AXIS2_PLACEMENT_3D('',#49300,#13379,#13380);
#10993=AXIS2_PLACEMENT_3D('',#49301,#13381,#13382);
#10994=AXIS2_PLACEMENT_3D('',#49332,#13384,#13385);
#10995=AXIS2_PLACEMENT_3D('',#49340,#13386,#13387);
#10996=AXIS2_PLACEMENT_3D('',#49391,#13389,#13390);
#10997=AXIS2_PLACEMENT_3D('',#49416,#13391,#13392);
#10998=AXIS2_PLACEMENT_3D('',#49461,#13393,#13394);
#10999=AXIS2_PLACEMENT_3D('',#49492,#13395,#13396);
#11000=AXIS2_PLACEMENT_3D('',#49591,#13397,#13398);
#11001=AXIS2_PLACEMENT_3D('',#49603,#13399,#13400);
#11002=AXIS2_PLACEMENT_3D('',#49605,#13401,#13402);
#11003=AXIS2_PLACEMENT_3D('',#49608,#13404,#13405);
#11004=AXIS2_PLACEMENT_3D('',#49609,#13406,#13407);
#11005=AXIS2_PLACEMENT_3D('',#49612,#13409,#13410);
#11006=AXIS2_PLACEMENT_3D('',#49613,#13411,#13412);
#11007=AXIS2_PLACEMENT_3D('',#49779,#13413,#13414);
#11008=AXIS2_PLACEMENT_3D('',#49782,#13416,#13417);
#11009=AXIS2_PLACEMENT_3D('',#49783,#13418,#13419);
#11010=AXIS2_PLACEMENT_3D('',#49785,#13420,#13421);
#11011=AXIS2_PLACEMENT_3D('',#49786,#13422,#13423);
#11012=AXIS2_PLACEMENT_3D('',#49789,#13424,#13425);
#11013=AXIS2_PLACEMENT_3D('',#49897,#13426,#13427);
#11014=AXIS2_PLACEMENT_3D('',#50016,#13428,#13429);
#11015=AXIS2_PLACEMENT_3D('',#50018,#13431,#13432);
#11016=AXIS2_PLACEMENT_3D('',#50019,#13433,#13434);
#11017=AXIS2_PLACEMENT_3D('',#50020,#13435,#13436);
#11018=AXIS2_PLACEMENT_3D('',#50021,#13437,#13438);
#11019=AXIS2_PLACEMENT_3D('',#50022,#13439,#13440);
#11020=AXIS2_PLACEMENT_3D('',#50023,#13441,#13442);
#11021=AXIS2_PLACEMENT_3D('',#50024,#13443,#13444);
#11022=AXIS2_PLACEMENT_3D('',#50025,#13445,#13446);
#11023=AXIS2_PLACEMENT_3D('',#50026,#13447,#13448);
#11024=AXIS2_PLACEMENT_3D('',#50027,#13449,#13450);
#11025=AXIS2_PLACEMENT_3D('',#50028,#13451,#13452);
#11026=AXIS2_PLACEMENT_3D('',#50029,#13453,#13454);
#11027=AXIS2_PLACEMENT_3D('',#50030,#13455,#13456);
#11028=AXIS2_PLACEMENT_3D('',#50031,#13457,#13458);
#11029=AXIS2_PLACEMENT_3D('',#50032,#13459,#13460);
#11030=AXIS2_PLACEMENT_3D('',#50033,#13461,#13462);
#11031=AXIS2_PLACEMENT_3D('',#50034,#13463,#13464);
#11032=AXIS2_PLACEMENT_3D('',#50035,#13465,#13466);
#11033=AXIS2_PLACEMENT_3D('',#50036,#13467,#13468);
#11034=AXIS2_PLACEMENT_3D('',#50037,#13469,#13470);
#11035=DIRECTION('axis',(0.,0.,1.));
#11036=DIRECTION('refdir',(1.,0.,0.));
#11037=DIRECTION('axis',(0.,0.,1.));
#11038=DIRECTION('refdir',(1.,0.,0.));
#11039=DIRECTION('center_axis',(-2.42833204006769E-16,-2.41473507855972E-15,
1.));
#11040=DIRECTION('ref_axis',(-0.422618261740706,-0.906307787036647,-2.29111895189949E-15));
#11041=DIRECTION('center_axis',(-2.42833204006769E-16,-2.41473507855972E-15,
1.));
#11042=DIRECTION('ref_axis',(-0.422618261740706,-0.906307787036647,-2.29111895189949E-15));
#11043=DIRECTION('',(2.42833204006769E-16,2.41473507855972E-15,-1.));
#11044=DIRECTION('center_axis',(-2.42833204006769E-16,-2.41473507855972E-15,
1.));
#11045=DIRECTION('ref_axis',(-0.422618261740706,-0.906307787036647,-2.29111895189949E-15));
#11046=DIRECTION('center_axis',(-2.42833204006769E-16,-2.41473507855972E-15,
1.));
#11047=DIRECTION('ref_axis',(0.422618261740706,0.906307787036647,2.29111895189949E-15));
#11048=DIRECTION('center_axis',(-2.42833204006769E-16,-2.41473507855972E-15,
1.));
#11049=DIRECTION('ref_axis',(0.422618261740706,0.906307787036647,2.29111895189949E-15));
#11050=DIRECTION('axis',(0.,0.,1.));
#11051=DIRECTION('refdir',(1.,0.,0.));
#11052=DIRECTION('center_axis',(0.906307787036647,-0.422618261740706,-8.00429517722823E-16));
#11053=DIRECTION('ref_axis',(2.42833204006769E-16,2.41473507855972E-15,
-1.));
#11054=DIRECTION('center_axis',(0.906307787036647,-0.422618261740706,-8.00429517722823E-16));
#11055=DIRECTION('ref_axis',(0.422618261740706,0.906307787036647,1.97116866169388E-15));
#11056=DIRECTION('center_axis',(2.42833204006769E-16,2.41473507855972E-15,
-1.));
#11057=DIRECTION('ref_axis',(0.422618261740706,0.906307787036647,2.29111895189949E-15));
#11058=DIRECTION('center_axis',(2.41685059822166E-11,-1.12674314556115E-11,
-1.));
#11059=DIRECTION('ref_axis',(0.422618261740706,0.906307787036647,2.29111895186703E-15));
#11060=DIRECTION('',(-2.42833204006769E-16,-2.41473507855972E-15,1.));
#11061=DIRECTION('center_axis',(2.41685059822166E-11,-1.12674314556115E-11,
-1.));
#11062=DIRECTION('ref_axis',(0.422618261740706,0.906307787036647,2.29111895186703E-15));
#11063=DIRECTION('center_axis',(2.41685059822166E-11,-1.12674314556115E-11,
-1.));
#11064=DIRECTION('ref_axis',(0.422618261740706,0.906307787036647,2.29111895186703E-15));
#11065=DIRECTION('center_axis',(0.422618261740706,0.906307787036647,1.97116866169388E-15));
#11066=DIRECTION('ref_axis',(1.28498035257541E-16,2.05596856412066E-15,
-1.));
#11067=DIRECTION('center_axis',(-0.422618261740706,-0.906307787036647,-1.97116866169388E-15));
#11068=DIRECTION('ref_axis',(3.58767987664542E-16,2.00764771571504E-15,
-1.));
#11069=DIRECTION('center_axis',(0.906307787036647,-0.422618261740706,-8.00429517722823E-16));
#11070=DIRECTION('ref_axis',(0.422618261740706,0.906307787036647,1.97116866169388E-15));
#11071=DIRECTION('center_axis',(0.906307787036647,-0.422618261740706,-8.00429517722823E-16));
#11072=DIRECTION('ref_axis',(0.422618261740706,0.906307787036647,1.97116866169388E-15));
#11073=DIRECTION('center_axis',(0.906307787036647,-0.422618261740706,-8.00429517722823E-16));
#11074=DIRECTION('ref_axis',(0.422618261740706,0.906307787036647,1.97116866169388E-15));
#11075=DIRECTION('',(-0.906307787036647,0.422618261740706,8.00429517722823E-16));
#11076=DIRECTION('center_axis',(2.98328550528607E-16,2.38885717348462E-15,
-1.));
#11077=DIRECTION('ref_axis',(0.906307787036647,-0.422618261740706,-7.39197177765454E-16));
#11078=DIRECTION('axis',(0.,0.,1.));
#11079=DIRECTION('refdir',(1.,0.,0.));
#11080=DIRECTION('center_axis',(0.906307787036647,-0.422618261740706,-8.00429517722823E-16));
#11081=DIRECTION('ref_axis',(2.42833204006769E-16,2.41473507855972E-15,
-1.));
#11082=DIRECTION('center_axis',(0.906307787036647,-0.422618261740706,-8.00429517722823E-16));
#11083=DIRECTION('ref_axis',(0.422618261740706,0.906307787036647,1.97116866169388E-15));
#11084=DIRECTION('center_axis',(2.42833204006769E-16,2.41473507855972E-15,
-1.));
#11085=DIRECTION('ref_axis',(0.422618261740706,0.906307787036647,2.29111895189949E-15));
#11086=DIRECTION('center_axis',(2.41685059822166E-11,-1.12674314556115E-11,
-1.));
#11087=DIRECTION('ref_axis',(0.422618261740706,0.906307787036647,2.29111895186703E-15));
#11088=DIRECTION('',(-2.42833204006769E-16,-2.41473507855972E-15,1.));
#11089=DIRECTION('center_axis',(2.41685059822166E-11,-1.12674314556115E-11,
-1.));
#11090=DIRECTION('ref_axis',(0.422618261740706,0.906307787036647,2.29111895186703E-15));
#11091=DIRECTION('center_axis',(2.41685059822166E-11,-1.12674314556115E-11,
-1.));
#11092=DIRECTION('ref_axis',(0.422618261740706,0.906307787036647,2.29111895186703E-15));
#11093=DIRECTION('center_axis',(0.422618261740706,0.906307787036647,1.97116866169388E-15));
#11094=DIRECTION('ref_axis',(1.28498035257541E-16,2.05596856412066E-15,
-1.));
#11095=DIRECTION('center_axis',(-0.422618261740706,-0.906307787036647,-1.97116866169388E-15));
#11096=DIRECTION('ref_axis',(3.58767987664542E-16,2.00764771571504E-15,
-1.));
#11097=DIRECTION('center_axis',(0.906307787036647,-0.422618261740706,-8.00429517722823E-16));
#11098=DIRECTION('ref_axis',(0.422618261740706,0.906307787036647,1.97116866169388E-15));
#11099=DIRECTION('center_axis',(0.906307787036647,-0.422618261740706,-8.00429517722823E-16));
#11100=DIRECTION('ref_axis',(0.422618261740706,0.906307787036647,1.97116866169388E-15));
#11101=DIRECTION('center_axis',(0.906307787036647,-0.422618261740706,-8.00429517722823E-16));
#11102=DIRECTION('ref_axis',(0.422618261740706,0.906307787036647,1.97116866169388E-15));
#11103=DIRECTION('',(-0.906307787036647,0.422618261740706,8.00429517722823E-16));
#11104=DIRECTION('center_axis',(2.98328550528607E-16,2.38885717348462E-15,
-1.));
#11105=DIRECTION('ref_axis',(0.906307787036647,-0.422618261740706,-7.39197177765454E-16));
#11106=DIRECTION('axis',(0.,0.,1.));
#11107=DIRECTION('refdir',(1.,0.,0.));
#11108=DIRECTION('center_axis',(0.,1.,1.04083408558608E-15));
#11109=DIRECTION('ref_axis',(-1.,0.,0.));
#11110=DIRECTION('center_axis',(0.,-1.,-1.04083408558608E-15));
#11111=DIRECTION('ref_axis',(-0.387755102042543,-9.5940175792169E-16,0.921762431887944));
#11112=DIRECTION('center_axis',(0.,-1.04083408558608E-15,1.));
#11113=DIRECTION('ref_axis',(1.,0.,0.));
#11114=DIRECTION('center_axis',(0.,1.,1.04083408558608E-15));
#11115=DIRECTION('ref_axis',(-0.387755102042826,-9.59401757921566E-16,0.921762431887825));
#11116=DIRECTION('center_axis',(0.,-1.,-1.04083408558608E-15));
#11117=DIRECTION('ref_axis',(1.,0.,0.));
#11118=DIRECTION('center_axis',(0.,-1.,-1.04083408558608E-15));
#11119=DIRECTION('ref_axis',(1.,0.,0.));
#11120=DIRECTION('center_axis',(0.,-1.,-1.04083408558608E-15));
#11121=DIRECTION('ref_axis',(-1.,0.,0.));
#11122=DIRECTION('center_axis',(0.,-1.,-1.04083408558608E-15));
#11123=DIRECTION('ref_axis',(-1.,0.,0.));
#11124=DIRECTION('',(0.,-1.,-1.04083408558608E-15));
#11125=DIRECTION('center_axis',(0.,-1.,-1.04083408558608E-15));
#11126=DIRECTION('ref_axis',(-1.,0.,0.));
#11127=DIRECTION('',(0.,-1.,-1.04083408558608E-15));
#11128=DIRECTION('center_axis',(0.,-1.,-1.04083408558608E-15));
#11129=DIRECTION('ref_axis',(-1.,0.,0.));
#11130=DIRECTION('',(0.,-1.,-1.04083408558608E-15));
#11131=DIRECTION('center_axis',(0.,-1.,-1.04083408558608E-15));
#11132=DIRECTION('ref_axis',(-1.,0.,0.));
#11133=DIRECTION('',(0.,-1.,-1.04083408558608E-15));
#11134=DIRECTION('center_axis',(0.,-1.,-1.04083408558608E-15));
#11135=DIRECTION('ref_axis',(-1.,0.,0.));
#11136=DIRECTION('',(0.,-1.,-1.04083408558608E-15));
#11137=DIRECTION('center_axis',(0.,-1.,-1.04083408558608E-15));
#11138=DIRECTION('ref_axis',(-1.,0.,0.));
#11139=DIRECTION('',(0.,-1.,-1.04083408558608E-15));
#11140=DIRECTION('center_axis',(0.,-1.,-1.04083408558608E-15));
#11141=DIRECTION('ref_axis',(-1.,0.,0.));
#11142=DIRECTION('',(0.,-1.,-1.04083408558608E-15));
#11143=DIRECTION('center_axis',(0.,-1.,-1.04083408558608E-15));
#11144=DIRECTION('ref_axis',(-1.,0.,0.));
#11145=DIRECTION('',(0.,-1.,-1.04083408558608E-15));
#11146=DIRECTION('center_axis',(0.,-1.,-1.04083408558608E-15));
#11147=DIRECTION('ref_axis',(-1.,0.,0.));
#11148=DIRECTION('',(0.,1.,1.04083408558608E-15));
#11149=DIRECTION('center_axis',(0.,1.,1.04083408558608E-15));
#11150=DIRECTION('ref_axis',(-1.,0.,0.));
#11151=DIRECTION('center_axis',(0.,-1.,-1.04083408558608E-15));
#11152=DIRECTION('ref_axis',(1.,0.,0.));
#11153=DIRECTION('center_axis',(0.,1.04083408558608E-15,-1.));
#11154=DIRECTION('ref_axis',(1.,0.,0.));
#11155=DIRECTION('center_axis',(0.,1.,1.04083408558608E-15));
#11156=DIRECTION('ref_axis',(1.,0.,0.));
#11157=DIRECTION('center_axis',(0.,-1.,-1.04083408558608E-15));
#11158=DIRECTION('ref_axis',(-1.,0.,0.));
#11159=DIRECTION('',(0.,-1.,-1.04083408558608E-15));
#11160=DIRECTION('center_axis',(0.,1.,1.04083408558608E-15));
#11161=DIRECTION('ref_axis',(-1.,0.,0.));
#11162=DIRECTION('center_axis',(0.,0.083045479854119,-0.996545758244848));
#11163=DIRECTION('ref_axis',(0.,-0.996545758244848,-0.083045479854119));
#11164=DIRECTION('',(0.,-1.,-1.04083408558608E-15));
#11165=DIRECTION('center_axis',(0.,-0.196116135138937,-0.98058067569077));
#11166=DIRECTION('ref_axis',(0.,0.98058067569077,-0.196116135138937));
#11167=DIRECTION('',(0.,-1.,-1.04083408558608E-15));
#11168=DIRECTION('center_axis',(0.,1.,1.04083408558608E-15));
#11169=DIRECTION('ref_axis',(-1.,0.,0.));
#11170=DIRECTION('',(0.,-1.,-1.04083408558608E-15));
#11171=DIRECTION('center_axis',(-0.980580675690769,-0.196116135138938,-2.04124358186013E-16));
#11172=DIRECTION('ref_axis',(-0.196116135138938,0.980580675690769,1.02062179092598E-15));
#11173=DIRECTION('',(0.,-1.,-1.04083408558608E-15));
#11174=DIRECTION('center_axis',(-0.996545758244848,0.083045479854118,8.64365660860182E-17));
#11175=DIRECTION('ref_axis',(-0.083045479854118,-0.996545758244848,-1.03723879302746E-15));
#11176=DIRECTION('center_axis',(0.,1.,1.04083408558608E-15));
#11177=DIRECTION('ref_axis',(-1.,0.,0.));
#11178=DIRECTION('center_axis',(0.996545758244848,0.083045479854118,8.64365660860182E-17));
#11179=DIRECTION('ref_axis',(-0.083045479854118,0.996545758244848,1.03723879302746E-15));
#11180=DIRECTION('',(0.,-1.,-1.04083408558608E-15));
#11181=DIRECTION('center_axis',(0.980580675690769,-0.196116135138938,-2.04124358186013E-16));
#11182=DIRECTION('ref_axis',(-0.196116135138938,-0.980580675690769,-1.02062179092598E-15));
#11183=DIRECTION('',(0.,-1.,-1.04083408558608E-15));
#11184=DIRECTION('center_axis',(0.,1.,1.04083408558608E-15));
#11185=DIRECTION('ref_axis',(-1.,0.,0.));
#11186=DIRECTION('',(0.,-1.,-1.04083408558608E-15));
#11187=DIRECTION('center_axis',(0.,-0.196116135138937,-0.98058067569077));
#11188=DIRECTION('ref_axis',(0.,0.98058067569077,-0.196116135138937));
#11189=DIRECTION('',(0.,-1.,-1.04083408558608E-15));
#11190=DIRECTION('center_axis',(0.,0.083045479854119,-0.996545758244848));
#11191=DIRECTION('ref_axis',(0.,-0.996545758244848,-0.083045479854119));
#11192=DIRECTION('center_axis',(0.,1.,1.04083408558608E-15));
#11193=DIRECTION('ref_axis',(-1.,0.,0.));
#11194=DIRECTION('center_axis',(0.,0.083045479854117,0.996545758244848));
#11195=DIRECTION('ref_axis',(0.,0.996545758244848,-0.083045479854117));
#11196=DIRECTION('',(0.,-1.,-1.04083408558608E-15));
#11197=DIRECTION('center_axis',(0.,-0.196116135138939,0.980580675690769));
#11198=DIRECTION('ref_axis',(0.,-0.980580675690769,-0.196116135138939));
#11199=DIRECTION('',(0.,-1.,-1.04083408558608E-15));
#11200=DIRECTION('center_axis',(0.,1.,1.04083408558608E-15));
#11201=DIRECTION('ref_axis',(-1.,0.,0.));
#11202=DIRECTION('',(0.,-1.,-1.04083408558608E-15));
#11203=DIRECTION('center_axis',(0.980580675690769,-0.196116135138938,-2.04124358186013E-16));
#11204=DIRECTION('ref_axis',(-0.196116135138938,-0.980580675690769,-1.02062179092598E-15));
#11205=DIRECTION('',(0.,-1.,-1.04083408558608E-15));
#11206=DIRECTION('center_axis',(0.996545758244848,0.083045479854118,8.64365660860182E-17));
#11207=DIRECTION('ref_axis',(-0.083045479854118,0.996545758244848,1.03723879302746E-15));
#11208=DIRECTION('center_axis',(0.,1.,1.04083408558608E-15));
#11209=DIRECTION('ref_axis',(-1.,0.,0.));
#11210=DIRECTION('center_axis',(-0.996545758244848,0.083045479854118,8.64365660860182E-17));
#11211=DIRECTION('ref_axis',(-0.083045479854118,-0.996545758244848,-1.03723879302746E-15));
#11212=DIRECTION('',(0.,-1.,-1.04083408558608E-15));
#11213=DIRECTION('center_axis',(-0.980580675690769,-0.196116135138938,-2.04124358186013E-16));
#11214=DIRECTION('ref_axis',(-0.196116135138938,0.980580675690769,1.02062179092598E-15));
#11215=DIRECTION('',(0.,-1.,-1.04083408558608E-15));
#11216=DIRECTION('center_axis',(0.,1.,1.04083408558608E-15));
#11217=DIRECTION('ref_axis',(-1.,0.,0.));
#11218=DIRECTION('',(0.,-1.,-1.04083408558608E-15));
#11219=DIRECTION('center_axis',(0.,-0.196116135138939,0.980580675690769));
#11220=DIRECTION('ref_axis',(0.,-0.980580675690769,-0.196116135138939));
#11221=DIRECTION('',(0.,-1.,-1.04083408558608E-15));
#11222=DIRECTION('center_axis',(0.,0.083045479854117,0.996545758244848));
#11223=DIRECTION('ref_axis',(0.,0.996545758244848,-0.083045479854117));
#11224=DIRECTION('center_axis',(0.,1.,1.04083408558608E-15));
#11225=DIRECTION('ref_axis',(-1.,0.,0.));
#11226=DIRECTION('center_axis',(0.,-1.,-1.04083408558608E-15));
#11227=DIRECTION('ref_axis',(1.,0.,0.));
#11228=DIRECTION('center_axis',(0.,-1.,-1.04083408558608E-15));
#11229=DIRECTION('ref_axis',(1.,0.,0.));
#11230=DIRECTION('center_axis',(0.99654575824488,-0.08304547985374,-8.64365660856247E-17));
#11231=DIRECTION('ref_axis',(8.26770005765773E-33,1.04083408558608E-15,
-1.));
#11232=DIRECTION('',(0.,1.04083408558608E-15,-1.));
#11233=DIRECTION('',(0.,-1.04083408558608E-15,1.));
#11234=DIRECTION('center_axis',(0.,1.,1.04083408558608E-15));
#11235=DIRECTION('ref_axis',(-1.,0.,0.));
#11236=DIRECTION('center_axis',(0.,1.,1.04083408558608E-15));
#11237=DIRECTION('ref_axis',(-1.,0.,0.));
#11238=DIRECTION('center_axis',(0.,-1.,-1.04083408558608E-15));
#11239=DIRECTION('ref_axis',(-1.,0.,0.));
#11240=DIRECTION('center_axis',(0.,-1.,-1.04083408558608E-15));
#11241=DIRECTION('ref_axis',(1.,0.,0.));
#11242=DIRECTION('',(0.,-1.04083408558608E-15,1.));
#11243=DIRECTION('center_axis',(-0.99654575824488,-0.08304547985374,-8.64365660856247E-17));
#11244=DIRECTION('ref_axis',(8.26770005765773E-33,-1.04083408558608E-15,
1.));
#11245=DIRECTION('',(0.,1.04083408558608E-15,-1.));
#11246=DIRECTION('center_axis',(0.,-0.083045479853739,-0.99654575824488));
#11247=DIRECTION('ref_axis',(-1.,0.,0.));
#11248=DIRECTION('',(-1.,0.,0.));
#11249=DIRECTION('',(1.,0.,0.));
#11250=DIRECTION('center_axis',(0.,-1.,-1.04083408558608E-15));
#11251=DIRECTION('ref_axis',(1.,0.,0.));
#11252=DIRECTION('',(1.,0.,0.));
#11253=DIRECTION('center_axis',(0.,1.,1.04083408558608E-15));
#11254=DIRECTION('ref_axis',(-1.,0.,0.));
#11255=DIRECTION('center_axis',(0.,-0.083045479853739,-0.99654575824488));
#11256=DIRECTION('ref_axis',(-1.,0.,0.));
#11257=DIRECTION('',(-1.,0.,0.));
#11258=DIRECTION('',(1.,0.,0.));
#11259=DIRECTION('center_axis',(0.,-1.,-1.04083408558608E-15));
#11260=DIRECTION('ref_axis',(1.,0.,0.));
#11261=DIRECTION('center_axis',(0.,1.,1.04083408558608E-15));
#11262=DIRECTION('ref_axis',(1.,0.,0.));
#11263=DIRECTION('',(1.,0.,0.));
#11264=DIRECTION('center_axis',(0.,-0.083045479853741,0.99654575824488));
#11265=DIRECTION('ref_axis',(1.,0.,0.));
#11266=DIRECTION('',(-1.,0.,0.));
#11267=DIRECTION('center_axis',(0.99654575824488,-0.08304547985374,-8.64365660856247E-17));
#11268=DIRECTION('ref_axis',(8.26770005765773E-33,1.04083408558608E-15,
-1.));
#11269=DIRECTION('',(0.,1.04083408558608E-15,-1.));
#11270=DIRECTION('',(0.,-1.04083408558608E-15,1.));
#11271=DIRECTION('center_axis',(0.,-1.,-1.04083408558608E-15));
#11272=DIRECTION('ref_axis',(1.,0.,0.));
#11273=DIRECTION('center_axis',(0.,1.,1.04083408558608E-15));
#11274=DIRECTION('ref_axis',(-1.,0.,0.));
#11275=DIRECTION('',(0.,-1.04083408558608E-15,1.));
#11276=DIRECTION('center_axis',(0.,1.,1.04083408558608E-15));
#11277=DIRECTION('ref_axis',(-1.,0.,0.));
#11278=DIRECTION('center_axis',(0.,-1.,-1.04083408558608E-15));
#11279=DIRECTION('ref_axis',(-1.,0.,0.));
#11280=DIRECTION('center_axis',(0.,-0.083045479853741,0.99654575824488));
#11281=DIRECTION('ref_axis',(1.,0.,0.));
#11282=DIRECTION('',(-1.,0.,0.));
#11283=DIRECTION('center_axis',(0.,1.,1.04083408558608E-15));
#11284=DIRECTION('ref_axis',(-1.,0.,0.));
#11285=DIRECTION('center_axis',(0.,-1.,-1.04083408558608E-15));
#11286=DIRECTION('ref_axis',(-1.,0.,0.));
#11287=DIRECTION('center_axis',(-0.99654575824488,-0.08304547985374,-8.64365660856247E-17));
#11288=DIRECTION('ref_axis',(8.26770005765773E-33,-1.04083408558608E-15,
1.));
#11289=DIRECTION('',(0.,1.04083408558608E-15,-1.));
#11290=DIRECTION('center_axis',(-1.,0.,0.));
#11291=DIRECTION('ref_axis',(0.,-1.,-1.04083408558608E-15));
#11292=DIRECTION('',(0.,-1.,-1.04083408558608E-15));
#11293=DIRECTION('',(0.,-1.04083408558608E-15,1.));
#11294=DIRECTION('center_axis',(0.,0.196116135138185,-0.98058067569092));
#11295=DIRECTION('ref_axis',(0.,0.98058067569092,0.196116135138185));
#11296=DIRECTION('',(-1.,0.,0.));
#11297=DIRECTION('center_axis',(-2.93579933474955E-11,0.196116135154336,
-0.98058067568769));
#11298=DIRECTION('ref_axis',(-0.872297796013763,0.479479440345853,0.0958958881035005));
#11299=DIRECTION('',(1.,0.,0.));
#11300=DIRECTION('',(1.,0.,0.));
#11301=DIRECTION('center_axis',(0.,-1.,-1.04083408558608E-15));
#11302=DIRECTION('ref_axis',(1.,0.,0.));
#11303=DIRECTION('center_axis',(0.,-1.,-1.04083408558608E-15));
#11304=DIRECTION('ref_axis',(-1.,0.,0.));
#11305=DIRECTION('',(-1.,0.,0.));
#11306=DIRECTION('center_axis',(0.,-1.,-1.04083408558608E-15));
#11307=DIRECTION('ref_axis',(-1.,0.,0.));
#11308=DIRECTION('center_axis',(0.,1.,1.04083408558608E-15));
#11309=DIRECTION('ref_axis',(-1.,0.,0.));
#11310=DIRECTION('center_axis',(-2.93579933474955E-11,0.196116135154334,
0.98058067568769));
#11311=DIRECTION('ref_axis',(-0.871703578481421,0.480517420696057,-0.0961034841735403));
#11312=DIRECTION('center_axis',(-0.98058067569092,0.196116135138184,2.04124358185228E-16));
#11313=DIRECTION('ref_axis',(-0.196116135138184,-0.98058067569092,-1.02062179092614E-15));
#11314=DIRECTION('',(0.,-1.04083408558608E-15,1.));
#11315=DIRECTION('',(0.,1.04083408558608E-15,-1.));
#11316=DIRECTION('',(0.,1.04083408558608E-15,-1.));
#11317=DIRECTION('center_axis',(0.,-1.,-1.04083408558608E-15));
#11318=DIRECTION('ref_axis',(-1.,0.,0.));
#11319=DIRECTION('center_axis',(0.,-1.,-1.04083408558608E-15));
#11320=DIRECTION('ref_axis',(-1.,0.,0.));
#11321=DIRECTION('center_axis',(0.,1.,1.04083408558608E-15));
#11322=DIRECTION('ref_axis',(-1.,0.,0.));
#11323=DIRECTION('center_axis',(0.,-1.,-1.04083408558608E-15));
#11324=DIRECTION('ref_axis',(1.,0.,0.));
#11325=DIRECTION('',(0.,-1.04083408558608E-15,1.));
#11326=DIRECTION('center_axis',(0.98058067569092,0.196116135138184,2.04124358185228E-16));
#11327=DIRECTION('ref_axis',(1.87305315315727E-31,1.04083408558608E-15,
-1.));
#11328=DIRECTION('',(0.,1.04083408558608E-15,-1.));
#11329=DIRECTION('',(0.,-1.04083408558608E-15,1.));
#11330=DIRECTION('center_axis',(1.,0.,0.));
#11331=DIRECTION('ref_axis',(0.,-1.04083408558608E-15,1.));
#11332=DIRECTION('',(0.,-1.,-1.04083408558608E-15));
#11333=DIRECTION('center_axis',(0.,0.196116135138185,-0.98058067569092));
#11334=DIRECTION('ref_axis',(0.,0.98058067569092,0.196116135138185));
#11335=DIRECTION('center_axis',(2.93579933474955E-11,0.196116135154336,
-0.98058067568769));
#11336=DIRECTION('ref_axis',(0.871703578481421,0.480517420696057,0.0961034841735413));
#11337=DIRECTION('',(-1.,0.,0.));
#11338=DIRECTION('',(1.,0.,0.));
#11339=DIRECTION('',(1.,0.,0.));
#11340=DIRECTION('center_axis',(0.,-1.,-1.04083408558608E-15));
#11341=DIRECTION('ref_axis',(1.,0.,0.));
#11342=DIRECTION('center_axis',(0.,-1.,-1.04083408558608E-15));
#11343=DIRECTION('ref_axis',(1.,0.,0.));
#11344=DIRECTION('center_axis',(2.93579933474955E-11,0.196116135154334,
0.98058067568769));
#11345=DIRECTION('ref_axis',(0.872297796013763,0.479479440345853,-0.0958958881034995));
#11346=DIRECTION('center_axis',(0.,1.,1.04083408558608E-15));
#11347=DIRECTION('ref_axis',(1.,0.,0.));
#11348=DIRECTION('center_axis',(0.,-1.,-1.04083408558608E-15));
#11349=DIRECTION('ref_axis',(1.,0.,0.));
#11350=DIRECTION('',(-1.,0.,0.));
#11351=DIRECTION('center_axis',(0.,0.196116135138183,0.98058067569092));
#11352=DIRECTION('ref_axis',(-1.,0.,0.));
#11353=DIRECTION('',(1.,0.,0.));
#11354=DIRECTION('',(-1.,0.,0.));
#11355=DIRECTION('center_axis',(0.,-1.04083408558608E-15,1.));
#11356=DIRECTION('ref_axis',(1.,0.,0.));
#11357=DIRECTION('',(0.,-1.,-1.04083408558608E-15));
#11358=DIRECTION('center_axis',(0.98058067569092,0.196116135138184,2.04124358185228E-16));
#11359=DIRECTION('ref_axis',(1.87305315315727E-31,1.04083408558608E-15,
-1.));
#11360=DIRECTION('',(0.,1.04083408558608E-15,-1.));
#11361=DIRECTION('',(0.,-1.04083408558608E-15,1.));
#11362=DIRECTION('',(0.,-1.04083408558608E-15,1.));
#11363=DIRECTION('center_axis',(0.,-1.,-1.04083408558608E-15));
#11364=DIRECTION('ref_axis',(-1.,0.,0.));
#11365=DIRECTION('center_axis',(0.,-1.,-1.04083408558608E-15));
#11366=DIRECTION('ref_axis',(-1.,0.,0.));
#11367=DIRECTION('center_axis',(0.,1.,1.04083408558608E-15));
#11368=DIRECTION('ref_axis',(-1.,0.,0.));
#11369=DIRECTION('center_axis',(0.,-1.,-1.04083408558608E-15));
#11370=DIRECTION('ref_axis',(1.,0.,0.));
#11371=DIRECTION('',(0.,1.04083408558608E-15,-1.));
#11372=DIRECTION('center_axis',(0.,0.196116135138183,0.98058067569092));
#11373=DIRECTION('ref_axis',(-1.,0.,0.));
#11374=DIRECTION('',(1.,0.,0.));
#11375=DIRECTION('',(-1.,0.,0.));
#11376=DIRECTION('center_axis',(-0.98058067569092,0.196116135138184,2.04124358185228E-16));
#11377=DIRECTION('ref_axis',(-0.196116135138184,-0.98058067569092,-1.02062179092614E-15));
#11378=DIRECTION('',(0.,1.04083408558608E-15,-1.));
#11379=DIRECTION('center_axis',(-1.,0.,0.));
#11380=DIRECTION('ref_axis',(0.,-1.,-1.04083408558608E-15));
#11381=DIRECTION('',(0.,-1.04083408558608E-15,1.));
#11382=DIRECTION('center_axis',(1.,0.,0.));
#11383=DIRECTION('ref_axis',(0.,-1.04083408558608E-15,1.));
#11384=DIRECTION('',(0.,1.04083408558608E-15,-1.));
#11385=DIRECTION('center_axis',(0.,-1.04083408558608E-15,1.));
#11386=DIRECTION('ref_axis',(1.,0.,0.));
#11387=DIRECTION('',(1.,0.,0.));
#11388=DIRECTION('center_axis',(0.,1.04083408558608E-15,-1.));
#11389=DIRECTION('ref_axis',(0.,1.,1.04083408558608E-15));
#11390=DIRECTION('',(-1.,0.,0.));
#11391=DIRECTION('center_axis',(0.,1.04083408558608E-15,-1.));
#11392=DIRECTION('ref_axis',(0.,1.,1.04083408558608E-15));
#11393=DIRECTION('',(-1.,0.,0.));
#11394=DIRECTION('center_axis',(0.,-1.04083408558608E-15,1.));
#11395=DIRECTION('ref_axis',(1.,0.,0.));
#11396=DIRECTION('',(1.,0.,0.));
#11397=DIRECTION('center_axis',(1.,0.,0.));
#11398=DIRECTION('ref_axis',(0.,-1.04083408558608E-15,1.));
#11399=DIRECTION('',(0.,1.04083408558608E-15,-1.));
#11400=DIRECTION('center_axis',(-1.,0.,0.));
#11401=DIRECTION('ref_axis',(0.,-1.,-1.04083408558608E-15));
#11402=DIRECTION('',(0.,-1.04083408558608E-15,1.));
#11403=DIRECTION('center_axis',(0.,-1.,-1.04083408558608E-15));
#11404=DIRECTION('ref_axis',(1.,0.,0.));
#11405=DIRECTION('center_axis',(0.,-1.,-1.04083408558608E-15));
#11406=DIRECTION('ref_axis',(1.,0.,0.));
#11407=DIRECTION('center_axis',(0.,-1.,-1.04083408558608E-15));
#11408=DIRECTION('ref_axis',(1.,0.,0.));
#11409=DIRECTION('center_axis',(0.,-1.,-1.04083408558608E-15));
#11410=DIRECTION('ref_axis',(1.,0.,0.));
#11411=DIRECTION('center_axis',(0.,-1.,-1.04083408558608E-15));
#11412=DIRECTION('ref_axis',(1.,0.,0.));
#11413=DIRECTION('',(0.,1.,1.04083408558608E-15));
#11414=DIRECTION('center_axis',(0.,1.04083408558608E-15,-1.));
#11415=DIRECTION('ref_axis',(0.,1.,1.04083408558608E-15));
#11416=DIRECTION('',(0.,-1.,-1.04083408558608E-15));
#11417=DIRECTION('center_axis',(0.,-1.,-1.04083408558608E-15));
#11418=DIRECTION('ref_axis',(-1.,0.,0.));
#11419=DIRECTION('',(0.,-1.,-1.04083408558608E-15));
#11420=DIRECTION('center_axis',(0.,-1.04083408558608E-15,1.));
#11421=DIRECTION('ref_axis',(1.,0.,0.));
#11422=DIRECTION('center_axis',(0.,1.,1.04083408558608E-15));
#11423=DIRECTION('ref_axis',(1.,0.,0.));
#11424=DIRECTION('center_axis',(0.,-1.,-1.04083408558608E-15));
#11425=DIRECTION('ref_axis',(1.,0.,0.));
#11426=DIRECTION('center_axis',(0.,-1.,-1.04083408558608E-15));
#11427=DIRECTION('ref_axis',(1.,1.27465413135645E-31,-1.22464679914735E-16));
#11428=DIRECTION('',(0.,-1.,-1.04083408558608E-15));
#11429=DIRECTION('center_axis',(0.,1.04083408558608E-15,-1.));
#11430=DIRECTION('ref_axis',(0.,1.,1.04083408558608E-15));
#11431=DIRECTION('center_axis',(0.,-1.,-1.04083408558608E-15));
#11432=DIRECTION('ref_axis',(-1.,0.,0.));
#11433=DIRECTION('',(0.,-1.,-1.04083408558608E-15));
#11434=DIRECTION('center_axis',(1.,0.,0.));
#11435=DIRECTION('ref_axis',(0.,-1.04083408558608E-15,1.));
#11436=DIRECTION('center_axis',(0.,-1.,-1.04083408558608E-15));
#11437=DIRECTION('ref_axis',(-1.,0.,0.));
#11438=DIRECTION('',(0.,-1.,-1.04083408558608E-15));
#11439=DIRECTION('center_axis',(-1.,0.,0.));
#11440=DIRECTION('ref_axis',(0.,-1.,-1.04083408558608E-15));
#11441=DIRECTION('axis',(0.,0.,1.));
#11442=DIRECTION('refdir',(1.,0.,0.));
#11443=DIRECTION('center_axis',(-2.37714673961354E-29,1.,6.52256026967277E-16));
#11444=DIRECTION('ref_axis',(-1.,-9.36001528722827E-29,1.07057171707285E-13));
#11445=DIRECTION('center_axis',(-3.25361965184118E-12,-1.,3.25296739583608E-12));
#11446=DIRECTION('ref_axis',(-1.,3.25361965185211E-12,3.36067682355905E-12));
#11447=DIRECTION('center_axis',(3.25361965184118E-12,1.,-3.25296739583608E-12));
#11448=DIRECTION('ref_axis',(-1.,3.25361965185211E-12,3.36067682355905E-12));
#11449=DIRECTION('center_axis',(0.,1.,6.52256026967277E-16));
#11450=DIRECTION('ref_axis',(-1.,0.,0.));
#11451=DIRECTION('center_axis',(0.,-1.,3.9715423814945E-12));
#11452=DIRECTION('ref_axis',(-1.,0.,0.));
#11453=DIRECTION('center_axis',(0.,1.,-3.9715423814945E-12));
#11454=DIRECTION('ref_axis',(-1.,0.,0.));
#11455=DIRECTION('center_axis',(0.,1.,-3.9715423814945E-12));
#11456=DIRECTION('ref_axis',(-1.,0.,0.));
#11457=DIRECTION('center_axis',(0.,1.,1.09634523681734E-15));
#11458=DIRECTION('ref_axis',(-1.,0.,0.));
#11459=DIRECTION('center_axis',(0.,-1.,2.49912569936186E-12));
#11460=DIRECTION('ref_axis',(-1.,0.,0.));
#11461=DIRECTION('',(0.707106781186547,0.707106781186548,6.88637545851563E-16));
#11462=DIRECTION('center_axis',(0.,1.,-2.38007808031482E-12));
#11463=DIRECTION('ref_axis',(-1.,0.,0.));
#11464=DIRECTION('center_axis',(0.,-1.,-8.74300631892309E-16));
#11465=DIRECTION('ref_axis',(0.,-8.74300631892309E-16,1.));
#11466=DIRECTION('center_axis',(0.,-1.,1.28117698141774E-12));
#11467=DIRECTION('ref_axis',(1.,0.,0.));
#11468=DIRECTION('center_axis',(0.,-1.,-8.74300631892318E-16));
#11469=DIRECTION('ref_axis',(-1.,0.,0.));
#11470=DIRECTION('',(0.,-1.,-8.74300631892318E-16));
#11471=DIRECTION('center_axis',(0.,-1.,2.49912569936186E-12));
#11472=DIRECTION('ref_axis',(-1.,0.,0.));
#11473=DIRECTION('center_axis',(0.,-1.,2.49912569936186E-12));
#11474=DIRECTION('ref_axis',(-1.,0.,0.));
#11475=DIRECTION('center_axis',(0.,1.,1.09634523681734E-15));
#11476=DIRECTION('ref_axis',(1.,0.,0.));
#11477=DIRECTION('center_axis',(0.,-1.,1.24912569936654E-12));
#11478=DIRECTION('ref_axis',(1.,0.,0.));
#11479=DIRECTION('',(0.707106781186547,-0.707106781186548,-8.61828757098662E-16));
#11480=DIRECTION('center_axis',(0.,1.,-1.28117698141774E-12));
#11481=DIRECTION('ref_axis',(1.,0.,0.));
#11482=DIRECTION('center_axis',(0.,-1.,-8.74300631892309E-16));
#11483=DIRECTION('ref_axis',(1.,0.,0.));
#11484=DIRECTION('',(0.,1.,8.74300631892309E-16));
#11485=DIRECTION('center_axis',(0.,1.,-1.24912569936654E-12));
#11486=DIRECTION('ref_axis',(1.,0.,0.));
#11487=DIRECTION('center_axis',(0.,-1.,-8.74300631892309E-16));
#11488=DIRECTION('ref_axis',(0.,-8.74300631892309E-16,1.));
#11489=DIRECTION('center_axis',(0.,1.,-1.665792366032E-12));
#11490=DIRECTION('ref_axis',(-1.,0.,0.));
#11491=DIRECTION('center_axis',(0.,-1.,-1.09634523681734E-15));
#11492=DIRECTION('ref_axis',(1.,0.,0.));
#11493=DIRECTION('',(0.707106781186547,0.707106781186548,8.61828757098662E-16));
#11494=DIRECTION('center_axis',(0.,1.,8.74300631892318E-16));
#11495=DIRECTION('ref_axis',(1.,0.,0.));
#11496=DIRECTION('center_axis',(0.,-1.,4.76103046125019E-12));
#11497=DIRECTION('ref_axis',(1.,0.,0.));
#11498=DIRECTION('',(-0.707106781186547,0.707106781186548,7.04819511230291E-16));
#11499=DIRECTION('center_axis',(0.,-1.,4.76103046125019E-12));
#11500=DIRECTION('ref_axis',(1.,0.,0.));
#11501=DIRECTION('center_axis',(0.,-1.,-8.74300631892318E-16));
#11502=DIRECTION('ref_axis',(-1.,0.,0.));
#11503=DIRECTION('',(0.,-1.,-8.74300631892318E-16));
#11504=DIRECTION('center_axis',(0.,1.,-4.76103046125019E-12));
#11505=DIRECTION('ref_axis',(-1.,0.,0.));
#11506=DIRECTION('center_axis',(0.,1.,-4.76103046125019E-12));
#11507=DIRECTION('ref_axis',(-1.,0.,0.));
#11508=DIRECTION('center_axis',(0.,1.,6.52256026967277E-16));
#11509=DIRECTION('ref_axis',(1.,0.,0.));
#11510=DIRECTION('center_axis',(0.,-1.,-6.52256026967277E-16));
#11511=DIRECTION('ref_axis',(1.,0.,0.));
#11512=DIRECTION('',(-0.813733471206735,-0.581238193719097,-4.78769724044094E-16));
#11513=DIRECTION('center_axis',(0.,1.,6.52256026967277E-16));
#11514=DIRECTION('ref_axis',(1.,0.,0.));
#11515=DIRECTION('center_axis',(0.,1.,-8.96208730519314E-13));
#11516=DIRECTION('ref_axis',(1.,0.,0.));
#11517=DIRECTION('center_axis',(0.,1.,-1.66030339217348E-12));
#11518=DIRECTION('ref_axis',(-1.,0.,0.));
#11519=DIRECTION('center_axis',(0.,1.,6.52256026967277E-16));
#11520=DIRECTION('ref_axis',(1.,0.,0.));
#11521=DIRECTION('center_axis',(0.,1.,-8.96208730519314E-13));
#11522=DIRECTION('ref_axis',(1.,0.,0.));
#11523=DIRECTION('center_axis',(0.,1.,-1.69748481005457E-12));
#11524=DIRECTION('ref_axis',(-1.,0.,0.));
#11525=DIRECTION('center_axis',(0.,-1.,-6.52256026967277E-16));
#11526=DIRECTION('ref_axis',(0.,-6.52256026967277E-16,1.));
#11527=DIRECTION('center_axis',(0.,-1.,8.96208730519314E-13));
#11528=DIRECTION('ref_axis',(1.,0.,0.));
#11529=DIRECTION('center_axis',(0.,-1.,1.68250544832888E-12));
#11530=DIRECTION('ref_axis',(-1.,0.,0.));
#11531=DIRECTION('center_axis',(0.,1.,6.52256026967277E-16));
#11532=DIRECTION('ref_axis',(1.,0.,0.));
#11533=DIRECTION('center_axis',(0.,1.,-8.96208730519314E-13));
#11534=DIRECTION('ref_axis',(1.,0.,0.));
#11535=DIRECTION('center_axis',(0.,1.,-1.73612621739787E-12));
#11536=DIRECTION('ref_axis',(-1.,0.,0.));
#11537=DIRECTION('center_axis',(0.,-1.,-6.52256026967277E-16));
#11538=DIRECTION('ref_axis',(0.,-6.52256026967277E-16,1.));
#11539=DIRECTION('center_axis',(0.,-1.,8.96208730519314E-13));
#11540=DIRECTION('ref_axis',(1.,0.,0.));
#11541=DIRECTION('center_axis',(0.,-1.,1.7204605278621E-12));
#11542=DIRECTION('ref_axis',(-1.,0.,0.));
#11543=DIRECTION('center_axis',(0.,1.,6.52256026967277E-16));
#11544=DIRECTION('ref_axis',(1.,0.,0.));
#11545=DIRECTION('center_axis',(0.,1.,-8.96208730519314E-13));
#11546=DIRECTION('ref_axis',(1.,0.,0.));
#11547=DIRECTION('center_axis',(0.,1.,-1.77656715745294E-12));
#11548=DIRECTION('ref_axis',(-1.,0.,0.));
#11549=DIRECTION('center_axis',(0.,-1.,-6.52256026967277E-16));
#11550=DIRECTION('ref_axis',(0.,-6.52256026967277E-16,1.));
#11551=DIRECTION('center_axis',(0.,-1.,8.96208730519314E-13));
#11552=DIRECTION('ref_axis',(1.,0.,0.));
#11553=DIRECTION('center_axis',(0.,-1.,1.76016686652978E-12));
#11554=DIRECTION('ref_axis',(-1.,0.,0.));
#11555=DIRECTION('center_axis',(0.,1.,6.52256026967277E-16));
#11556=DIRECTION('ref_axis',(1.,0.,0.));
#11557=DIRECTION('center_axis',(0.,1.,-8.96208730519314E-13));
#11558=DIRECTION('ref_axis',(1.,0.,0.));
#11559=DIRECTION('center_axis',(0.,1.,-1.81893633360534E-12));
#11560=DIRECTION('ref_axis',(-1.,0.,0.));
#11561=DIRECTION('center_axis',(0.,-1.,-6.52256026967277E-16));
#11562=DIRECTION('ref_axis',(0.,-6.52256026967277E-16,1.));
#11563=DIRECTION('center_axis',(0.,-1.,8.96208730519314E-13));
#11564=DIRECTION('ref_axis',(1.,0.,0.));
#11565=DIRECTION('center_axis',(0.,-1.,1.80174853205239E-12));
#11566=DIRECTION('ref_axis',(-1.,0.,0.));
#11567=DIRECTION('center_axis',(0.,1.,6.52256026967277E-16));
#11568=DIRECTION('ref_axis',(1.,0.,0.));
#11569=DIRECTION('center_axis',(0.,1.,-8.96208730519314E-13));
#11570=DIRECTION('ref_axis',(1.,0.,0.));
#11571=DIRECTION('center_axis',(0.,1.,-1.86337502221387E-12));
#11572=DIRECTION('ref_axis',(-1.,0.,0.));
#11573=DIRECTION('center_axis',(0.,-1.,-6.52256026967277E-16));
#11574=DIRECTION('ref_axis',(0.,-6.52256026967277E-16,1.));
#11575=DIRECTION('center_axis',(0.,-1.,8.96208730519314E-13));
#11576=DIRECTION('ref_axis',(1.,0.,0.));
#11577=DIRECTION('center_axis',(0.,-1.,1.84534159501235E-12));
#11578=DIRECTION('ref_axis',(-1.,0.,0.));
#11579=DIRECTION('center_axis',(0.,-1.,-8.74300631892309E-16));
#11580=DIRECTION('ref_axis',(0.,-8.74300631892309E-16,1.));
#11581=DIRECTION('center_axis',(0.,-1.,8.95986685914389E-13));
#11582=DIRECTION('ref_axis',(-1.,0.,0.));
#11583=DIRECTION('center_axis',(0.,1.,-1.90981660175007E-12));
#11584=DIRECTION('ref_axis',(-1.,0.,0.));
#11585=DIRECTION('center_axis',(0.,-1.,-8.74300631892309E-16));
#11586=DIRECTION('ref_axis',(0.,-8.74300631892309E-16,1.));
#11587=DIRECTION('center_axis',(0.,-1.,8.95986685914389E-13));
#11588=DIRECTION('ref_axis',(-1.,0.,0.));
#11589=DIRECTION('center_axis',(0.,-1.,1.89087357173833E-12));
#11590=DIRECTION('ref_axis',(-1.,0.,0.));
#11591=DIRECTION('center_axis',(0.,-1.,-8.74300631892309E-16));
#11592=DIRECTION('ref_axis',(0.,-8.74300631892309E-16,1.));
#11593=DIRECTION('center_axis',(0.,-1.,8.95986685914389E-13));
#11594=DIRECTION('ref_axis',(-1.,0.,0.));
#11595=DIRECTION('center_axis',(0.,-1.,1.93895331704599E-12));
#11596=DIRECTION('ref_axis',(-1.,0.,0.));
#11597=DIRECTION('center_axis',(0.,-1.,-8.74300631892309E-16));
#11598=DIRECTION('ref_axis',(0.,-8.74300631892309E-16,1.));
#11599=DIRECTION('center_axis',(0.,-1.,8.95986685914389E-13));
#11600=DIRECTION('ref_axis',(-1.,0.,0.));
#11601=DIRECTION('center_axis',(0.,1.,-1.95887654741229E-12));
#11602=DIRECTION('ref_axis',(-1.,0.,0.));
#11603=DIRECTION('center_axis',(0.,-1.,-6.52256026967277E-16));
#11604=DIRECTION('ref_axis',(1.,0.,0.));
#11605=DIRECTION('center_axis',(0.,-1.,8.96208730519314E-13));
#11606=DIRECTION('ref_axis',(1.,0.,0.));
#11607=DIRECTION('',(0.,1.,6.52256026967277E-16));
#11608=DIRECTION('center_axis',(0.,-1.,-6.52256026967277E-16));
#11609=DIRECTION('ref_axis',(1.,0.,0.));
#11610=DIRECTION('',(0.,1.,6.52256026967277E-16));
#11611=DIRECTION('center_axis',(0.,-1.,-6.52256026967277E-16));
#11612=DIRECTION('ref_axis',(1.,0.,0.));
#11613=DIRECTION('',(0.,1.,6.52256026967277E-16));
#11614=DIRECTION('center_axis',(0.,-1.,-6.52256026967277E-16));
#11615=DIRECTION('ref_axis',(1.,0.,0.));
#11616=DIRECTION('',(0.,1.,6.52256026967277E-16));
#11617=DIRECTION('center_axis',(0.,-1.,-6.52256026967277E-16));
#11618=DIRECTION('ref_axis',(1.,0.,0.));
#11619=DIRECTION('',(0.,1.,6.52256026967277E-16));
#11620=DIRECTION('center_axis',(0.,-1.,-6.52256026967277E-16));
#11621=DIRECTION('ref_axis',(1.,0.,0.));
#11622=DIRECTION('',(0.,1.,6.52256026967277E-16));
#11623=DIRECTION('center_axis',(0.,-1.,-8.74300631892309E-16));
#11624=DIRECTION('ref_axis',(-1.,0.,0.));
#11625=DIRECTION('',(0.,1.,8.74300631892309E-16));
#11626=DIRECTION('center_axis',(0.,-1.,-8.74300631892309E-16));
#11627=DIRECTION('ref_axis',(-1.,0.,0.));
#11628=DIRECTION('',(0.,1.,8.74300631892309E-16));
#11629=DIRECTION('center_axis',(0.,-1.,-8.74300631892309E-16));
#11630=DIRECTION('ref_axis',(-1.,0.,0.));
#11631=DIRECTION('',(-0.0523359562429438,0.998629534754574,8.66693127132923E-16));
#11632=DIRECTION('center_axis',(0.,1.,-1.98954073916915E-12));
#11633=DIRECTION('ref_axis',(-1.,0.,0.));
#11634=DIRECTION('center_axis',(0.,-1.,-8.74300631892309E-16));
#11635=DIRECTION('ref_axis',(-1.,0.,0.));
#11636=DIRECTION('',(-0.0523359562429438,0.998629534754574,8.66693127132923E-16));
#11637=DIRECTION('center_axis',(0.,-1.,-8.74300631892309E-16));
#11638=DIRECTION('ref_axis',(-1.,0.,0.));
#11639=DIRECTION('',(-0.0523359562429438,0.998629534754574,8.66693127132923E-16));
#11640=DIRECTION('center_axis',(0.,-1.,-8.74300631892309E-16));
#11641=DIRECTION('ref_axis',(-1.,0.,0.));
#11642=DIRECTION('',(-0.0523359562429438,0.998629534754574,8.66693127132923E-16));
#11643=DIRECTION('center_axis',(0.,-1.,-8.74300631892309E-16));
#11644=DIRECTION('ref_axis',(-1.,0.,0.));
#11645=DIRECTION('',(-0.0523359562429438,0.998629534754574,8.66693127132923E-16));
#11646=DIRECTION('center_axis',(0.,-1.,-8.74300631892309E-16));
#11647=DIRECTION('ref_axis',(-1.,0.,0.));
#11648=DIRECTION('',(-0.0523359562429438,0.998629534754574,8.66693127132923E-16));
#11649=DIRECTION('center_axis',(0.,-1.,-8.74300631892309E-16));
#11650=DIRECTION('ref_axis',(-1.,0.,0.));
#11651=DIRECTION('',(-0.0523359562429438,0.998629534754574,8.66693127132923E-16));
#11652=DIRECTION('center_axis',(0.,-1.,-6.52256026967277E-16));
#11653=DIRECTION('ref_axis',(0.,-6.52256026967277E-16,1.));
#11654=DIRECTION('center_axis',(0.,-1.,-8.74300631892309E-16));
#11655=DIRECTION('ref_axis',(-1.,0.,0.));
#11656=DIRECTION('center_axis',(0.,-1.,2.12243424546674E-12));
#11657=DIRECTION('ref_axis',(-1.,0.,0.));
#11658=DIRECTION('',(-0.0523359562429438,0.998629534754574,8.66693127132923E-16));
#11659=DIRECTION('center_axis',(0.,1.,-2.15847746020963E-12));
#11660=DIRECTION('ref_axis',(-1.,0.,0.));
#11661=DIRECTION('center_axis',(0.,-1.,-8.74300631892309E-16));
#11662=DIRECTION('ref_axis',(-1.,0.,0.));
#11663=DIRECTION('center_axis',(0.,-1.,2.18319386742199E-12));
#11664=DIRECTION('ref_axis',(-1.,0.,0.));
#11665=DIRECTION('',(-0.0523359562429438,0.998629534754574,8.66693127132923E-16));
#11666=DIRECTION('center_axis',(0.,1.,-2.2213479215854E-12));
#11667=DIRECTION('ref_axis',(-1.,0.,0.));
#11668=DIRECTION('center_axis',(0.,-1.,-8.74300631892309E-16));
#11669=DIRECTION('ref_axis',(-1.,0.,0.));
#11670=DIRECTION('center_axis',(0.,-1.,2.0649637236167E-12));
#11671=DIRECTION('ref_axis',(-1.,0.,0.));
#11672=DIRECTION('',(-0.0523359562429438,0.998629534754574,8.66693127132923E-16));
#11673=DIRECTION('center_axis',(0.,1.,-2.09906654771079E-12));
#11674=DIRECTION('ref_axis',(-1.,0.,0.));
#11675=DIRECTION('center_axis',(0.,-1.,-8.74300631892309E-16));
#11676=DIRECTION('ref_axis',(-1.,0.,0.));
#11677=DIRECTION('center_axis',(0.,-1.,2.0105222668657E-12));
#11678=DIRECTION('ref_axis',(-1.,0.,0.));
#11679=DIRECTION('',(-0.0523359562429438,0.998629534754574,8.66693127132923E-16));
#11680=DIRECTION('center_axis',(0.,1.,-2.0428372792574E-12));
#11681=DIRECTION('ref_axis',(-1.,0.,0.));
#11682=DIRECTION('center_axis',(0.,-1.,-8.74300631892309E-16));
#11683=DIRECTION('ref_axis',(-1.,0.,0.));
#11684=DIRECTION('',(-0.0523359562429438,0.998629534754574,8.66693127132923E-16));
#11685=DIRECTION('center_axis',(0.,-1.,-8.74300631892309E-16));
#11686=DIRECTION('ref_axis',(0.,-8.74300631892309E-16,1.));
#11687=DIRECTION('center_axis',(0.,-1.,8.95986685914389E-13));
#11688=DIRECTION('ref_axis',(-1.,0.,0.));
#11689=DIRECTION('center_axis',(0.,-1.,-8.74300631892309E-16));
#11690=DIRECTION('ref_axis',(-1.,0.,0.));
#11691=DIRECTION('center_axis',(0.,-1.,8.95986685914389E-13));
#11692=DIRECTION('ref_axis',(-1.,0.,0.));
#11693=DIRECTION('',(0.,1.,8.74300631892309E-16));
#11694=DIRECTION('center_axis',(0.,-1.,-8.74300631892309E-16));
#11695=DIRECTION('ref_axis',(0.,-8.74300631892309E-16,1.));
#11696=DIRECTION('center_axis',(0.,-1.,-8.74300631892309E-16));
#11697=DIRECTION('ref_axis',(0.,-8.74300631892309E-16,1.));
#11698=DIRECTION('center_axis',(0.,-1.,8.95986685914389E-13));
#11699=DIRECTION('ref_axis',(-1.,0.,0.));
#11700=DIRECTION('center_axis',(0.,-1.,-8.74300631892309E-16));
#11701=DIRECTION('ref_axis',(-1.,0.,0.));
#11702=DIRECTION('center_axis',(0.,-1.,8.95986685914389E-13));
#11703=DIRECTION('ref_axis',(-1.,0.,0.));
#11704=DIRECTION('',(0.,1.,8.74300631892309E-16));
#11705=DIRECTION('center_axis',(0.,-1.,-8.74300631892309E-16));
#11706=DIRECTION('ref_axis',(0.,-8.74300631892309E-16,1.));
#11707=DIRECTION('center_axis',(0.,-1.,-8.74300631892309E-16));
#11708=DIRECTION('ref_axis',(0.,-8.74300631892309E-16,1.));
#11709=DIRECTION('center_axis',(0.,-1.,8.95986685914389E-13));
#11710=DIRECTION('ref_axis',(-1.,0.,0.));
#11711=DIRECTION('center_axis',(0.,-1.,-8.74300631892309E-16));
#11712=DIRECTION('ref_axis',(-1.,0.,0.));
#11713=DIRECTION('center_axis',(0.,-1.,8.95986685914389E-13));
#11714=DIRECTION('ref_axis',(-1.,0.,0.));
#11715=DIRECTION('',(0.,1.,8.74300631892309E-16));
#11716=DIRECTION('center_axis',(0.,-1.,-8.74300631892309E-16));
#11717=DIRECTION('ref_axis',(0.,-8.74300631892309E-16,1.));
#11718=DIRECTION('center_axis',(0.,-1.,-8.74300631892309E-16));
#11719=DIRECTION('ref_axis',(0.,-8.74300631892309E-16,1.));
#11720=DIRECTION('center_axis',(0.,-1.,1.24912569936654E-12));
#11721=DIRECTION('ref_axis',(-1.,0.,0.));
#11722=DIRECTION('center_axis',(0.,-1.,-8.74300631892309E-16));
#11723=DIRECTION('ref_axis',(-1.,0.,0.));
#11724=DIRECTION('center_axis',(0.,-1.,1.24912569936654E-12));
#11725=DIRECTION('ref_axis',(-1.,0.,0.));
#11726=DIRECTION('',(0.,1.,8.74300631892309E-16));
#11727=DIRECTION('center_axis',(0.,-1.,-8.74300631892309E-16));
#11728=DIRECTION('ref_axis',(0.,-8.74300631892309E-16,1.));
#11729=DIRECTION('center_axis',(0.,-1.,-8.74300631892309E-16));
#11730=DIRECTION('ref_axis',(0.,-8.74300631892309E-16,1.));
#11731=DIRECTION('center_axis',(0.,-1.,1.24912569936654E-12));
#11732=DIRECTION('ref_axis',(-1.,0.,0.));
#11733=DIRECTION('center_axis',(0.,-1.,1.665792366032E-12));
#11734=DIRECTION('ref_axis',(-1.,0.,0.));
#11735=DIRECTION('center_axis',(0.,-1.,-8.74300631892309E-16));
#11736=DIRECTION('ref_axis',(-1.,0.,0.));
#11737=DIRECTION('center_axis',(0.,-1.,1.24912569936654E-12));
#11738=DIRECTION('ref_axis',(-1.,0.,0.));
#11739=DIRECTION('',(0.,1.,8.74300631892309E-16));
#11740=DIRECTION('center_axis',(0.,-1.,-8.74300631892309E-16));
#11741=DIRECTION('ref_axis',(0.,-8.74300631892309E-16,1.));
#11742=DIRECTION('center_axis',(0.,-1.,-8.74300631892309E-16));
#11743=DIRECTION('ref_axis',(-1.,0.,0.));
#11744=DIRECTION('',(0.,1.,8.74300631892309E-16));
#11745=DIRECTION('axis',(0.,0.,1.));
#11746=DIRECTION('refdir',(1.,0.,0.));
#11747=DIRECTION('center_axis',(0.,0.927650238806477,0.373450176653173));
#11748=DIRECTION('ref_axis',(-1.,0.,0.));
#11749=DIRECTION('',(0.,-0.373450176653687,0.92765023880627));
#11750=DIRECTION('',(1.,0.,0.));
#11751=DIRECTION('center_axis',(0.,0.927650238805982,0.373450176654402));
#11752=DIRECTION('ref_axis',(0.,0.373450176654402,-0.927650238805982));
#11753=DIRECTION('',(1.,0.,0.));
#11754=DIRECTION('center_axis',(0.,1.,1.09634523681734E-15));
#11755=DIRECTION('ref_axis',(1.,0.,0.));
#11756=DIRECTION('',(0.,1.09634523681734E-15,-1.));
#11757=DIRECTION('center_axis',(0.,-1.,-1.09634523681734E-15));
#11758=DIRECTION('ref_axis',(1.,0.,0.));
#11759=DIRECTION('center_axis',(0.,0.927650238806478,0.373450176653172));
#11760=DIRECTION('ref_axis',(-1.,0.,0.));
#11761=DIRECTION('center_axis',(0.,0.927650238805982,0.373450176654402));
#11762=DIRECTION('ref_axis',(0.,0.373450176654402,-0.927650238805982));
#11763=DIRECTION('',(1.,0.,0.));
#11764=DIRECTION('',(0.,0.373450176653686,-0.927650238806271));
#11765=DIRECTION('',(1.,0.,0.));
#11766=DIRECTION('center_axis',(0.,1.,1.09634523681734E-15));
#11767=DIRECTION('ref_axis',(1.,0.,0.));
#11768=DIRECTION('center_axis',(0.,-1.,-1.09634523681734E-15));
#11769=DIRECTION('ref_axis',(1.,0.,0.));
#11770=DIRECTION('',(0.,-1.09634523681734E-15,1.));
#11771=DIRECTION('center_axis',(0.,1.,1.09634523681734E-15));
#11772=DIRECTION('ref_axis',(1.,0.,0.));
#11773=DIRECTION('',(0.,1.,1.09634523681734E-15));
#11774=DIRECTION('center_axis',(0.,1.,1.09634523681734E-15));
#11775=DIRECTION('ref_axis',(1.,0.,0.));
#11776=DIRECTION('',(0.,1.,1.09634523681734E-15));
#11777=DIRECTION('center_axis',(0.,1.,1.09634523681734E-15));
#11778=DIRECTION('ref_axis',(1.,0.,0.));
#11779=DIRECTION('center_axis',(-1.,0.,0.));
#11780=DIRECTION('ref_axis',(0.,1.,1.09634523681734E-15));
#11781=DIRECTION('',(0.,-1.09634523681734E-15,1.));
#11782=DIRECTION('',(0.,1.,1.09634523681734E-15));
#11783=DIRECTION('',(0.,-1.09634523681734E-15,1.));
#11784=DIRECTION('center_axis',(1.,0.,0.));
#11785=DIRECTION('ref_axis',(0.,1.09634523681734E-15,-1.));
#11786=DIRECTION('',(0.,1.,1.09634523681734E-15));
#11787=DIRECTION('',(0.,-1.09634523681734E-15,1.));
#11788=DIRECTION('',(0.,1.,1.09634523681734E-15));
#11789=DIRECTION('',(0.,1.09634523681734E-15,-1.));
#11790=DIRECTION('center_axis',(0.,1.09634523681734E-15,-1.));
#11791=DIRECTION('ref_axis',(1.,0.,0.));
#11792=DIRECTION('',(1.,0.,0.));
#11793=DIRECTION('',(0.,1.,1.09634523681734E-15));
#11794=DIRECTION('',(-1.,0.,0.));
#11795=DIRECTION('',(0.,1.,1.09634523681734E-15));
#11796=DIRECTION('center_axis',(0.,-1.09634523681734E-15,1.));
#11797=DIRECTION('ref_axis',(0.,-1.,-1.09634523681734E-15));
#11798=DIRECTION('',(-1.,0.,0.));
#11799=DIRECTION('',(0.,1.,1.09634523681734E-15));
#11800=DIRECTION('',(1.,0.,0.));
#11801=DIRECTION('',(0.,1.,1.09634523681734E-15));
#11802=DIRECTION('center_axis',(0.,1.,1.09634523681734E-15));
#11803=DIRECTION('ref_axis',(1.,0.,0.));
#11804=DIRECTION('',(0.,-1.09634523681734E-15,1.));
#11805=DIRECTION('',(0.,1.09634523681734E-15,-1.));
#11806=DIRECTION('center_axis',(0.,1.,1.09634523681734E-15));
#11807=DIRECTION('ref_axis',(6.12323399573677E-17,1.09634523681734E-15,
-1.));
#11808=DIRECTION('center_axis',(0.,1.,1.09634523681734E-15));
#11809=DIRECTION('ref_axis',(1.,0.,0.));
#11810=DIRECTION('center_axis',(0.,-1.,-1.09634523681734E-15));
#11811=DIRECTION('ref_axis',(1.,0.,0.));
#11812=DIRECTION('center_axis',(0.,1.,1.09634523681734E-15));
#11813=DIRECTION('ref_axis',(-0.994617989425745,-1.13592451729936E-16,0.103610111044667));
#11814=DIRECTION('center_axis',(0.,1.,1.09634523681734E-15));
#11815=DIRECTION('ref_axis',(1.,0.,0.));
#11816=DIRECTION('',(0.,1.,1.09634523681734E-15));
#11817=DIRECTION('center_axis',(0.,1.,1.09634523681734E-15));
#11818=DIRECTION('ref_axis',(1.,0.,0.));
#11819=DIRECTION('center_axis',(-1.,0.,0.));
#11820=DIRECTION('ref_axis',(0.,1.,1.09634523681734E-15));
#11821=DIRECTION('',(0.,1.09634523681734E-15,-1.));
#11822=DIRECTION('',(0.,-1.09634523681734E-15,1.));
#11823=DIRECTION('center_axis',(1.,0.,0.));
#11824=DIRECTION('ref_axis',(0.,1.09634523681734E-15,-1.));
#11825=DIRECTION('',(0.,-1.09634523681734E-15,1.));
#11826=DIRECTION('',(0.,1.09634523681734E-15,-1.));
#11827=DIRECTION('center_axis',(0.,1.,1.09634523681734E-15));
#11828=DIRECTION('ref_axis',(1.,0.,0.));
#11829=DIRECTION('center_axis',(0.,1.,1.09634523681734E-15));
#11830=DIRECTION('ref_axis',(1.,0.,0.));
#11831=DIRECTION('axis',(0.,0.,1.));
#11832=DIRECTION('refdir',(1.,0.,0.));
#11833=DIRECTION('center_axis',(0.984807753012209,-0.173648177666927,-6.9026791896102E-15));
#11834=DIRECTION('ref_axis',(6.74488507274914E-15,-1.49880108324396E-15,
1.));
#11835=DIRECTION('center_axis',(0.984807753012209,-0.173648177666927,-6.9026791896102E-15));
#11836=DIRECTION('ref_axis',(-0.173648177666927,-0.984807753012209,-1.41609297436625E-15));
#11837=DIRECTION('center_axis',(-6.74488507274914E-15,1.49880108324396E-15,
-1.));
#11838=DIRECTION('ref_axis',(-0.173648177666927,-0.984807753012209,-3.04793925546002E-16));
#11839=DIRECTION('center_axis',(1.31243041282465E-11,-2.31385942497016E-12,
-1.));
#11840=DIRECTION('ref_axis',(-0.173648177666927,-0.984807753012209,-3.04793925546223E-16));
#11841=DIRECTION('',(6.74488507274914E-15,-1.49880108324396E-15,1.));
#11842=DIRECTION('center_axis',(1.31243041282465E-11,-2.31385942497016E-12,
-1.));
#11843=DIRECTION('ref_axis',(-0.173648177666927,-0.984807753012209,-3.04793925546223E-16));
#11844=DIRECTION('center_axis',(1.31243041282465E-11,-2.31385942497016E-12,
-1.));
#11845=DIRECTION('ref_axis',(-0.173648177666927,-0.984807753012209,-3.04793925546223E-16));
#11846=DIRECTION('center_axis',(0.173648177666927,0.984807753012209,1.41609297436625E-15));
#11847=DIRECTION('ref_axis',(-6.47630097698008E-15,1.85037170770859E-15,
-1.));
#11848=DIRECTION('center_axis',(-0.173648177666927,-0.984807753012209,-1.41609297436625E-15));
#11849=DIRECTION('ref_axis',(-6.31282311555423E-15,2.55105953078819E-15,
-1.));
#11850=DIRECTION('center_axis',(0.984807753012209,-0.173648177666927,-6.9026791896102E-15));
#11851=DIRECTION('ref_axis',(-0.173648177666927,-0.984807753012209,-1.41609297436625E-15));
#11852=DIRECTION('center_axis',(0.984807753012209,-0.173648177666927,-6.9026791896102E-15));
#11853=DIRECTION('ref_axis',(-0.173648177666927,-0.984807753012209,-1.41609297436625E-15));
#11854=DIRECTION('center_axis',(0.984807753012209,-0.173648177666927,-6.9026791896102E-15));
#11855=DIRECTION('ref_axis',(-0.173648177666927,-0.984807753012209,-1.41609297436625E-15));
#11856=DIRECTION('',(-0.984807753012209,0.173648177666927,6.9026791896102E-15));
#11857=DIRECTION('center_axis',(-6.46591174117934E-15,1.44961055799008E-15,
-1.));
#11858=DIRECTION('ref_axis',(-0.173648177666927,-0.984807753012209,-3.04793925546006E-16));
#11859=DIRECTION('axis',(0.,0.,1.));
#11860=DIRECTION('refdir',(1.,0.,0.));
#11861=DIRECTION('center_axis',(-6.74488507274914E-15,1.49880108324396E-15,
-1.));
#11862=DIRECTION('ref_axis',(-0.173648177666927,-0.984807753012209,-3.04793925546002E-16));
#11863=DIRECTION('center_axis',(2.62550741678841E-11,-4.62916846043658E-12,
-1.));
#11864=DIRECTION('ref_axis',(-0.173648177666927,-0.984807753012209,-3.04793925548737E-16));
#11865=DIRECTION('',(6.74488507274914E-15,-1.49880108324396E-15,1.));
#11866=DIRECTION('center_axis',(2.62550741678841E-11,-4.62916846043658E-12,
-1.));
#11867=DIRECTION('ref_axis',(-0.173648177666927,-0.984807753012209,-3.04793925548737E-16));
#11868=DIRECTION('center_axis',(2.62550741678841E-11,-4.62916846043658E-12,
-1.));
#11869=DIRECTION('ref_axis',(-0.173648177666927,-0.984807753012209,-3.04793925548737E-16));
#11870=DIRECTION('center_axis',(0.173648177666927,0.984807753012209,1.41609297436625E-15));
#11871=DIRECTION('ref_axis',(-6.16790569236198E-15,2.05596856412066E-15,
-1.));
#11872=DIRECTION('center_axis',(-0.173648177666927,-0.984807753012209,-1.41609297436625E-15));
#11873=DIRECTION('ref_axis',(-5.78605122952035E-15,2.45817543460173E-15,
-1.));
#11874=DIRECTION('center_axis',(0.984807753012209,-0.173648177666927,-6.9026791896102E-15));
#11875=DIRECTION('ref_axis',(-0.173648177666927,-0.984807753012209,-1.41609297436625E-15));
#11876=DIRECTION('center_axis',(0.984807753012209,-0.173648177666927,-6.9026791896102E-15));
#11877=DIRECTION('ref_axis',(-0.173648177666927,-0.984807753012209,-1.41609297436625E-15));
#11878=DIRECTION('center_axis',(0.984807753012209,-0.173648177666927,-6.9026791896102E-15));
#11879=DIRECTION('ref_axis',(-0.173648177666927,-0.984807753012209,-1.41609297436625E-15));
#11880=DIRECTION('',(-0.984807753012209,0.173648177666927,6.9026791896102E-15));
#11881=DIRECTION('center_axis',(0.984807753012209,-0.173648177666927,-6.9026791896102E-15));
#11882=DIRECTION('ref_axis',(-0.173648177666927,-0.984807753012209,-1.41609297436625E-15));
#11883=DIRECTION('center_axis',(-6.46591174117934E-15,1.44961055799008E-15,
-1.));
#11884=DIRECTION('ref_axis',(-0.173648177666927,-0.984807753012209,-3.04793925546006E-16));
#11885=DIRECTION('center_axis',(0.984807753012209,-0.173648177666927,-6.9026791896102E-15));
#11886=DIRECTION('ref_axis',(6.74488507274914E-15,-1.49880108324396E-15,
1.));
#11887=DIRECTION('axis',(0.,0.,1.));
#11888=DIRECTION('refdir',(1.,0.,0.));
#11889=DIRECTION('center_axis',(-6.74488507274914E-15,1.49880108324396E-15,
-1.));
#11890=DIRECTION('ref_axis',(-0.173648177666927,-0.984807753012209,-3.04793925546002E-16));
#11891=DIRECTION('center_axis',(2.62550741678841E-11,-4.62916846043658E-12,
-1.));
#11892=DIRECTION('ref_axis',(-0.173648177666927,-0.984807753012209,-3.04793925548737E-16));
#11893=DIRECTION('',(6.74488507274914E-15,-1.49880108324396E-15,1.));
#11894=DIRECTION('center_axis',(2.62550741678841E-11,-4.62916846043658E-12,
-1.));
#11895=DIRECTION('ref_axis',(-0.173648177666927,-0.984807753012209,-3.04793925548737E-16));
#11896=DIRECTION('center_axis',(2.62550741678841E-11,-4.62916846043658E-12,
-1.));
#11897=DIRECTION('ref_axis',(-0.173648177666927,-0.984807753012209,-3.04793925548737E-16));
#11898=DIRECTION('center_axis',(0.173648177666927,0.984807753012209,1.41609297436625E-15));
#11899=DIRECTION('ref_axis',(-6.16790569236198E-15,2.05596856412066E-15,
-1.));
#11900=DIRECTION('center_axis',(-0.173648177666927,-0.984807753012209,-1.41609297436625E-15));
#11901=DIRECTION('ref_axis',(-5.78605122952035E-15,2.45817543460173E-15,
-1.));
#11902=DIRECTION('center_axis',(0.984807753012209,-0.173648177666927,-6.9026791896102E-15));
#11903=DIRECTION('ref_axis',(-0.173648177666927,-0.984807753012209,-1.41609297436625E-15));
#11904=DIRECTION('center_axis',(0.984807753012209,-0.173648177666927,-6.9026791896102E-15));
#11905=DIRECTION('ref_axis',(-0.173648177666927,-0.984807753012209,-1.41609297436625E-15));
#11906=DIRECTION('center_axis',(0.984807753012209,-0.173648177666927,-6.9026791896102E-15));
#11907=DIRECTION('ref_axis',(-0.173648177666927,-0.984807753012209,-1.41609297436625E-15));
#11908=DIRECTION('',(-0.984807753012209,0.173648177666927,6.9026791896102E-15));
#11909=DIRECTION('center_axis',(0.984807753012209,-0.173648177666927,-6.9026791896102E-15));
#11910=DIRECTION('ref_axis',(-0.173648177666927,-0.984807753012209,-1.41609297436625E-15));
#11911=DIRECTION('center_axis',(-6.46591174117934E-15,1.44961055799008E-15,
-1.));
#11912=DIRECTION('ref_axis',(-0.173648177666927,-0.984807753012209,-3.04793925546006E-16));
#11913=DIRECTION('center_axis',(0.984807753012209,-0.173648177666927,-6.9026791896102E-15));
#11914=DIRECTION('ref_axis',(6.74488507274914E-15,-1.49880108324396E-15,
1.));
#11915=DIRECTION('axis',(0.,0.,1.));
#11916=DIRECTION('refdir',(1.,0.,0.));
#11917=DIRECTION('center_axis',(1.66533453693773E-16,1.,1.1518563880486E-15));
#11918=DIRECTION('ref_axis',(1.,-1.66533453693753E-16,-1.72407814243868E-14));
#11919=DIRECTION('',(1.66533453693773E-16,1.,1.1518563880486E-15));
#11920=DIRECTION('center_axis',(1.66533453693773E-16,1.,1.1518563880486E-15));
#11921=DIRECTION('ref_axis',(1.,-1.66533453693753E-16,-1.72407814243868E-14));
#11922=DIRECTION('',(1.66533453693773E-16,1.,1.1518563880486E-15));
#11923=DIRECTION('center_axis',(1.66533453693773E-16,1.,1.1518563880486E-15));
#11924=DIRECTION('ref_axis',(1.,-1.66533453693753E-16,-1.72407814243868E-14));
#11925=DIRECTION('',(1.66533453693773E-16,1.,1.1518563880486E-15));
#11926=DIRECTION('center_axis',(1.66533453693773E-16,1.,1.1518563880486E-15));
#11927=DIRECTION('ref_axis',(1.,-1.66533453693753E-16,-1.72407814243868E-14));
#11928=DIRECTION('',(1.66533453693773E-16,1.,1.1518563880486E-15));
#11929=DIRECTION('center_axis',(1.66533453693773E-16,1.,1.1518563880486E-15));
#11930=DIRECTION('ref_axis',(1.,-1.66533453693753E-16,-1.72407814243868E-14));
#11931=DIRECTION('',(1.66533453693773E-16,1.,1.1518563880486E-15));
#11932=DIRECTION('center_axis',(1.66533453693773E-16,1.,1.1518563880486E-15));
#11933=DIRECTION('ref_axis',(1.,-1.66533453693753E-16,-1.72407814243868E-14));
#11934=DIRECTION('',(1.66533453693773E-16,1.,1.1518563880486E-15));
#11935=DIRECTION('center_axis',(1.66533453693773E-16,1.,1.1518563880486E-15));
#11936=DIRECTION('ref_axis',(1.,-1.66533453693753E-16,-1.72407814243868E-14));
#11937=DIRECTION('',(1.66533453693773E-16,1.,1.1518563880486E-15));
#11938=DIRECTION('center_axis',(1.66533453693773E-16,1.,1.1518563880486E-15));
#11939=DIRECTION('ref_axis',(1.,-1.66533453693753E-16,-1.72407814243868E-14));
#11940=DIRECTION('',(1.66533453693773E-16,1.,1.1518563880486E-15));
#11941=DIRECTION('center_axis',(1.66533453693773E-16,1.,1.1518563880486E-15));
#11942=DIRECTION('ref_axis',(1.,-1.66533453686288E-16,-6.49812218125261E-12));
#11943=DIRECTION('center_axis',(1.66533453693773E-16,1.,1.1518563880486E-15));
#11944=DIRECTION('ref_axis',(1.,-1.66533453693706E-16,-5.82535567993926E-14));
#11945=DIRECTION('',(1.66533453693773E-16,1.,1.1518563880486E-15));
#11946=DIRECTION('center_axis',(-1.66533453693773E-16,-1.,-1.1518563880486E-15));
#11947=DIRECTION('ref_axis',(1.,-1.66533453686241E-16,-6.53913495662739E-12));
#11948=DIRECTION('center_axis',(1.66533453693773E-16,1.,1.1518563880486E-15));
#11949=DIRECTION('ref_axis',(1.,-1.66533453693706E-16,-5.82535567993926E-14));
#11950=DIRECTION('',(1.66533453693773E-16,1.,1.1518563880486E-15));
#11951=DIRECTION('center_axis',(1.66533453693773E-16,1.,1.1518563880486E-15));
#11952=DIRECTION('ref_axis',(1.,-1.66533453693706E-16,-5.82535567993926E-14));
#11953=DIRECTION('',(1.66533453693773E-16,1.,1.1518563880486E-15));
#11954=DIRECTION('center_axis',(1.66533453693773E-16,1.,1.1518563880486E-15));
#11955=DIRECTION('ref_axis',(1.,-1.66533453693706E-16,-5.82535567993926E-14));
#11956=DIRECTION('',(1.66533453693773E-16,1.,1.1518563880486E-15));
#11957=DIRECTION('center_axis',(1.66533453693773E-16,1.,1.1518563880486E-15));
#11958=DIRECTION('ref_axis',(1.,-1.66533453693706E-16,-5.82535567993926E-14));
#11959=DIRECTION('',(1.66533453693773E-16,1.,1.1518563880486E-15));
#11960=DIRECTION('center_axis',(1.66533453693773E-16,1.,1.1518563880486E-15));
#11961=DIRECTION('ref_axis',(1.,-1.66533453693706E-16,-5.82535567993926E-14));
#11962=DIRECTION('',(1.66533453693773E-16,1.,1.1518563880486E-15));
#11963=DIRECTION('center_axis',(1.66533453693773E-16,1.,1.1518563880486E-15));
#11964=DIRECTION('ref_axis',(1.,-1.66533453693706E-16,-5.82535567993926E-14));
#11965=DIRECTION('',(1.66533453693773E-16,1.,1.1518563880486E-15));
#11966=DIRECTION('center_axis',(1.66533453693773E-16,1.,1.1518563880486E-15));
#11967=DIRECTION('ref_axis',(1.,-1.66533453693706E-16,-5.82535567993926E-14));
#11968=DIRECTION('',(1.66533453693773E-16,1.,1.1518563880486E-15));
#11969=DIRECTION('center_axis',(1.66533453693773E-16,1.,1.1518563880486E-15));
#11970=DIRECTION('ref_axis',(1.,-1.66533453693706E-16,-5.82535567993926E-14));
#11971=DIRECTION('',(1.66533453693773E-16,1.,1.1518563880486E-15));
#11972=DIRECTION('center_axis',(1.66533453693773E-16,1.,1.1518563880486E-15));
#11973=DIRECTION('ref_axis',(1.,-1.66533453693706E-16,-5.82535567993926E-14));
#11974=DIRECTION('',(1.66533453693773E-16,1.,1.1518563880486E-15));
#11975=DIRECTION('center_axis',(1.66533453693773E-16,1.,1.1518563880486E-15));
#11976=DIRECTION('ref_axis',(1.,-1.66533453693706E-16,-5.82535567993926E-14));
#11977=DIRECTION('',(1.66533453693773E-16,1.,1.1518563880486E-15));
#11978=DIRECTION('center_axis',(1.66533453693773E-16,1.,1.1518563880486E-15));
#11979=DIRECTION('ref_axis',(1.,-1.66533453693706E-16,-5.82535567993926E-14));
#11980=DIRECTION('',(1.66533453693773E-16,1.,1.1518563880486E-15));
#11981=DIRECTION('center_axis',(1.66533453693773E-16,1.,1.1518563880486E-15));
#11982=DIRECTION('ref_axis',(1.,-1.66533453693706E-16,-5.82535567993926E-14));
#11983=DIRECTION('',(1.66533453693773E-16,1.,1.1518563880486E-15));
#11984=DIRECTION('center_axis',(1.66533453693773E-16,1.,1.1518563880486E-15));
#11985=DIRECTION('ref_axis',(1.,-1.66533453686241E-16,-6.53913495662739E-12));
#11986=DIRECTION('center_axis',(1.66533453693773E-16,1.,1.1518563880486E-15));
#11987=DIRECTION('ref_axis',(1.,-1.66533453693773E-16,2.77555756156287E-17));
#11988=DIRECTION('',(1.66533453693773E-16,1.,1.1518563880486E-15));
#11989=DIRECTION('center_axis',(1.66533453693773E-16,1.,1.1518563880486E-15));
#11990=DIRECTION('ref_axis',(1.,-1.66533453693773E-16,2.77555756156287E-17));
#11991=DIRECTION('',(1.66533453693773E-16,1.,1.1518563880486E-15));
#11992=DIRECTION('center_axis',(1.66533453693773E-16,1.,1.1518563880486E-15));
#11993=DIRECTION('ref_axis',(1.,-1.66533453693773E-16,2.77555756156287E-17));
#11994=DIRECTION('',(1.66533453693773E-16,1.,1.1518563880486E-15));
#11995=DIRECTION('center_axis',(1.66533453693773E-16,1.,1.1518563880486E-15));
#11996=DIRECTION('ref_axis',(1.,-1.66533453693773E-16,2.77555756156287E-17));
#11997=DIRECTION('',(1.66533453693773E-16,1.,1.1518563880486E-15));
#11998=DIRECTION('center_axis',(1.66533453693773E-16,1.,1.1518563880486E-15));
#11999=DIRECTION('ref_axis',(1.,-1.66533453693773E-16,2.77555756156287E-17));
#12000=DIRECTION('',(1.66533453693773E-16,1.,1.1518563880486E-15));
#12001=DIRECTION('center_axis',(1.66533453693773E-16,1.,1.1518563880486E-15));
#12002=DIRECTION('ref_axis',(1.,-1.66533453693773E-16,2.77555756156287E-17));
#12003=DIRECTION('',(1.66533453693773E-16,1.,1.1518563880486E-15));
#12004=DIRECTION('center_axis',(1.66533453693773E-16,1.,1.1518563880486E-15));
#12005=DIRECTION('ref_axis',(1.,-1.66533453693773E-16,2.77555756156287E-17));
#12006=DIRECTION('',(1.66533453693773E-16,1.,1.1518563880486E-15));
#12007=DIRECTION('center_axis',(1.66533453693773E-16,1.,1.1518563880486E-15));
#12008=DIRECTION('ref_axis',(1.,-1.66533453693773E-16,2.77555756156287E-17));
#12009=DIRECTION('center_axis',(1.66533453693773E-16,1.,1.1518563880486E-15));
#12010=DIRECTION('ref_axis',(1.,-1.66533453693773E-16,2.77555756156287E-17));
#12011=DIRECTION('',(1.66533453693773E-16,1.,1.1518563880486E-15));
#12012=DIRECTION('center_axis',(-1.66533453693773E-16,-1.,-1.1518563880486E-15));
#12013=DIRECTION('ref_axis',(1.,-1.66533453693773E-16,2.77555756156287E-17));
#12014=DIRECTION('center_axis',(1.66533453693773E-16,1.,1.1518563880486E-15));
#12015=DIRECTION('ref_axis',(1.,-1.66533453693773E-16,2.77555756156287E-17));
#12016=DIRECTION('',(1.66533453693773E-16,1.,1.1518563880486E-15));
#12017=DIRECTION('center_axis',(1.66533453693773E-16,1.,1.1518563880486E-15));
#12018=DIRECTION('ref_axis',(1.,-1.66533453693773E-16,2.77555756156287E-17));
#12019=DIRECTION('',(1.66533453693773E-16,1.,1.1518563880486E-15));
#12020=DIRECTION('center_axis',(1.66533453693773E-16,1.,1.1518563880486E-15));
#12021=DIRECTION('ref_axis',(1.,-1.66533453693773E-16,2.77555756156287E-17));
#12022=DIRECTION('',(1.66533453693773E-16,1.,1.1518563880486E-15));
#12023=DIRECTION('center_axis',(1.66533453693773E-16,1.,1.1518563880486E-15));
#12024=DIRECTION('ref_axis',(1.,-1.66533453693773E-16,2.77555756156287E-17));
#12025=DIRECTION('',(1.66533453693773E-16,1.,1.1518563880486E-15));
#12026=DIRECTION('center_axis',(1.66533453693773E-16,1.,1.1518563880486E-15));
#12027=DIRECTION('ref_axis',(1.,-1.66533453693773E-16,2.77555756156287E-17));
#12028=DIRECTION('',(1.66533453693773E-16,1.,1.1518563880486E-15));
#12029=DIRECTION('center_axis',(1.66533453693773E-16,1.,1.1518563880486E-15));
#12030=DIRECTION('ref_axis',(1.,-1.66533453693773E-16,2.77555756156287E-17));
#12031=DIRECTION('',(1.66533453693773E-16,1.,1.1518563880486E-15));
#12032=DIRECTION('center_axis',(1.66533453693773E-16,1.,1.1518563880486E-15));
#12033=DIRECTION('ref_axis',(1.,-1.66533453693773E-16,2.77555756156287E-17));
#12034=DIRECTION('',(1.66533453693773E-16,1.,1.1518563880486E-15));
#12035=DIRECTION('center_axis',(1.66533453693773E-16,1.,1.1518563880486E-15));
#12036=DIRECTION('ref_axis',(1.,-1.66533453693773E-16,2.77555756156287E-17));
#12037=DIRECTION('',(1.66533453693773E-16,1.,1.1518563880486E-15));
#12038=DIRECTION('center_axis',(1.66533453693773E-16,1.,1.1518563880486E-15));
#12039=DIRECTION('ref_axis',(1.,-1.66533453693773E-16,2.77555756156287E-17));
#12040=DIRECTION('',(1.66533453693773E-16,1.,1.1518563880486E-15));
#12041=DIRECTION('center_axis',(1.66533453693773E-16,1.,1.1518563880486E-15));
#12042=DIRECTION('ref_axis',(1.,-1.66533453693773E-16,2.77555756156287E-17));
#12043=DIRECTION('',(1.66533453693773E-16,1.,1.1518563880486E-15));
#12044=DIRECTION('center_axis',(1.66533453693773E-16,1.,1.1518563880486E-15));
#12045=DIRECTION('ref_axis',(1.,-1.66533453693773E-16,2.77555756156287E-17));
#12046=DIRECTION('',(1.66533453693773E-16,1.,1.1518563880486E-15));
#12047=DIRECTION('center_axis',(1.66533453693773E-16,1.,1.1518563880486E-15));
#12048=DIRECTION('ref_axis',(1.,-1.66533453693773E-16,2.77555756156287E-17));
#12049=DIRECTION('center_axis',(1.66533453693773E-16,1.,1.1518563880486E-15));
#12050=DIRECTION('ref_axis',(1.,-1.66533453693773E-16,2.77555756156287E-17));
#12051=DIRECTION('center_axis',(1.66533453693773E-16,1.,1.1518563880486E-15));
#12052=DIRECTION('ref_axis',(1.,-1.66533453693773E-16,2.77555756156287E-17));
#12053=DIRECTION('center_axis',(-1.,2.96593211435634E-32,-2.77555756156289E-17));
#12054=DIRECTION('ref_axis',(-2.3111159332647E-33,1.,1.1518563880486E-15));
#12055=DIRECTION('',(-1.66533453693773E-16,-1.,-1.1518563880486E-15));
#12056=DIRECTION('',(2.77555756156289E-17,1.1518563880486E-15,-1.));
#12057=DIRECTION('',(1.66533453693773E-16,1.,1.1518563880486E-15));
#12058=DIRECTION('',(2.77555756156289E-17,1.1518563880486E-15,-1.));
#12059=DIRECTION('center_axis',(-0.707106781186547,-0.707106781186548,-8.34111618675756E-16));
#12060=DIRECTION('ref_axis',(-0.707106781186548,0.707106781186547,7.94859307208661E-16));
#12061=DIRECTION('',(-0.707106781186548,0.707106781186547,7.94859307208661E-16));
#12062=DIRECTION('',(0.707106781186548,-0.707106781186547,-7.94859307208661E-16));
#12063=DIRECTION('',(-2.77555756156289E-17,-1.1518563880486E-15,1.));
#12064=DIRECTION('center_axis',(-0.707106781186548,8.14485462942207E-16,
-0.707106781186548));
#12065=DIRECTION('ref_axis',(8.32667268468875E-17,1.,1.06858966120171E-15));
#12066=DIRECTION('',(0.707106781186548,8.14485462942207E-16,-0.707106781186548));
#12067=DIRECTION('',(-1.66533453693773E-16,-1.,-1.1518563880486E-15));
#12068=DIRECTION('',(-0.707106781186548,-8.14485462942207E-16,0.707106781186548));
#12069=DIRECTION('center_axis',(-1.66533453693773E-16,-1.,-1.1518563880486E-15));
#12070=DIRECTION('ref_axis',(-2.77555756156289E-17,-1.1518563880486E-15,
1.));
#12071=DIRECTION('',(1.,-2.96593211435634E-32,2.77555756156289E-17));
#12072=DIRECTION('',(-0.707106781186547,8.14485462942209E-16,-0.707106781186548));
#12073=DIRECTION('',(-1.,2.96593211435634E-32,-2.77555756156289E-17));
#12074=DIRECTION('',(2.77555756156289E-17,1.1518563880486E-15,-1.));
#12075=DIRECTION('center_axis',(-1.66533453693773E-16,-1.,-1.1518563880486E-15));
#12076=DIRECTION('ref_axis',(1.,-1.66533453693773E-16,2.77555756156287E-17));
#12077=DIRECTION('center_axis',(-0.707106781186548,-8.14485462942208E-16,
0.707106781186547));
#12078=DIRECTION('ref_axis',(-0.707106781186547,8.14485462942209E-16,-0.707106781186548));
#12079=DIRECTION('',(0.707106781186547,-8.14485462942209E-16,0.707106781186548));
#12080=DIRECTION('',(1.66533453693773E-16,1.,1.1518563880486E-15));
#12081=DIRECTION('center_axis',(1.66533453693773E-16,1.,1.1518563880486E-15));
#12082=DIRECTION('ref_axis',(1.,-1.66533453693773E-16,2.77555756156287E-17));
#12083=DIRECTION('',(2.77555756156289E-17,1.1518563880486E-15,-1.));
#12084=DIRECTION('',(1.,-2.96593211435634E-32,2.77555756156289E-17));
#12085=DIRECTION('',(-1.,2.96593211435634E-32,-2.77555756156289E-17));
#12086=DIRECTION('',(2.77555756156289E-17,1.1518563880486E-15,-1.));
#12087=DIRECTION('center_axis',(-1.66533453693773E-16,-1.,-1.1518563880486E-15));
#12088=DIRECTION('ref_axis',(1.,-1.66533453693773E-16,2.77555756156287E-17));
#12089=DIRECTION('center_axis',(-1.66533453693773E-16,-1.,-1.1518563880486E-15));
#12090=DIRECTION('ref_axis',(1.,-1.66533453693773E-16,2.77555756156287E-17));
#12091=DIRECTION('center_axis',(-1.66533453693773E-16,-1.,-1.1518563880486E-15));
#12092=DIRECTION('ref_axis',(1.,-1.66533453693773E-16,2.77555756156287E-17));
#12093=DIRECTION('center_axis',(-1.66533453693773E-16,-1.,-1.1518563880486E-15));
#12094=DIRECTION('ref_axis',(1.,-1.66533453693773E-16,2.77555756156287E-17));
#12095=DIRECTION('center_axis',(-0.577350269189626,-0.577350269189625,-0.577350269189627));
#12096=DIRECTION('ref_axis',(-0.707106781186547,0.707106781186548,6.63491932426099E-16));
#12097=DIRECTION('',(1.3738309013483E-16,0.707106781186548,-0.707106781186547));
#12098=DIRECTION('center_axis',(-0.577350269189626,-0.577350269189627,0.577350269189625));
#12099=DIRECTION('ref_axis',(1.073776216497E-16,0.707106781186546,0.707106781186549));
#12100=DIRECTION('',(-9.81307786677355E-17,-0.707106781186546,-0.707106781186549));
#12101=DIRECTION('center_axis',(2.77555756156289E-17,1.1518563880486E-15,
-1.));
#12102=DIRECTION('ref_axis',(1.,-2.96593211435634E-32,2.77555756156289E-17));
#12103=DIRECTION('center_axis',(2.77555756156289E-17,1.1518563880486E-15,
-1.));
#12104=DIRECTION('ref_axis',(1.,-2.96593211435634E-32,2.77555756156289E-17));
#12105=DIRECTION('',(1.66533453693773E-16,1.,1.1518563880486E-15));
#12106=DIRECTION('',(1.,-2.96593211435634E-32,2.77555756156289E-17));
#12107=DIRECTION('center_axis',(2.77555756156289E-17,1.1518563880486E-15,
-1.));
#12108=DIRECTION('ref_axis',(1.,-2.96593211435634E-32,2.77555756156289E-17));
#12109=DIRECTION('',(-1.,2.96593211435634E-32,-2.77555756156289E-17));
#12110=DIRECTION('',(-1.66533453693773E-16,-1.,-1.1518563880486E-15));
#12111=DIRECTION('',(-1.,2.96593211435634E-32,-2.77555756156289E-17));
#12112=DIRECTION('',(1.66533453693773E-16,1.,1.1518563880486E-15));
#12113=DIRECTION('center_axis',(2.77555756156289E-17,1.1518563880486E-15,
-1.));
#12114=DIRECTION('ref_axis',(1.,-2.96593211435634E-32,2.77555756156289E-17));
#12115=DIRECTION('center_axis',(1.66533453693773E-16,1.,1.1518563880486E-15));
#12116=DIRECTION('ref_axis',(1.,-1.66533453693773E-16,2.77555756156287E-17));
#12117=DIRECTION('center_axis',(1.66533453693773E-16,1.,1.1518563880486E-15));
#12118=DIRECTION('ref_axis',(1.,-1.66533453693773E-16,2.77555756156287E-17));
#12119=DIRECTION('',(1.66533453693773E-16,1.,1.1518563880486E-15));
#12120=DIRECTION('center_axis',(2.77555756156289E-17,1.1518563880486E-15,
-1.));
#12121=DIRECTION('ref_axis',(1.,-2.96593211435634E-32,2.77555756156289E-17));
#12122=DIRECTION('center_axis',(-2.77555756156289E-17,-1.1518563880486E-15,
1.));
#12123=DIRECTION('ref_axis',(1.,-2.96593211435634E-32,2.77555756156289E-17));
#12124=DIRECTION('center_axis',(2.77555756156289E-17,1.1518563880486E-15,
-1.));
#12125=DIRECTION('ref_axis',(1.,-2.96593211435634E-32,2.77555756156289E-17));
#12126=DIRECTION('',(2.77555756156289E-17,1.1518563880486E-15,-1.));
#12127=DIRECTION('center_axis',(-2.77555756156289E-17,-1.1518563880486E-15,
1.));
#12128=DIRECTION('ref_axis',(1.,-2.96593211435634E-32,2.77555756156289E-17));
#12129=DIRECTION('center_axis',(-2.77555756156289E-17,-1.1518563880486E-15,
1.));
#12130=DIRECTION('ref_axis',(1.,-2.96593211435634E-32,2.77555756156289E-17));
#12131=DIRECTION('center_axis',(-2.77555756156289E-17,-1.1518563880486E-15,
1.));
#12132=DIRECTION('ref_axis',(-1.66533453693773E-16,-1.,-1.1518563880486E-15));
#12133=DIRECTION('center_axis',(-2.77555756156289E-17,-1.1518563880486E-15,
1.));
#12134=DIRECTION('ref_axis',(1.,-2.96593211435634E-32,2.77555756156289E-17));
#12135=DIRECTION('',(-1.66533453693773E-16,-1.,-1.1518563880486E-15));
#12136=DIRECTION('',(1.,-2.96593211435634E-32,2.77555756156289E-17));
#12137=DIRECTION('',(1.66533453693773E-16,1.,1.1518563880486E-15));
#12138=DIRECTION('',(1.,-2.96593211435634E-32,2.77555756156289E-17));
#12139=DIRECTION('',(-1.,2.96593211435634E-32,-2.77555756156289E-17));
#12140=DIRECTION('',(-1.66533453693773E-16,-1.,-1.1518563880486E-15));
#12141=DIRECTION('center_axis',(-2.77555756156289E-17,-1.1518563880486E-15,
1.));
#12142=DIRECTION('ref_axis',(1.,-2.96593211435634E-32,2.77555756156289E-17));
#12143=DIRECTION('center_axis',(2.77555756156289E-17,1.1518563880486E-15,
-1.));
#12144=DIRECTION('ref_axis',(1.,-2.96593211435634E-32,2.77555756156289E-17));
#12145=DIRECTION('center_axis',(-1.66533453693773E-16,-1.,-1.1518563880486E-15));
#12146=DIRECTION('ref_axis',(1.,-1.66533453693773E-16,2.77555756156287E-17));
#12147=DIRECTION('',(-0.707106781186548,-0.707106781186547,-9.20707224299304E-16));
#12148=DIRECTION('center_axis',(-1.66533453693773E-16,-1.,-1.1518563880486E-15));
#12149=DIRECTION('ref_axis',(1.,-1.66533453693773E-16,2.77555756156287E-17));
#12150=DIRECTION('center_axis',(1.66533453693773E-16,1.,1.1518563880486E-15));
#12151=DIRECTION('ref_axis',(1.,-1.66533453693773E-16,2.77555756156287E-17));
#12152=DIRECTION('center_axis',(1.66533453693773E-16,1.,1.1518563880486E-15));
#12153=DIRECTION('ref_axis',(1.,-1.66533453693773E-16,2.77555756156287E-17));
#12154=DIRECTION('',(-0.707106781186548,-0.707106781186547,-9.20707224299304E-16));
#12155=DIRECTION('center_axis',(-1.66533453693773E-16,-1.,-1.1518563880486E-15));
#12156=DIRECTION('ref_axis',(1.,-1.66533453693773E-16,2.77555756156287E-17));
#12157=DIRECTION('center_axis',(1.66533453693773E-16,1.,1.1518563880486E-15));
#12158=DIRECTION('ref_axis',(1.,-1.66533453693773E-16,2.77555756156287E-17));
#12159=DIRECTION('',(-0.707106781186548,-0.707106781186547,-9.20707224299304E-16));
#12160=DIRECTION('center_axis',(0.707106781186547,-0.707106781186548,-7.94859307208662E-16));
#12161=DIRECTION('ref_axis',(-2.77555756156286E-17,-1.1518563880486E-15,
1.));
#12162=DIRECTION('',(0.707106781186548,0.707106781186547,8.34111618675755E-16));
#12163=DIRECTION('',(-2.77555756156289E-17,-1.1518563880486E-15,1.));
#12164=DIRECTION('',(-0.707106781186548,-0.707106781186547,-8.34111618675755E-16));
#12165=DIRECTION('center_axis',(-9.81307786677357E-17,-0.707106781186547,
-0.707106781186548));
#12166=DIRECTION('ref_axis',(-1.,8.32667268468865E-17,5.55111512312577E-17));
#12167=DIRECTION('',(-1.3738309013483E-16,-0.707106781186548,0.707106781186547));
#12168=DIRECTION('center_axis',(-1.3738309013483E-16,-0.707106781186549,
0.707106781186546));
#12169=DIRECTION('ref_axis',(9.81307786677355E-17,0.707106781186546,0.707106781186549));
#12170=DIRECTION('',(9.81307786677355E-17,0.707106781186546,0.707106781186549));
#12171=DIRECTION('center_axis',(0.707106781186548,8.14485462942207E-16,
-0.707106781186548));
#12172=DIRECTION('ref_axis',(-8.32667268468889E-17,-1.,-1.23512311489549E-15));
#12173=DIRECTION('',(0.707106781186548,-8.14485462942207E-16,0.707106781186548));
#12174=DIRECTION('',(-1.66533453693773E-16,-1.,-1.1518563880486E-15));
#12175=DIRECTION('',(-0.707106781186548,8.14485462942207E-16,-0.707106781186548));
#12176=DIRECTION('center_axis',(1.3738309013483E-16,0.707106781186549,-0.707106781186547));
#12177=DIRECTION('ref_axis',(1.,-8.32667268468867E-17,1.11022302462515E-16));
#12178=DIRECTION('',(9.81307786677356E-17,0.707106781186547,0.707106781186548));
#12179=DIRECTION('',(1.,-2.96593211435634E-32,2.77555756156289E-17));
#12180=DIRECTION('',(-9.81307786677356E-17,-0.707106781186547,-0.707106781186548));
#12181=DIRECTION('center_axis',(-0.707106781186548,8.14485462942207E-16,
-0.707106781186548));
#12182=DIRECTION('ref_axis',(8.32667268468875E-17,1.,1.06858966120171E-15));
#12183=DIRECTION('',(-0.707106781186548,-8.14485462942207E-16,0.707106781186548));
#12184=DIRECTION('',(1.66533453693773E-16,1.,1.1518563880486E-15));
#12185=DIRECTION('',(0.707106781186548,8.14485462942207E-16,-0.707106781186548));
#12186=DIRECTION('center_axis',(1.66533453693773E-16,1.,1.1518563880486E-15));
#12187=DIRECTION('ref_axis',(1.,-1.66533453693773E-16,2.77555756156287E-17));
#12188=DIRECTION('',(0.707106781186547,-8.14485462942209E-16,0.707106781186548));
#12189=DIRECTION('',(-2.77555756156289E-17,-1.1518563880486E-15,1.));
#12190=DIRECTION('center_axis',(2.77555756156289E-17,1.1518563880486E-15,
-1.));
#12191=DIRECTION('ref_axis',(1.,-2.96593211435634E-32,2.77555756156289E-17));
#12192=DIRECTION('center_axis',(-2.77555756156289E-17,-1.1518563880486E-15,
1.));
#12193=DIRECTION('ref_axis',(1.,-2.96593211435634E-32,2.77555756156289E-17));
#12194=DIRECTION('',(-0.707106781186547,9.01081068565758E-16,-0.707106781186548));
#12195=DIRECTION('center_axis',(0.707106781186547,-8.14485462942209E-16,
0.707106781186548));
#12196=DIRECTION('ref_axis',(-8.32667268468885E-17,-1.,-1.06858966120171E-15));
#12197=DIRECTION('',(0.707106781186548,8.14485462942208E-16,-0.707106781186547));
#12198=DIRECTION('',(1.66533453693773E-16,1.,1.1518563880486E-15));
#12199=DIRECTION('',(-0.707106781186548,-8.14485462942208E-16,0.707106781186547));
#12200=DIRECTION('center_axis',(-0.707106781186548,-8.14485462942208E-16,
0.707106781186547));
#12201=DIRECTION('ref_axis',(-0.707106781186547,8.14485462942209E-16,-0.707106781186548));
#12202=DIRECTION('',(-0.707106781186547,8.14485462942209E-16,-0.707106781186548));
#12203=DIRECTION('',(-1.66533453693773E-16,-1.,-1.1518563880486E-15));
#12204=DIRECTION('center_axis',(9.81307786677355E-17,0.707106781186547,
0.707106781186549));
#12205=DIRECTION('ref_axis',(-1.,8.32667268468864E-17,5.55111512312577E-17));
#12206=DIRECTION('',(1.3738309013483E-16,0.707106781186548,-0.707106781186547));
#12207=DIRECTION('',(-1.,2.96593211435634E-32,-2.77555756156289E-17));
#12208=DIRECTION('',(-1.3738309013483E-16,-0.707106781186548,0.707106781186547));
#12209=DIRECTION('center_axis',(-2.77555756156289E-17,-1.1518563880486E-15,
1.));
#12210=DIRECTION('ref_axis',(1.,-2.96593211435634E-32,2.77555756156289E-17));
#12211=DIRECTION('center_axis',(2.77555756156289E-17,1.1518563880486E-15,
-1.));
#12212=DIRECTION('ref_axis',(1.,-2.96593211435634E-32,2.77555756156289E-17));
#12213=DIRECTION('',(-0.707106781186548,-9.01081068565757E-16,0.707106781186547));
#12214=DIRECTION('center_axis',(1.66533453693773E-16,1.,1.1518563880486E-15));
#12215=DIRECTION('ref_axis',(1.,-1.66533453693773E-16,2.77555756156287E-17));
#12216=DIRECTION('center_axis',(-1.66533453693773E-16,-1.,-1.1518563880486E-15));
#12217=DIRECTION('ref_axis',(1.,-1.66533453693773E-16,2.77555756156287E-17));
#12218=DIRECTION('center_axis',(1.66533453693773E-16,1.,1.1518563880486E-15));
#12219=DIRECTION('ref_axis',(1.,-1.66533453693773E-16,2.77555756156287E-17));
#12220=DIRECTION('center_axis',(-3.33321305916122E-12,1.,1.15185639931397E-15));
#12221=DIRECTION('ref_axis',(1.,3.33321305916122E-12,-3.37956487043916E-12));
#12222=DIRECTION('center_axis',(1.66533453693773E-16,1.,1.1518563880486E-15));
#12223=DIRECTION('ref_axis',(1.,-1.66533453693773E-16,2.77555756156287E-17));
#12224=DIRECTION('center_axis',(0.577350269189626,-0.577350269189627,0.577350269189625));
#12225=DIRECTION('ref_axis',(-1.98170923120496E-17,0.707106781186546,0.707106781186549));
#12226=DIRECTION('center_axis',(1.,-2.96593211435634E-32,2.77555756156289E-17));
#12227=DIRECTION('ref_axis',(2.77555756156289E-17,1.1518563880486E-15,-1.));
#12228=DIRECTION('',(2.77555756156289E-17,1.1518563880486E-15,-1.));
#12229=DIRECTION('center_axis',(0.577350269189626,-0.577350269189625,-0.577350269189627));
#12230=DIRECTION('ref_axis',(-1.44988248207523E-16,-0.707106781186549,0.707106781186546));
#12231=DIRECTION('center_axis',(0.577350269189626,0.577350269189627,-0.577350269189625));
#12232=DIRECTION('ref_axis',(-1.073776216497E-16,-0.707106781186546,-0.707106781186549));
#12233=DIRECTION('',(-0.707106781186548,0.707106781186548,7.94859307208662E-16));
#12234=DIRECTION('center_axis',(1.66533453693773E-16,1.,1.1518563880486E-15));
#12235=DIRECTION('ref_axis',(1.,-1.66533453693773E-16,2.77555756156287E-17));
#12236=DIRECTION('',(-2.77555756156289E-17,-1.1518563880486E-15,1.));
#12237=DIRECTION('',(2.77555756156289E-17,1.1518563880486E-15,-1.));
#12238=DIRECTION('center_axis',(1.66533453693773E-16,1.,1.1518563880486E-15));
#12239=DIRECTION('ref_axis',(1.,-1.66533453693773E-16,2.77555756156287E-17));
#12240=DIRECTION('center_axis',(1.66533453693773E-16,1.,1.1518563880486E-15));
#12241=DIRECTION('ref_axis',(1.,-1.66533453693773E-16,2.77555756156287E-17));
#12242=DIRECTION('center_axis',(-0.577350269189626,0.577350269189627,-0.577350269189625));
#12243=DIRECTION('ref_axis',(0.707106781186548,0.707106781186547,7.17735637696692E-16));
#12244=DIRECTION('',(-0.707106781186548,-0.707106781186548,-8.34111618675754E-16));
#12245=DIRECTION('center_axis',(-1.,2.96593211435634E-32,-2.77555756156289E-17));
#12246=DIRECTION('ref_axis',(-2.3111159332647E-33,1.,1.1518563880486E-15));
#12247=DIRECTION('',(-2.77555756156289E-17,-1.1518563880486E-15,1.));
#12248=DIRECTION('center_axis',(1.66533453693773E-16,1.,1.1518563880486E-15));
#12249=DIRECTION('ref_axis',(1.,-1.66533453693706E-16,-5.82535567993926E-14));
#12250=DIRECTION('center_axis',(2.77555756156289E-17,1.1518563880486E-15,
-1.));
#12251=DIRECTION('ref_axis',(1.,-2.96593211435634E-32,2.77555756156289E-17));
#12252=DIRECTION('',(2.77555756156289E-17,1.1518563880486E-15,-1.));
#12253=DIRECTION('center_axis',(-0.0089256192300513,-0.714647716078422,
-0.699427605421215));
#12254=DIRECTION('ref_axis',(-0.0957941300462763,0.696849620500493,-0.710791172607677));
#12255=DIRECTION('',(2.77555756156289E-17,1.1518563880486E-15,-1.));
#12256=DIRECTION('center_axis',(-0.0044136154535447,-0.712446086579493,
0.701712971033166));
#12257=DIRECTION('ref_axis',(0.138109839253334,-0.69542932579062,-0.705197649692497));
#12258=DIRECTION('center_axis',(0.00217776971565482,-0.711046915342384,
0.703141195992062));
#12259=DIRECTION('ref_axis',(-0.164197556343665,-0.693853653920902,-0.701146396575909));
#12260=DIRECTION('',(-2.77555756156289E-17,-1.1518563880486E-15,1.));
#12261=DIRECTION('center_axis',(0.0157381824501623,-0.717295463101778,-0.696591363876105));
#12262=DIRECTION('ref_axis',(0.0401947273684774,0.69656836830124,-0.716363659166154));
#12263=DIRECTION('center_axis',(0.577350269189626,0.577350269189625,0.577350269189627));
#12264=DIRECTION('ref_axis',(5.74277188698721E-17,-0.707106781186549,0.707106781186546));
#12265=DIRECTION('',(0.707106781186548,-0.707106781186548,-7.94859307208662E-16));
#12266=DIRECTION('center_axis',(-0.577350269189626,0.577350269189625,0.577350269189627));
#12267=DIRECTION('ref_axis',(-0.707106781186548,7.32325096026742E-16,-0.707106781186547));
#12268=DIRECTION('',(0.707106781186548,0.707106781186548,8.34111618675754E-16));
#12269=DIRECTION('center_axis',(1.66533453693773E-16,1.,1.1518563880486E-15));
#12270=DIRECTION('ref_axis',(1.,-1.66533453693773E-16,2.77555756156287E-17));
#12271=DIRECTION('center_axis',(-1.66533453693773E-16,-1.,-1.1518563880486E-15));
#12272=DIRECTION('ref_axis',(1.,-1.66533453693773E-16,2.77555756156287E-17));
#12273=DIRECTION('',(-0.707106781186547,0.707106781186548,8.81454912832211E-16));
#12274=DIRECTION('center_axis',(-1.66533453693773E-16,-1.,-1.1518563880486E-15));
#12275=DIRECTION('ref_axis',(1.,-1.66533453693773E-16,2.77555756156287E-17));
#12276=DIRECTION('center_axis',(1.20274161001058E-16,1.,1.1518563880486E-15));
#12277=DIRECTION('ref_axis',(1.,-1.20274161001005E-16,-4.62315371170993E-14));
#12278=DIRECTION('center_axis',(3.33321305916122E-12,-1.,-1.15185639931397E-15));
#12279=DIRECTION('ref_axis',(1.,3.33321305916122E-12,-3.37956487043916E-12));
#12280=DIRECTION('center_axis',(1.66533453693773E-16,1.,1.1518563880486E-15));
#12281=DIRECTION('ref_axis',(1.,-1.66533453693753E-16,-1.72407814243868E-14));
#12282=DIRECTION('center_axis',(0.707106781186548,0.707106781186548,8.34111618675754E-16));
#12283=DIRECTION('ref_axis',(-2.77555756156281E-17,-1.1518563880486E-15,
1.));
#12284=DIRECTION('center_axis',(1.66533453693773E-16,1.,1.1518563880486E-15));
#12285=DIRECTION('ref_axis',(1.,-1.66533453693773E-16,2.77555756156287E-17));
#12286=DIRECTION('center_axis',(-1.66533453693773E-16,-1.,-1.1518563880486E-15));
#12287=DIRECTION('ref_axis',(1.,-1.66533453693773E-16,2.77555756156287E-17));
#12288=DIRECTION('',(-0.707106781186547,0.707106781186548,8.81454912832211E-16));
#12289=DIRECTION('center_axis',(-1.66533453693773E-16,-1.,-1.1518563880486E-15));
#12290=DIRECTION('ref_axis',(1.,-1.66533453693773E-16,2.77555756156287E-17));
#12291=DIRECTION('center_axis',(-0.707106781186548,0.707106781186548,7.94859307208662E-16));
#12292=DIRECTION('ref_axis',(2.77555756156286E-17,1.1518563880486E-15,-1.));
#12293=DIRECTION('center_axis',(1.66533453693773E-16,1.,1.1518563880486E-15));
#12294=DIRECTION('ref_axis',(1.,-1.66533453693773E-16,2.77555756156287E-17));
#12295=DIRECTION('center_axis',(1.66533453693773E-16,1.,1.1518563880486E-15));
#12296=DIRECTION('ref_axis',(1.,-1.66533453693753E-16,-1.72407814243868E-14));
#12297=DIRECTION('center_axis',(-1.66533453693773E-16,-1.,-1.1518563880486E-15));
#12298=DIRECTION('ref_axis',(1.,-1.66533453686288E-16,-6.49812218125261E-12));
#12299=DIRECTION('center_axis',(1.66533453693773E-16,1.,1.1518563880486E-15));
#12300=DIRECTION('ref_axis',(1.,-1.66533453693773E-16,2.77555756156287E-17));
#12301=DIRECTION('center_axis',(2.90775474051727E-9,-1.,-1.25901276750935E-9));
#12302=DIRECTION('ref_axis',(-0.245664236959599,5.0609894999909E-10,-0.969354982799933));
#12303=DIRECTION('center_axis',(1.66533453693773E-16,1.,1.1518563880486E-15));
#12304=DIRECTION('ref_axis',(1.,-1.66533453693773E-16,2.77555756156287E-17));
#12305=DIRECTION('center_axis',(1.66533453693773E-16,1.,1.1518563880486E-15));
#12306=DIRECTION('ref_axis',(1.,-1.66533453693753E-16,-1.72407814243868E-14));
#12307=DIRECTION('center_axis',(1.66533453693773E-16,1.,1.1518563880486E-15));
#12308=DIRECTION('ref_axis',(-0.987415940103716,3.46597824626892E-16,-0.158144747712638));
#12309=DIRECTION('center_axis',(1.66533453693773E-16,1.,1.1518563880486E-15));
#12310=DIRECTION('ref_axis',(-0.99782706232177,2.42064446342925E-16,-0.0658874320208806));
#12311=DIRECTION('center_axis',(1.66533453693773E-16,1.,1.1518563880486E-15));
#12312=DIRECTION('ref_axis',(1.,-1.66533453693773E-16,2.77555756156287E-17));
#12313=DIRECTION('center_axis',(1.66533453693773E-16,1.,1.1518563880486E-15));
#12314=DIRECTION('ref_axis',(1.,-1.66533453693773E-16,2.77555756156287E-17));
#12315=DIRECTION('axis',(0.,0.,1.));
#12316=DIRECTION('refdir',(1.,0.,0.));
#12317=DIRECTION('center_axis',(2.42833204006769E-16,2.41473507855972E-15,
-1.));
#12318=DIRECTION('ref_axis',(0.422618261740706,0.906307787036647,2.29111895189949E-15));
#12319=DIRECTION('center_axis',(3.62526098085663E-11,-1.69023416117786E-11,
-1.));
#12320=DIRECTION('ref_axis',(0.422618261740706,0.906307787036647,2.29111895186089E-15));
#12321=DIRECTION('',(-2.42833204006769E-16,-2.41473507855972E-15,1.));
#12322=DIRECTION('center_axis',(3.62526098085663E-11,-1.69023416117786E-11,
-1.));
#12323=DIRECTION('ref_axis',(0.422618261740706,0.906307787036647,2.29111895186089E-15));
#12324=DIRECTION('center_axis',(3.62526098085663E-11,-1.69023416117786E-11,
-1.));
#12325=DIRECTION('ref_axis',(0.422618261740706,0.906307787036647,2.29111895186089E-15));
#12326=DIRECTION('center_axis',(0.422618261740706,0.906307787036647,1.97116866169388E-15));
#12327=DIRECTION('ref_axis',(1.33440267382831E-16,2.1350442781253E-15,-1.));
#12328=DIRECTION('center_axis',(-0.422618261740706,-0.906307787036647,-1.97116866169388E-15));
#12329=DIRECTION('ref_axis',(3.8032634610719E-16,1.99759488807599E-15,-1.));
#12330=DIRECTION('center_axis',(0.906307787036647,-0.422618261740706,-8.00429517722823E-16));
#12331=DIRECTION('ref_axis',(0.422618261740706,0.906307787036647,1.97116866169388E-15));
#12332=DIRECTION('center_axis',(0.906307787036647,-0.422618261740706,-8.00429517722823E-16));
#12333=DIRECTION('ref_axis',(0.422618261740706,0.906307787036647,1.97116866169388E-15));
#12334=DIRECTION('center_axis',(0.906307787036647,-0.422618261740706,-8.00429517722823E-16));
#12335=DIRECTION('ref_axis',(0.422618261740706,0.906307787036647,1.97116866169388E-15));
#12336=DIRECTION('',(-0.906307787036647,0.422618261740706,8.00429517722823E-16));
#12337=DIRECTION('center_axis',(0.906307787036647,-0.422618261740706,-8.00429517722823E-16));
#12338=DIRECTION('ref_axis',(0.422618261740706,0.906307787036647,1.97116866169388E-15));
#12339=DIRECTION('center_axis',(2.98328550528607E-16,2.38885717348462E-15,
-1.));
#12340=DIRECTION('ref_axis',(0.906307787036647,-0.422618261740706,-7.39197177765454E-16));
#12341=DIRECTION('center_axis',(0.906307787036647,-0.422618261740706,-8.00429517722823E-16));
#12342=DIRECTION('ref_axis',(2.42833204006769E-16,2.41473507855972E-15,
-1.));
#12343=DIRECTION('axis',(0.,0.,1.));
#12344=DIRECTION('refdir',(1.,0.,0.));
#12345=DIRECTION('center_axis',(0.,1.,0.));
#12346=DIRECTION('ref_axis',(-1.,0.,5.99795050356438E-14));
#12347=DIRECTION('center_axis',(0.00224230328468888,0.997965773468312,0.0637125345734545));
#12348=DIRECTION('ref_axis',(0.997534176097042,0.0022370021927377,-0.0701467272193514));
#12349=DIRECTION('center_axis',(0.,1.,0.));
#12350=DIRECTION('ref_axis',(-1.,0.,4.05997950501941E-12));
#12351=DIRECTION('center_axis',(0.,-1.,0.));
#12352=DIRECTION('ref_axis',(-1.,0.,4.05997950501941E-12));
#12353=DIRECTION('center_axis',(0.,1.,0.));
#12354=DIRECTION('ref_axis',(-1.,0.,0.));
#12355=DIRECTION('center_axis',(0.,1.,0.));
#12356=DIRECTION('ref_axis',(-1.,0.,0.));
#12357=DIRECTION('center_axis',(0.,1.,0.));
#12358=DIRECTION('ref_axis',(-1.,0.,0.));
#12359=DIRECTION('center_axis',(0.,1.,0.));
#12360=DIRECTION('ref_axis',(1.,0.,1.24958540118864E-14));
#12361=DIRECTION('center_axis',(-0.00223920793173383,0.997967529966866,
-0.063685124477159));
#12362=DIRECTION('ref_axis',(-0.997538864914972,0.00223390431455718,0.0700801159792351));
#12363=DIRECTION('center_axis',(0.,1.,0.));
#12364=DIRECTION('ref_axis',(1.,0.,4.01249585399583E-12));
#12365=DIRECTION('center_axis',(0.,-1.,0.));
#12366=DIRECTION('ref_axis',(1.,0.,4.01249585399583E-12));
#12367=DIRECTION('center_axis',(0.,1.,0.));
#12368=DIRECTION('ref_axis',(1.,0.,0.));
#12369=DIRECTION('center_axis',(0.,1.,0.));
#12370=DIRECTION('ref_axis',(1.,0.,0.));
#12371=DIRECTION('center_axis',(0.,-1.,0.));
#12372=DIRECTION('ref_axis',(1.,0.,0.));
#12373=DIRECTION('center_axis',(0.,-1.,0.));
#12374=DIRECTION('ref_axis',(-1.,0.,0.));
#12375=DIRECTION('center_axis',(0.,1.,0.));
#12376=DIRECTION('ref_axis',(-1.,0.,0.));
#12377=DIRECTION('',(0.707106781186547,-0.707106781186548,8.65956056235493E-17));
#12378=DIRECTION('center_axis',(0.,-1.,0.));
#12379=DIRECTION('ref_axis',(-1.,0.,0.));
#12380=DIRECTION('center_axis',(0.,-1.,0.));
#12381=DIRECTION('ref_axis',(-1.,0.,0.));
#12382=DIRECTION('center_axis',(0.,-1.,0.));
#12383=DIRECTION('ref_axis',(-1.,0.,0.));
#12384=DIRECTION('',(0.,-1.,0.));
#12385=DIRECTION('center_axis',(0.,1.,0.));
#12386=DIRECTION('ref_axis',(1.,0.,0.));
#12387=DIRECTION('center_axis',(0.,1.,0.));
#12388=DIRECTION('ref_axis',(1.,0.,0.));
#12389=DIRECTION('center_axis',(0.,1.,0.));
#12390=DIRECTION('ref_axis',(-1.,0.,0.));
#12391=DIRECTION('center_axis',(0.,-1.,0.));
#12392=DIRECTION('ref_axis',(-1.,0.,0.));
#12393=DIRECTION('',(0.707106781186547,0.707106781186548,-8.65956056235493E-17));
#12394=DIRECTION('center_axis',(0.,1.,0.));
#12395=DIRECTION('ref_axis',(-1.,0.,0.));
#12396=DIRECTION('center_axis',(0.,1.,0.));
#12397=DIRECTION('ref_axis',(1.,0.,0.));
#12398=DIRECTION('center_axis',(0.,-1.,0.));
#12399=DIRECTION('ref_axis',(-1.,0.,0.));
#12400=DIRECTION('center_axis',(0.,-1.,0.));
#12401=DIRECTION('ref_axis',(-1.,0.,0.));
#12402=DIRECTION('',(0.,-1.,0.));
#12403=DIRECTION('center_axis',(0.,-1.,0.));
#12404=DIRECTION('ref_axis',(-1.,0.,0.));
#12405=DIRECTION('center_axis',(0.,1.,0.));
#12406=DIRECTION('ref_axis',(-1.,0.,0.));
#12407=DIRECTION('',(0.739940073395943,0.672672793996313,-9.061652424452E-17));
#12408=DIRECTION('center_axis',(0.,-1.,0.));
#12409=DIRECTION('ref_axis',(-1.,0.,0.));
#12410=DIRECTION('center_axis',(0.,1.,0.));
#12411=DIRECTION('ref_axis',(-1.,0.,0.));
#12412=DIRECTION('',(-0.707106781186547,0.707106781186548,-8.65956056235493E-17));
#12413=DIRECTION('center_axis',(0.,1.,0.));
#12414=DIRECTION('ref_axis',(-1.,0.,0.));
#12415=DIRECTION('',(0.,-1.,0.));
#12416=DIRECTION('center_axis',(0.,-1.,0.));
#12417=DIRECTION('ref_axis',(-1.,0.,0.));
#12418=DIRECTION('center_axis',(0.,1.,0.));
#12419=DIRECTION('ref_axis',(1.,0.,0.));
#12420=DIRECTION('center_axis',(0.,1.,0.));
#12421=DIRECTION('ref_axis',(-1.,0.,0.));
#12422=DIRECTION('center_axis',(0.,1.,0.));
#12423=DIRECTION('ref_axis',(-1.,0.,0.));
#12424=DIRECTION('center_axis',(0.,-1.,0.));
#12425=DIRECTION('ref_axis',(-1.,0.,0.));
#12426=DIRECTION('',(-0.707106781186547,0.707106781186548,-8.65956056235493E-17));
#12427=DIRECTION('center_axis',(0.,-1.,0.));
#12428=DIRECTION('ref_axis',(-1.,0.,0.));
#12429=DIRECTION('center_axis',(0.,1.,0.));
#12430=DIRECTION('ref_axis',(1.,0.,0.));
#12431=DIRECTION('center_axis',(0.,1.,0.));
#12432=DIRECTION('ref_axis',(1.,0.,0.));
#12433=DIRECTION('center_axis',(0.,-1.,0.));
#12434=DIRECTION('ref_axis',(1.,0.,0.));
#12435=DIRECTION('center_axis',(0.,-1.,0.));
#12436=DIRECTION('ref_axis',(1.,0.,0.));
#12437=DIRECTION('center_axis',(0.,1.,0.));
#12438=DIRECTION('ref_axis',(1.,0.,0.));
#12439=DIRECTION('center_axis',(0.,-1.,0.));
#12440=DIRECTION('ref_axis',(-1.,0.,0.));
#12441=DIRECTION('center_axis',(0.,1.,0.));
#12442=DIRECTION('ref_axis',(1.,0.,0.));
#12443=DIRECTION('',(0.707106781186548,-0.707106781186547,-8.65956056235494E-17));
#12444=DIRECTION('center_axis',(0.,1.,0.));
#12445=DIRECTION('ref_axis',(1.,0.,0.));
#12446=DIRECTION('center_axis',(0.,1.,0.));
#12447=DIRECTION('ref_axis',(-1.,0.,0.));
#12448=DIRECTION('center_axis',(0.,1.,0.));
#12449=DIRECTION('ref_axis',(-1.,0.,0.));
#12450=DIRECTION('',(0.,-1.,0.));
#12451=DIRECTION('axis',(0.,0.,1.));
#12452=DIRECTION('refdir',(1.,0.,0.));
#12453=DIRECTION('center_axis',(-6.74488507274914E-15,1.49880108324396E-15,
-1.));
#12454=DIRECTION('ref_axis',(-0.173648177666927,-0.984807753012209,-3.04793925546002E-16));
#12455=DIRECTION('center_axis',(6.74488507274914E-15,-1.49880108324396E-15,
1.));
#12456=DIRECTION('ref_axis',(-0.173648177666927,-0.984807753012209,-3.04793925546002E-16));
#12457=DIRECTION('',(-0.122787803968966,-0.696364240320021,0.707106781186547));
#12458=DIRECTION('center_axis',(-6.74488507274914E-15,1.49880108324396E-15,
-1.));
#12459=DIRECTION('ref_axis',(-0.173648177666927,-0.984807753012209,-3.04793925546002E-16));
#12460=DIRECTION('center_axis',(-6.74488507274914E-15,1.49880108324396E-15,
-1.));
#12461=DIRECTION('ref_axis',(-0.173648177666927,-0.984807753012209,-3.04793925546002E-16));
#12462=DIRECTION('center_axis',(-6.74488507274914E-15,1.49880108324396E-15,
-1.));
#12463=DIRECTION('ref_axis',(-0.173648177666927,-0.984807753012209,-3.04793925546002E-16));
#12464=DIRECTION('',(6.74488507274914E-15,-1.49880108324396E-15,1.));
#12465=DIRECTION('center_axis',(-6.74488507274914E-15,1.49880108324396E-15,
-1.));
#12466=DIRECTION('ref_axis',(-0.173648177666927,-0.984807753012209,-3.04793925546002E-16));
#12467=DIRECTION('center_axis',(6.74488507274914E-15,-1.49880108324396E-15,
1.));
#12468=DIRECTION('ref_axis',(-0.173648177666927,-0.984807753012209,-3.04793925546002E-16));
#12469=DIRECTION('',(-0.122787803968975,-0.696364240320018,-0.707106781186548));
#12470=DIRECTION('center_axis',(6.74488507274914E-15,-1.49880108324396E-15,
1.));
#12471=DIRECTION('ref_axis',(-0.173648177666927,-0.984807753012209,-3.04793925546002E-16));
#12472=DIRECTION('center_axis',(-6.74488507274914E-15,1.49880108324396E-15,
-1.));
#12473=DIRECTION('ref_axis',(-0.173648177666927,-0.984807753012209,-3.04793925546002E-16));
#12474=DIRECTION('axis',(0.,0.,1.));
#12475=DIRECTION('refdir',(1.,0.,0.));
#12476=DIRECTION('center_axis',(0.,-1.,2.77555756156289E-17));
#12477=DIRECTION('ref_axis',(-1.,0.,0.));
#12478=DIRECTION('',(0.,1.,-2.77555756156289E-17));
#12479=DIRECTION('center_axis',(0.,1.,-2.77555756156289E-17));
#12480=DIRECTION('ref_axis',(1.,0.,0.));
#12481=DIRECTION('center_axis',(0.,-1.,2.77555756156289E-17));
#12482=DIRECTION('ref_axis',(-1.,0.,0.));
#12483=DIRECTION('',(0.,1.,-2.77555756156289E-17));
#12484=DIRECTION('center_axis',(0.,-1.,2.77555756156289E-17));
#12485=DIRECTION('ref_axis',(-1.,0.,0.));
#12486=DIRECTION('',(0.,1.,-2.77555756156289E-17));
#12487=DIRECTION('center_axis',(0.,-1.,2.77555756156289E-17));
#12488=DIRECTION('ref_axis',(-1.,0.,0.));
#12489=DIRECTION('',(0.,1.,-2.77555756156289E-17));
#12490=DIRECTION('center_axis',(0.,-1.,2.77555756156289E-17));
#12491=DIRECTION('ref_axis',(-1.,0.,0.));
#12492=DIRECTION('',(0.,1.,-2.77555756156289E-17));
#12493=DIRECTION('center_axis',(0.,-1.,2.77555756156289E-17));
#12494=DIRECTION('ref_axis',(-1.,0.,0.));
#12495=DIRECTION('',(0.,1.,-2.77555756156289E-17));
#12496=DIRECTION('center_axis',(0.,-1.,2.77555756156289E-17));
#12497=DIRECTION('ref_axis',(-1.,0.,0.));
#12498=DIRECTION('',(0.,1.,-2.77555756156289E-17));
#12499=DIRECTION('center_axis',(0.,-1.,2.77555756156289E-17));
#12500=DIRECTION('ref_axis',(-1.,0.,0.));
#12501=DIRECTION('center_axis',(0.,-1.,2.77555756156289E-17));
#12502=DIRECTION('ref_axis',(-1.,0.,0.));
#12503=DIRECTION('center_axis',(0.,-1.,2.77555756156289E-17));
#12504=DIRECTION('ref_axis',(-1.,0.,0.));
#12505=DIRECTION('center_axis',(0.,-1.,2.77555756156289E-17));
#12506=DIRECTION('ref_axis',(-1.,-6.24795276412959E-31,-2.251062219229E-14));
#12507=DIRECTION('center_axis',(0.,-1.,2.77555756156289E-17));
#12508=DIRECTION('ref_axis',(-1.,-1.39402673353861E-28,-5.02251062216718E-12));
#12509=DIRECTION('center_axis',(0.,1.,-2.77555756156289E-17));
#12510=DIRECTION('ref_axis',(-1.,-1.39402673353861E-28,-5.02251062216718E-12));
#12511=DIRECTION('center_axis',(0.,-1.,2.77555756156289E-17));
#12512=DIRECTION('ref_axis',(-1.,0.,0.));
#12513=DIRECTION('center_axis',(0.,-1.,2.77555756156289E-17));
#12514=DIRECTION('ref_axis',(1.,0.,0.));
#12515=DIRECTION('',(0.,-2.77555756156289E-17,-1.));
#12516=DIRECTION('',(-0.500000000000316,2.40370335797894E-17,0.866025403784256));
#12517=DIRECTION('',(0.866025403784258,-1.38777878078232E-17,-0.500000000000314));
#12518=DIRECTION('',(-1.,2.77670126733686E-29,1.0004120634318E-12));
#12519=DIRECTION('',(0.866025403784257,1.38777878078232E-17,0.500000000000315));
#12520=DIRECTION('',(-0.500000000000317,-2.40370335797894E-17,-0.866025403784255));
#12521=DIRECTION('',(0.,2.77555756156289E-17,1.));
#12522=DIRECTION('',(0.500000000000317,-2.40370335797894E-17,-0.866025403784256));
#12523=DIRECTION('',(-0.866025403784254,1.38777878078233E-17,0.50000000000032));
#12524=DIRECTION('',(1.,-2.77708250259577E-29,-1.00054941790939E-12));
#12525=DIRECTION('',(-0.866025403784253,-1.38777878078234E-17,-0.500000000000322));
#12526=DIRECTION('',(0.500000000000318,2.40370335797894E-17,0.866025403784255));
#12527=DIRECTION('center_axis',(0.,1.,-2.77555756156289E-17));
#12528=DIRECTION('ref_axis',(-1.,0.,0.));
#12529=DIRECTION('',(-0.6,-0.8,9.56832684413443E-17));
#12530=DIRECTION('center_axis',(0.,-1.,2.77555756156289E-17));
#12531=DIRECTION('ref_axis',(-1.,0.,0.));
#12532=DIRECTION('center_axis',(0.707106781186548,-0.707106781186548,1.96261557335472E-17));
#12533=DIRECTION('ref_axis',(-5.8813528649299E-33,2.77555756156289E-17,
1.));
#12534=DIRECTION('',(0.447213595500212,0.447213595500212,0.77459666924119));
#12535=DIRECTION('',(0.,2.77555756156289E-17,1.));
#12536=DIRECTION('',(-0.447213595500212,-0.447213595500212,0.77459666924119));
#12537=DIRECTION('center_axis',(0.866025403784438,-1.38777878078144E-17,
-0.5));
#12538=DIRECTION('ref_axis',(-5.88504909690158E-32,1.,-2.77555756156289E-17));
#12539=DIRECTION('',(0.447213595500213,-0.447213595500208,0.774596669241192));
#12540=DIRECTION('',(0.,-1.,2.77555756156289E-17));
#12541=DIRECTION('',(-0.447213595500213,-0.447213595500208,-0.774596669241192));
#12542=DIRECTION('',(0.500000000000318,2.40370335797894E-17,0.866025403784255));
#12543=DIRECTION('',(-0.447213595500212,0.447213595500212,-0.77459666924119));
#12544=DIRECTION('',(0.,1.,-2.77555756156289E-17));
#12545=DIRECTION('center_axis',(-0.866025403781998,1.38777878079318E-17,
0.500000000004228));
#12546=DIRECTION('ref_axis',(0.500000000004228,2.40370335797268E-17,0.866025403781998));
#12547=DIRECTION('center_axis',(0.353553390593272,-0.707106781186546,0.612372435695797));
#12548=DIRECTION('ref_axis',(-0.86602540378444,1.41991444031354E-15,0.499999999999998));
#12549=DIRECTION('',(-0.44721359550021,0.447213595500215,0.774596669241189));
#12550=DIRECTION('',(-0.866025403784258,1.38777878078232E-17,0.500000000000314));
#12551=DIRECTION('',(-0.894427190999716,-0.447213595500357,1.00038097340813E-12));
#12552=DIRECTION('center_axis',(4.12063432796478E-16,2.77555756156289E-17,
1.));
#12553=DIRECTION('ref_axis',(0.,1.,-2.77555756156289E-17));
#12554=DIRECTION('',(0.,-1.,2.77555756156289E-17));
#12555=DIRECTION('',(0.894427190999716,-0.447213595500357,-1.0003561480666E-12));
#12556=DIRECTION('',(-1.,2.77670126733686E-29,1.0004120634318E-12));
#12557=DIRECTION('',(0.894427190999716,0.447213595500357,-1.00038097340813E-12));
#12558=DIRECTION('',(0.,1.,-2.77555756156289E-17));
#12559=DIRECTION('',(-0.894427190999716,0.447213595500357,1.0003561480666E-12));
#12560=DIRECTION('center_axis',(0.,-2.77555756156289E-17,-1.));
#12561=DIRECTION('ref_axis',(-1.,0.,0.));
#12562=DIRECTION('center_axis',(-0.353553390593273,-0.707106781186547,0.612372435695796));
#12563=DIRECTION('ref_axis',(-0.866025403784439,-7.69758259559516E-16,-0.499999999999999));
#12564=DIRECTION('',(-0.866025403784257,-1.38777878078232E-17,-0.500000000000315));
#12565=DIRECTION('',(-0.447213595500212,-0.447213595500213,-0.77459666924119));
#12566=DIRECTION('center_axis',(-0.707106781186548,-0.707106781186548,1.96261557335472E-17));
#12567=DIRECTION('ref_axis',(-5.8813528649299E-33,-2.77555756156289E-17,
-1.));
#12568=DIRECTION('',(-0.447213595500212,0.447213595500212,-0.77459666924119));
#12569=DIRECTION('',(0.,-2.77555756156289E-17,-1.));
#12570=DIRECTION('',(0.447213595500212,-0.447213595500212,-0.77459666924119));
#12571=DIRECTION('center_axis',(-0.866025403784439,-1.38777878078144E-17,
-0.5));
#12572=DIRECTION('ref_axis',(-5.58796234969744E-32,-1.,2.77555756156289E-17));
#12573=DIRECTION('',(0.,-1.,2.77555756156289E-17));
#12574=DIRECTION('',(-0.447213595500212,-0.447213595500212,0.77459666924119));
#12575=DIRECTION('',(0.500000000000317,-2.40370335797894E-17,-0.866025403784256));
#12576=DIRECTION('',(-0.447213595500212,0.44721359550021,0.774596669241191));
#12577=DIRECTION('',(0.,1.,-2.77555756156289E-17));
#12578=DIRECTION('',(0.447213595500212,0.44721359550021,-0.774596669241191));
#12579=DIRECTION('center_axis',(-0.353553390593276,-0.707106781186548,-0.612372435695793));
#12580=DIRECTION('ref_axis',(0.866025403784437,-1.39419548385453E-15,-0.500000000000002));
#12581=DIRECTION('',(0.866025403784254,-1.38777878078233E-17,-0.50000000000032));
#12582=DIRECTION('',(0.894427190999715,-0.44721359550036,-1.00047900164617E-12));
#12583=DIRECTION('center_axis',(0.353553390593277,-0.707106781186548,-0.612372435695793));
#12584=DIRECTION('ref_axis',(0.866025403784437,1.74380243674934E-15,0.500000000000003));
#12585=DIRECTION('',(0.894427190999714,0.447213595500361,-1.0005038269877E-12));
#12586=DIRECTION('',(0.866025403784253,1.38777878078234E-17,0.500000000000322));
#12587=DIRECTION('center_axis',(0.353553390593277,0.707106781186548,-0.612372435695793));
#12588=DIRECTION('ref_axis',(-0.894427190999914,0.447213595499961,1.25683885207554E-16));
#12589=DIRECTION('',(-0.866025403784253,-1.38777878078234E-17,-0.500000000000322));
#12590=DIRECTION('',(-0.894427190999714,0.447213595500361,1.00047900164617E-12));
#12591=DIRECTION('',(0.866025403784253,1.38777878078234E-17,0.500000000000322));
#12592=DIRECTION('center_axis',(0.,-1.,2.77555756156289E-17));
#12593=DIRECTION('ref_axis',(1.,0.,0.));
#12594=DIRECTION('',(1.,-2.77708250259577E-29,-1.00054941790939E-12));
#12595=DIRECTION('',(0.866025403784254,-1.38777878078233E-17,-0.50000000000032));
#12596=DIRECTION('',(0.,-2.77555756156289E-17,-1.));
#12597=DIRECTION('',(-0.500000000000317,-2.40370335797894E-17,-0.866025403784255));
#12598=DIRECTION('',(-0.866025403784257,-1.38777878078232E-17,-0.500000000000315));
#12599=DIRECTION('',(-0.866025403784258,1.38777878078232E-17,0.500000000000314));
#12600=DIRECTION('',(-0.500000000000316,2.40370335797894E-17,0.866025403784256));
#12601=DIRECTION('',(0.,2.77555756156289E-17,1.));
#12602=DIRECTION('center_axis',(0.,1.,0.));
#12603=DIRECTION('ref_axis',(0.809016994374948,0.,0.587785252292472));
#12604=DIRECTION('center_axis',(-0.353553390593277,0.707106781186548,-0.612372435695793));
#12605=DIRECTION('ref_axis',(-0.894427190999914,-0.447213595499961,-7.92695080627049E-18));
#12606=DIRECTION('',(-0.894427190999715,-0.44721359550036,1.0005038269877E-12));
#12607=DIRECTION('',(-0.866025403784254,1.38777878078233E-17,0.50000000000032));
#12608=DIRECTION('center_axis',(-0.707106781186548,0.707106781186548,-1.96261557335472E-17));
#12609=DIRECTION('ref_axis',(-0.707106781186548,-0.707106781186548,1.96261557335472E-17));
#12610=DIRECTION('',(0.,2.77555756156289E-17,1.));
#12611=DIRECTION('',(0.447213595500212,0.447213595500212,0.77459666924119));
#12612=DIRECTION('center_axis',(-0.353553390593273,0.707106781186547,0.612372435695796));
#12613=DIRECTION('ref_axis',(2.2218001674842E-16,-0.654653670707978,0.755928946018454));
#12614=DIRECTION('',(0.447213595500212,-0.447213595500213,0.77459666924119));
#12615=DIRECTION('',(0.866025403784257,1.38777878078232E-17,0.500000000000315));
#12616=DIRECTION('center_axis',(0.353553390593272,0.707106781186546,0.612372435695797));
#12617=DIRECTION('ref_axis',(1.93047492713039E-16,-0.65465367070798,0.755928946018453));
#12618=DIRECTION('',(0.866025403784258,-1.38777878078232E-17,-0.500000000000314));
#12619=DIRECTION('',(0.44721359550021,0.447213595500215,-0.774596669241189));
#12620=DIRECTION('center_axis',(0.866025403784439,1.38777878078144E-17,
0.5));
#12621=DIRECTION('ref_axis',(5.58796234969744E-32,1.,-2.77555756156289E-17));
#12622=DIRECTION('',(0.,-1.,2.77555756156289E-17));
#12623=DIRECTION('',(0.447213595500212,-0.447213595500212,-0.77459666924119));
#12624=DIRECTION('',(0.,1.,-2.77555756156289E-17));
#12625=DIRECTION('center_axis',(-0.866025403781999,-1.38777878079317E-17,
-0.500000000004226));
#12626=DIRECTION('ref_axis',(-0.500000000004226,2.40370335797268E-17,0.866025403781999));
#12627=DIRECTION('center_axis',(0.499999999999999,2.40370335797946E-17,
0.866025403784439));
#12628=DIRECTION('ref_axis',(-2.24770773560686E-32,1.,-2.77555756156289E-17));
#12629=DIRECTION('center_axis',(-0.499999999999999,2.40370335797946E-17,
0.866025403784439));
#12630=DIRECTION('ref_axis',(-0.866025403784439,-1.38777878078144E-17,-0.499999999999999));
#12631=DIRECTION('',(0.,-1.,2.77555756156289E-17));
#12632=DIRECTION('center_axis',(-0.866025403784439,1.38777878078144E-17,
0.5));
#12633=DIRECTION('ref_axis',(-0.5,-2.40370335797945E-17,-0.866025403784439));
#12634=DIRECTION('',(0.,1.,-2.77555756156289E-17));
#12635=DIRECTION('center_axis',(-1.,0.,0.));
#12636=DIRECTION('ref_axis',(0.,-2.77555756156289E-17,-1.));
#12637=DIRECTION('center_axis',(-0.500000000000001,-2.40370335797945E-17,
-0.866025403784438));
#12638=DIRECTION('ref_axis',(9.24446373305873E-33,-1.,2.77555756156289E-17));
#12639=DIRECTION('',(0.,-1.,2.77555756156289E-17));
#12640=DIRECTION('center_axis',(-1.65847312553218E-46,-2.77555756156292E-17,
-1.));
#12641=DIRECTION('ref_axis',(1.,-5.49417910395304E-16,1.52494103565577E-32));
#12642=DIRECTION('',(0.,1.,-2.77555756156289E-17));
#12643=DIRECTION('center_axis',(0.500000000000001,-2.40370335797945E-17,
-0.866025403784438));
#12644=DIRECTION('ref_axis',(9.24446373305873E-33,1.,-2.77555756156289E-17));
#12645=DIRECTION('center_axis',(0.707106781186548,0.707106781186548,-1.96261557335472E-17));
#12646=DIRECTION('ref_axis',(5.8813528649299E-33,2.77555756156289E-17,1.));
#12647=DIRECTION('',(0.,-2.77555756156289E-17,-1.));
#12648=DIRECTION('center_axis',(1.,0.,0.));
#12649=DIRECTION('ref_axis',(0.,-1.,2.77555756156289E-17));
#12650=DIRECTION('center_axis',(0.,2.77555756156289E-17,1.));
#12651=DIRECTION('ref_axis',(-1.,0.,0.));
#12652=DIRECTION('',(0.991227900682634,1.25058687706283E-16,0.132163720091021));
#12653=DIRECTION('center_axis',(0.866025403784439,1.38777878078144E-17,
0.5));
#12654=DIRECTION('ref_axis',(-0.5,2.40370335797945E-17,0.866025403784439));
#12655=DIRECTION('',(0.610071089398797,9.93983693090308E-17,-0.79234668288557));
#12656=DIRECTION('center_axis',(0.866025403784438,-1.38777878078144E-17,
-0.5));
#12657=DIRECTION('ref_axis',(0.5,2.40370335797945E-17,0.866025403784438));
#12658=DIRECTION('',(-0.381156811283838,9.57300891824016E-17,-0.92451040297659));
#12659=DIRECTION('center_axis',(0.,1.,-2.77555756156289E-17));
#12660=DIRECTION('ref_axis',(-1.,0.,0.));
#12661=DIRECTION('center_axis',(0.,-1.,2.77555756156289E-17));
#12662=DIRECTION('ref_axis',(-1.,0.,0.));
#12663=DIRECTION('',(0.316227766016838,0.948683298050514,-6.50579831597291E-17));
#12664=DIRECTION('center_axis',(0.,-1.,2.77555756156289E-17));
#12665=DIRECTION('ref_axis',(1.,0.,0.));
#12666=DIRECTION('center_axis',(0.,-1.,2.77555756156289E-17));
#12667=DIRECTION('ref_axis',(1.,0.,0.));
#12668=DIRECTION('center_axis',(0.,1.,-2.77555756156289E-17));
#12669=DIRECTION('ref_axis',(-1.,0.,0.));
#12670=DIRECTION('center_axis',(0.,1.,-2.77555756156289E-17));
#12671=DIRECTION('ref_axis',(-1.,0.,0.));
#12672=DIRECTION('',(0.,1.,-2.77555756156289E-17));
#12673=DIRECTION('center_axis',(0.,1.,-2.77555756156289E-17));
#12674=DIRECTION('ref_axis',(1.,0.,0.));
#12675=DIRECTION('center_axis',(0.,-1.,2.77555756156289E-17));
#12676=DIRECTION('ref_axis',(1.,0.,0.));
#12677=DIRECTION('',(-0.624695047554425,0.78086880944303,5.48296157566908E-17));
#12678=DIRECTION('center_axis',(0.,1.,-2.77555756156289E-17));
#12679=DIRECTION('ref_axis',(1.,0.,0.));
#12680=DIRECTION('center_axis',(0.,-1.,2.77555756156289E-17));
#12681=DIRECTION('ref_axis',(1.,0.,0.));
#12682=DIRECTION('center_axis',(0.,-1.,2.77555756156289E-17));
#12683=DIRECTION('ref_axis',(1.,0.,0.));
#12684=DIRECTION('center_axis',(0.,-1.,2.77555756156289E-17));
#12685=DIRECTION('ref_axis',(1.,0.,0.));
#12686=DIRECTION('',(0.,-1.,2.77555756156289E-17));
#12687=DIRECTION('center_axis',(0.,-1.,2.77555756156289E-17));
#12688=DIRECTION('ref_axis',(1.,0.,0.));
#12689=DIRECTION('center_axis',(0.,1.,-2.77555756156289E-17));
#12690=DIRECTION('ref_axis',(-1.,0.,0.));
#12691=DIRECTION('',(0.707106781186547,0.707106781186548,6.69694498900021E-17));
#12692=DIRECTION('center_axis',(0.,1.,-2.77555756156289E-17));
#12693=DIRECTION('ref_axis',(-1.,0.,0.));
#12694=DIRECTION('center_axis',(0.,-1.,2.77555756156289E-17));
#12695=DIRECTION('ref_axis',(1.,0.,0.));
#12696=DIRECTION('center_axis',(0.,-1.,2.77555756156289E-17));
#12697=DIRECTION('ref_axis',(1.,0.,0.));
#12698=DIRECTION('center_axis',(0.,-1.,2.77555756156289E-17));
#12699=DIRECTION('ref_axis',(1.,0.,0.));
#12700=DIRECTION('axis',(0.,0.,1.));
#12701=DIRECTION('refdir',(1.,0.,0.));
#12702=DIRECTION('center_axis',(2.22734643137795E-17,1.,1.11022302462516E-15));
#12703=DIRECTION('ref_axis',(-0.707106781186547,-7.69296511685101E-16,0.707106781186548));
#12704=DIRECTION('center_axis',(1.,2.77555756156289E-17,3.04610206107265E-32));
#12705=DIRECTION('ref_axis',(3.53858499469356E-34,-1.11022302462516E-15,
1.));
#12706=DIRECTION('center_axis',(-3.53858499469356E-34,1.11022302462516E-15,
-1.));
#12707=DIRECTION('ref_axis',(-2.22734643137795E-17,-1.,-1.11022302462516E-15));
#12708=DIRECTION('center_axis',(2.22734643137795E-17,1.,1.11022302462516E-15));
#12709=DIRECTION('ref_axis',(-0.707106781186547,-7.69296511685101E-16,0.707106781186548));
#12710=DIRECTION('center_axis',(1.,2.77555756156289E-17,3.04610206107265E-32));
#12711=DIRECTION('ref_axis',(1.96261557335472E-17,-0.707106781186549,0.707106781186546));
#12712=DIRECTION('center_axis',(-3.53858499469356E-34,1.11022302462516E-15,
-1.));
#12713=DIRECTION('ref_axis',(-2.22734643137795E-17,-1.,-1.11022302462516E-15));
#12714=DIRECTION('center_axis',(2.22734643137795E-17,1.,1.11022302462516E-15));
#12715=DIRECTION('ref_axis',(-1.,2.22734643137795E-17,2.50823714187942E-32));
#12716=DIRECTION('center_axis',(1.,2.77555756156289E-17,3.04610206107265E-32));
#12717=DIRECTION('ref_axis',(1.96261557335472E-17,-0.707106781186549,0.707106781186546));
#12718=DIRECTION('center_axis',(-3.53858499469356E-34,1.11022302462516E-15,
-1.));
#12719=DIRECTION('ref_axis',(-0.707106781186547,-0.707106781186547,-7.8504622934189E-16));
#12720=DIRECTION('center_axis',(2.22734643137795E-17,1.,1.11022302462516E-15));
#12721=DIRECTION('ref_axis',(-1.,2.22734643137795E-17,2.50823714187942E-32));
#12722=DIRECTION('center_axis',(-3.53858499469356E-34,1.11022302462516E-15,
-1.));
#12723=DIRECTION('ref_axis',(0.707106781186548,-0.707106781186547,-7.8504622934189E-16));
#12724=DIRECTION('center_axis',(-1.,-2.77555756156289E-17,-3.04610206107265E-32));
#12725=DIRECTION('ref_axis',(2.77555756156289E-17,-1.,-1.11022302462516E-15));
#12726=DIRECTION('center_axis',(2.22734643137795E-17,1.,1.11022302462516E-15));
#12727=DIRECTION('ref_axis',(3.53858499469358E-34,-1.11022302462516E-15,
1.));
#12728=DIRECTION('center_axis',(-3.53858499469356E-34,1.11022302462516E-15,
-1.));
#12729=DIRECTION('ref_axis',(0.707106781186548,-0.707106781186547,-7.8504622934189E-16));
#12730=DIRECTION('center_axis',(-1.,-2.77555756156289E-17,-3.04610206107265E-32));
#12731=DIRECTION('ref_axis',(1.96261557335472E-17,-0.707106781186549,0.707106781186546));
#12732=DIRECTION('center_axis',(2.22734643137795E-17,1.,1.11022302462516E-15));
#12733=DIRECTION('ref_axis',(3.53858499469358E-34,-1.11022302462516E-15,
1.));
#12734=DIRECTION('center_axis',(-3.53858499469356E-34,1.11022302462516E-15,
-1.));
#12735=DIRECTION('ref_axis',(1.,2.77555756156289E-17,3.04610206107265E-32));
#12736=DIRECTION('center_axis',(-1.,-2.77555756156289E-17,-3.04610206107265E-32));
#12737=DIRECTION('ref_axis',(1.96261557335472E-17,-0.707106781186549,0.707106781186546));
#12738=DIRECTION('center_axis',(2.22734643137795E-17,1.,1.11022302462516E-15));
#12739=DIRECTION('ref_axis',(0.707106781186548,-8.0079594699868E-16,0.707106781186547));
#12740=DIRECTION('center_axis',(-3.53858499469356E-34,1.11022302462516E-15,
-1.));
#12741=DIRECTION('ref_axis',(1.,2.77555756156289E-17,3.04610206107265E-32));
#12742=DIRECTION('center_axis',(1.,2.77555756156289E-17,3.04610206107265E-32));
#12743=DIRECTION('ref_axis',(1.96261557335472E-17,-0.707106781186546,-0.707106781186549));
#12744=DIRECTION('center_axis',(2.22734643137795E-17,1.,1.11022302462516E-15));
#12745=DIRECTION('ref_axis',(-3.53858499469358E-34,1.11022302462516E-15,
-1.));
#12746=DIRECTION('center_axis',(3.53858499469356E-34,-1.11022302462516E-15,
1.));
#12747=DIRECTION('ref_axis',(-1.,-2.77555756156289E-17,-3.04610206107265E-32));
#12748=DIRECTION('center_axis',(1.,2.77555756156289E-17,3.04610206107265E-32));
#12749=DIRECTION('ref_axis',(1.96261557335472E-17,-0.707106781186546,-0.707106781186549));
#12750=DIRECTION('center_axis',(2.22734643137795E-17,1.,1.11022302462516E-15));
#12751=DIRECTION('ref_axis',(-0.707106781186546,8.00795946998682E-16,-0.707106781186549));
#12752=DIRECTION('center_axis',(3.53858499469356E-34,-1.11022302462516E-15,
1.));
#12753=DIRECTION('ref_axis',(-1.,-2.77555756156289E-17,-3.04610206107265E-32));
#12754=DIRECTION('center_axis',(1.,2.77555756156289E-17,3.04610206107265E-32));
#12755=DIRECTION('ref_axis',(2.77555756156289E-17,-1.,-1.11022302462516E-15));
#12756=DIRECTION('center_axis',(2.22734643137795E-17,1.,1.11022302462516E-15));
#12757=DIRECTION('ref_axis',(-0.707106781186546,8.00795946998682E-16,-0.707106781186549));
#12758=DIRECTION('center_axis',(3.53858499469356E-34,-1.11022302462516E-15,
1.));
#12759=DIRECTION('ref_axis',(-0.707106781186547,-0.707106781186548,-7.85046229341891E-16));
#12760=DIRECTION('center_axis',(1.,2.77555756156289E-17,3.04610206107265E-32));
#12761=DIRECTION('ref_axis',(2.77555756156289E-17,-1.,-1.11022302462516E-15));
#12762=DIRECTION('center_axis',(3.53858499469356E-34,-1.11022302462516E-15,
1.));
#12763=DIRECTION('ref_axis',(0.707106781186549,-0.707106781186546,-7.85046229341888E-16));
#12764=DIRECTION('center_axis',(2.22734643137795E-17,1.,1.11022302462516E-15));
#12765=DIRECTION('ref_axis',(1.,-2.22734643137795E-17,-2.50823714187942E-32));
#12766=DIRECTION('center_axis',(-1.,-2.77555756156289E-17,-3.04610206107265E-32));
#12767=DIRECTION('ref_axis',(-3.53858499469356E-34,1.11022302462516E-15,
-1.));
#12768=DIRECTION('center_axis',(3.53858499469356E-34,-1.11022302462516E-15,
1.));
#12769=DIRECTION('ref_axis',(0.707106781186549,-0.707106781186546,-7.85046229341888E-16));
#12770=DIRECTION('center_axis',(2.22734643137795E-17,1.,1.11022302462516E-15));
#12771=DIRECTION('ref_axis',(0.707106781186548,7.692965116851E-16,-0.707106781186548));
#12772=DIRECTION('center_axis',(-1.,-2.77555756156289E-17,-3.04610206107265E-32));
#12773=DIRECTION('ref_axis',(-3.53858499469356E-34,1.11022302462516E-15,
-1.));
#12774=DIRECTION('center_axis',(3.53858499469356E-34,-1.11022302462516E-15,
1.));
#12775=DIRECTION('ref_axis',(-2.22734643137795E-17,-1.,-1.11022302462516E-15));
#12776=DIRECTION('center_axis',(2.22734643137795E-17,1.,1.11022302462516E-15));
#12777=DIRECTION('ref_axis',(0.707106781186548,7.692965116851E-16,-0.707106781186548));
#12778=DIRECTION('center_axis',(-1.,-2.77555756156289E-17,-3.04610206107265E-32));
#12779=DIRECTION('ref_axis',(1.96261557335472E-17,-0.707106781186548,-0.707106781186547));
#12780=DIRECTION('center_axis',(3.53858499469356E-34,-1.11022302462516E-15,
1.));
#12781=DIRECTION('ref_axis',(-2.22734643137795E-17,-1.,-1.11022302462516E-15));
#12782=DIRECTION('center_axis',(2.22734643137795E-17,1.,1.11022302462516E-15));
#12783=DIRECTION('ref_axis',(1.,-2.22734643137795E-17,-2.50823714187942E-32));
#12784=DIRECTION('center_axis',(-1.,-2.77555756156289E-17,-3.04610206107265E-32));
#12785=DIRECTION('ref_axis',(1.96261557335472E-17,-0.707106781186548,-0.707106781186547));
#12786=DIRECTION('center_axis',(-2.22734643137795E-17,-1.,-1.11022302462516E-15));
#12787=DIRECTION('ref_axis',(0.707106781186547,7.692965116851E-16,-0.707106781186547));
#12788=DIRECTION('center_axis',(-2.22734643137795E-17,-1.,-1.11022302462516E-15));
#12789=DIRECTION('ref_axis',(0.707106781186548,7.692965116851E-16,-0.707106781186548));
#12790=DIRECTION('',(-2.22734643137795E-17,-1.,-1.11022302462516E-15));
#12791=DIRECTION('',(2.22734643137795E-17,1.,1.11022302462516E-15));
#12792=DIRECTION('center_axis',(2.22734643137795E-17,1.,1.11022302462516E-15));
#12793=DIRECTION('ref_axis',(-3.53858499469358E-34,1.11022302462516E-15,
-1.));
#12794=DIRECTION('center_axis',(3.53858499469356E-34,-1.11022302462516E-15,
1.));
#12795=DIRECTION('ref_axis',(-0.707106781186547,-0.707106781186548,-7.85046229341891E-16));
#12796=DIRECTION('center_axis',(-2.22734643137795E-17,-1.,-1.11022302462516E-15));
#12797=DIRECTION('ref_axis',(-0.707106781186549,8.00795946998678E-16,-0.707106781186546));
#12798=DIRECTION('center_axis',(-2.22734643137795E-17,-1.,-1.11022302462516E-15));
#12799=DIRECTION('ref_axis',(-0.707106781186549,8.00795946998678E-16,-0.707106781186546));
#12800=DIRECTION('',(-2.22734643137795E-17,-1.,-1.11022302462516E-15));
#12801=DIRECTION('',(2.22734643137795E-17,1.,1.11022302462516E-15));
#12802=DIRECTION('center_axis',(1.,2.77555756156289E-17,3.04610206107265E-32));
#12803=DIRECTION('ref_axis',(1.96261557335472E-17,-0.707106781186548,-0.707106781186547));
#12804=DIRECTION('',(-1.,-2.77555756156289E-17,-3.04610206107265E-32));
#12805=DIRECTION('',(1.,2.77555756156289E-17,3.04610206107265E-32));
#12806=DIRECTION('center_axis',(-1.,-2.77555756156289E-17,-3.04610206107265E-32));
#12807=DIRECTION('ref_axis',(2.77555756156289E-17,-1.,-1.11022302462516E-15));
#12808=DIRECTION('center_axis',(2.22734643137795E-17,1.,1.11022302462516E-15));
#12809=DIRECTION('ref_axis',(0.707106781186548,-8.0079594699868E-16,0.707106781186547));
#12810=DIRECTION('center_axis',(-2.22734643137795E-17,-1.,-1.11022302462516E-15));
#12811=DIRECTION('ref_axis',(0.707106781186548,-8.0079594699868E-16,0.707106781186547));
#12812=DIRECTION('center_axis',(-2.22734643137795E-17,-1.,-1.11022302462516E-15));
#12813=DIRECTION('ref_axis',(0.707106781186548,-8.0079594699868E-16,0.707106781186547));
#12814=DIRECTION('',(-2.22734643137795E-17,-1.,-1.11022302462516E-15));
#12815=DIRECTION('',(2.22734643137795E-17,1.,1.11022302462516E-15));
#12816=DIRECTION('center_axis',(1.,2.77555756156289E-17,3.04610206107265E-32));
#12817=DIRECTION('ref_axis',(3.53858499469356E-34,-1.11022302462516E-15,
1.));
#12818=DIRECTION('center_axis',(-3.53858499469356E-34,1.11022302462516E-15,
-1.));
#12819=DIRECTION('ref_axis',(-0.707106781186547,-0.707106781186547,-7.8504622934189E-16));
#12820=DIRECTION('center_axis',(-2.22734643137795E-17,-1.,-1.11022302462516E-15));
#12821=DIRECTION('ref_axis',(-0.707106781186547,-7.69296511685101E-16,0.707106781186548));
#12822=DIRECTION('center_axis',(-2.22734643137795E-17,-1.,-1.11022302462516E-15));
#12823=DIRECTION('ref_axis',(-0.707106781186547,-7.69296511685101E-16,0.707106781186548));
#12824=DIRECTION('',(-2.22734643137795E-17,-1.,-1.11022302462516E-15));
#12825=DIRECTION('',(2.22734643137795E-17,1.,1.11022302462516E-15));
#12826=DIRECTION('center_axis',(-3.53858499469356E-34,1.11022302462516E-15,
-1.));
#12827=DIRECTION('ref_axis',(-0.707106781186547,-0.707106781186547,-7.8504622934189E-16));
#12828=DIRECTION('',(3.53858499469356E-34,-1.11022302462516E-15,1.));
#12829=DIRECTION('',(-3.53858499469356E-34,1.11022302462516E-15,-1.));
#12830=DIRECTION('center_axis',(-1.,-2.77555756156289E-17,-3.04610206107265E-32));
#12831=DIRECTION('ref_axis',(1.96261557335472E-17,-0.707106781186549,0.707106781186546));
#12832=DIRECTION('',(1.,2.77555756156289E-17,3.04610206107265E-32));
#12833=DIRECTION('',(-1.,-2.77555756156289E-17,-3.04610206107265E-32));
#12834=DIRECTION('center_axis',(3.53858499469356E-34,-1.11022302462516E-15,
1.));
#12835=DIRECTION('ref_axis',(0.707106781186549,-0.707106781186546,-7.85046229341888E-16));
#12836=DIRECTION('',(-3.53858499469356E-34,1.11022302462516E-15,-1.));
#12837=DIRECTION('',(3.53858499469356E-34,-1.11022302462516E-15,1.));
#12838=DIRECTION('center_axis',(-3.53858499469356E-34,1.11022302462516E-15,
-1.));
#12839=DIRECTION('ref_axis',(1.,2.77555756156289E-17,3.04610206107265E-32));
#12840=DIRECTION('',(-1.,-2.77555756156289E-17,-3.04610206107265E-32));
#12841=DIRECTION('',(-2.22734643137795E-17,-1.,-1.11022302462516E-15));
#12842=DIRECTION('center_axis',(3.53858499469356E-34,-1.11022302462516E-15,
1.));
#12843=DIRECTION('ref_axis',(1.,2.77555756156289E-17,3.04610206107265E-32));
#12844=DIRECTION('',(2.22734643137795E-17,1.,1.11022302462516E-15));
#12845=DIRECTION('',(-1.,-2.77555756156289E-17,-3.04610206107265E-32));
#12846=DIRECTION('',(2.22734643137795E-17,1.,1.11022302462516E-15));
#12847=DIRECTION('center_axis',(3.53858499469356E-34,-1.11022302462516E-15,
1.));
#12848=DIRECTION('ref_axis',(1.,2.77555756156289E-17,3.04610206107265E-32));
#12849=DIRECTION('',(2.22734643137795E-17,1.,1.11022302462516E-15));
#12850=DIRECTION('',(1.,2.77555756156289E-17,3.04610206107265E-32));
#12851=DIRECTION('center_axis',(2.22734643137795E-17,1.,1.11022302462516E-15));
#12852=DIRECTION('ref_axis',(1.,-2.22734643137795E-17,-2.50823714187942E-32));
#12853=DIRECTION('',(-3.53858499469356E-34,1.11022302462516E-15,-1.));
#12854=DIRECTION('',(1.,2.77555756156289E-17,3.04610206107265E-32));
#12855=DIRECTION('',(3.53858499469356E-34,-1.11022302462516E-15,1.));
#12856=DIRECTION('',(1.,2.77555756156289E-17,3.04610206107265E-32));
#12857=DIRECTION('',(-3.53858499469356E-34,1.11022302462516E-15,-1.));
#12858=DIRECTION('center_axis',(-1.,-2.77555756156289E-17,-3.04610206107265E-32));
#12859=DIRECTION('ref_axis',(-2.77555756156289E-17,1.,1.11022302462516E-15));
#12860=DIRECTION('',(-3.53858499469356E-34,1.11022302462516E-15,-1.));
#12861=DIRECTION('',(2.22734643137795E-17,1.,1.11022302462516E-15));
#12862=DIRECTION('',(3.53858499469356E-34,-1.11022302462516E-15,1.));
#12863=DIRECTION('',(2.22734643137795E-17,1.,1.11022302462516E-15));
#12864=DIRECTION('',(-3.53858499469356E-34,1.11022302462516E-15,-1.));
#12865=DIRECTION('',(2.22734643137795E-17,1.,1.11022302462516E-15));
#12866=DIRECTION('',(3.53858499469356E-34,-1.11022302462516E-15,1.));
#12867=DIRECTION('',(2.22734643137795E-17,1.,1.11022302462516E-15));
#12868=DIRECTION('center_axis',(2.22734643137795E-17,1.,1.11022302462516E-15));
#12869=DIRECTION('ref_axis',(1.,-2.22734643137795E-17,-2.50823714187942E-32));
#12870=DIRECTION('',(-1.,-2.77555756156289E-17,-3.04610206107265E-32));
#12871=DIRECTION('',(3.53858499469356E-34,-1.11022302462516E-15,1.));
#12872=DIRECTION('',(1.,2.77555756156289E-17,3.04610206107265E-32));
#12873=DIRECTION('',(3.53858499469356E-34,-1.11022302462516E-15,1.));
#12874=DIRECTION('',(-1.,-2.77555756156289E-17,-3.04610206107265E-32));
#12875=DIRECTION('center_axis',(2.22734643137795E-17,1.,1.11022302462516E-15));
#12876=DIRECTION('ref_axis',(1.,-2.22734643137795E-17,-2.50823714187942E-32));
#12877=DIRECTION('center_axis',(-2.22734643137795E-17,-1.,-1.11022302462516E-15));
#12878=DIRECTION('ref_axis',(1.,-2.22734643137795E-17,-2.50823714187942E-32));
#12879=DIRECTION('center_axis',(2.22734643137795E-17,1.,1.11022302462516E-15));
#12880=DIRECTION('ref_axis',(1.,-2.22734643137795E-17,-2.50823714187942E-32));
#12881=DIRECTION('center_axis',(-3.53858499469356E-34,1.11022302462516E-15,
-1.));
#12882=DIRECTION('ref_axis',(0.707106781186547,0.707106781186548,7.85046229341891E-16));
#12883=DIRECTION('center_axis',(3.53858499469356E-34,-1.11022302462516E-15,
1.));
#12884=DIRECTION('ref_axis',(0.707106781186547,0.707106781186548,7.85046229341891E-16));
#12885=DIRECTION('',(3.53858499469356E-34,-1.11022302462516E-15,1.));
#12886=DIRECTION('center_axis',(-3.53858499469356E-34,1.11022302462516E-15,
-1.));
#12887=DIRECTION('ref_axis',(0.707106781186547,0.707106781186548,7.85046229341891E-16));
#12888=DIRECTION('',(-3.53858499469356E-34,1.11022302462516E-15,-1.));
#12889=DIRECTION('center_axis',(2.22734643137795E-17,1.,1.11022302462516E-15));
#12890=DIRECTION('ref_axis',(1.,-2.22734643137795E-17,-2.50823714187942E-32));
#12891=DIRECTION('',(-1.,-2.77555756156289E-17,-3.04610206107265E-32));
#12892=DIRECTION('',(1.,2.77555756156289E-17,3.04610206107265E-32));
#12893=DIRECTION('center_axis',(-3.53858499469356E-34,1.11022302462516E-15,
-1.));
#12894=DIRECTION('ref_axis',(1.,2.77555756156289E-17,3.04610206107265E-32));
#12895=DIRECTION('',(2.22734643137795E-17,1.,1.11022302462516E-15));
#12896=DIRECTION('',(-1.,-2.77555756156289E-17,-3.04610206107265E-32));
#12897=DIRECTION('',(1.,2.77555756156289E-17,3.04610206107265E-32));
#12898=DIRECTION('center_axis',(-3.53858499469356E-34,1.11022302462516E-15,
-1.));
#12899=DIRECTION('ref_axis',(0.707106781186547,0.707106781186548,7.85046229341891E-16));
#12900=DIRECTION('center_axis',(3.53858499469356E-34,-1.11022302462516E-15,
1.));
#12901=DIRECTION('ref_axis',(0.707106781186547,0.707106781186548,7.85046229341891E-16));
#12902=DIRECTION('',(3.53858499469356E-34,-1.11022302462516E-15,1.));
#12903=DIRECTION('center_axis',(-3.53858499469356E-34,1.11022302462516E-15,
-1.));
#12904=DIRECTION('ref_axis',(0.707106781186547,0.707106781186548,7.85046229341891E-16));
#12905=DIRECTION('',(-3.53858499469356E-34,1.11022302462516E-15,-1.));
#12906=DIRECTION('center_axis',(2.22734643137795E-17,1.,1.11022302462516E-15));
#12907=DIRECTION('ref_axis',(1.,-2.22734643137795E-17,-2.50823714187942E-32));
#12908=DIRECTION('',(-1.,-2.77555756156289E-17,-3.04610206107265E-32));
#12909=DIRECTION('',(1.,2.77555756156289E-17,3.04610206107265E-32));
#12910=DIRECTION('center_axis',(-3.53858499469356E-34,1.11022302462516E-15,
-1.));
#12911=DIRECTION('ref_axis',(1.,2.77555756156289E-17,3.04610206107265E-32));
#12912=DIRECTION('',(2.22734643137795E-17,1.,1.11022302462516E-15));
#12913=DIRECTION('',(1.,2.77555756156289E-17,3.04610206107265E-32));
#12914=DIRECTION('center_axis',(1.,2.77555756156289E-17,3.04610206107265E-32));
#12915=DIRECTION('ref_axis',(-1.96261557335472E-17,0.707106781186547,0.707106781186549));
#12916=DIRECTION('center_axis',(-1.,-2.77555756156289E-17,-3.04610206107265E-32));
#12917=DIRECTION('ref_axis',(-1.96261557335472E-17,0.707106781186547,0.707106781186549));
#12918=DIRECTION('',(-1.,-2.77555756156289E-17,-3.04610206107265E-32));
#12919=DIRECTION('center_axis',(1.,2.77555756156289E-17,3.04610206107265E-32));
#12920=DIRECTION('ref_axis',(-1.96261557335472E-17,0.707106781186547,0.707106781186549));
#12921=DIRECTION('',(1.,2.77555756156289E-17,3.04610206107265E-32));
#12922=DIRECTION('center_axis',(-1.,-2.77555756156289E-17,-3.04610206107265E-32));
#12923=DIRECTION('ref_axis',(-2.77555756156289E-17,1.,1.11022302462516E-15));
#12924=DIRECTION('',(3.53858499469356E-34,-1.11022302462516E-15,1.));
#12925=DIRECTION('',(-3.53858499469356E-34,1.11022302462516E-15,-1.));
#12926=DIRECTION('',(2.22734643137795E-17,1.,1.11022302462516E-15));
#12927=DIRECTION('',(3.53858499469356E-34,-1.11022302462516E-15,1.));
#12928=DIRECTION('',(2.22734643137795E-17,1.,1.11022302462516E-15));
#12929=DIRECTION('center_axis',(2.22734643137795E-17,1.,1.11022302462516E-15));
#12930=DIRECTION('ref_axis',(1.,-2.22734643137795E-17,-2.50823714187942E-32));
#12931=DIRECTION('',(-3.53858499469356E-34,1.11022302462516E-15,-1.));
#12932=DIRECTION('center_axis',(-1.,-2.77555756156289E-17,-3.04610206107265E-32));
#12933=DIRECTION('ref_axis',(-1.96261557335472E-17,0.707106781186549,-0.707106781186546));
#12934=DIRECTION('center_axis',(1.,2.77555756156289E-17,3.04610206107265E-32));
#12935=DIRECTION('ref_axis',(-1.96261557335472E-17,0.707106781186549,-0.707106781186546));
#12936=DIRECTION('',(1.,2.77555756156289E-17,3.04610206107265E-32));
#12937=DIRECTION('center_axis',(-1.,-2.77555756156289E-17,-3.04610206107265E-32));
#12938=DIRECTION('ref_axis',(-1.96261557335472E-17,0.707106781186549,-0.707106781186546));
#12939=DIRECTION('',(-1.,-2.77555756156289E-17,-3.04610206107265E-32));
#12940=DIRECTION('center_axis',(1.,2.77555756156289E-17,3.04610206107265E-32));
#12941=DIRECTION('ref_axis',(-3.53858499469356E-34,1.11022302462516E-15,
-1.));
#12942=DIRECTION('',(-3.53858499469356E-34,1.11022302462516E-15,-1.));
#12943=DIRECTION('',(2.22734643137795E-17,1.,1.11022302462516E-15));
#12944=DIRECTION('',(3.53858499469356E-34,-1.11022302462516E-15,1.));
#12945=DIRECTION('',(2.22734643137795E-17,1.,1.11022302462516E-15));
#12946=DIRECTION('',(3.53858499469356E-34,-1.11022302462516E-15,1.));
#12947=DIRECTION('',(2.22734643137795E-17,1.,1.11022302462516E-15));
#12948=DIRECTION('center_axis',(2.22734643137795E-17,1.,1.11022302462516E-15));
#12949=DIRECTION('ref_axis',(1.,-2.22734643137795E-17,-2.50823714187942E-32));
#12950=DIRECTION('',(3.53858499469356E-34,-1.11022302462516E-15,1.));
#12951=DIRECTION('',(1.,2.77555756156289E-17,3.04610206107265E-32));
#12952=DIRECTION('center_axis',(3.53858499469356E-34,-1.11022302462516E-15,
1.));
#12953=DIRECTION('ref_axis',(-0.707106781186546,0.707106781186549,7.85046229341892E-16));
#12954=DIRECTION('center_axis',(-3.53858499469356E-34,1.11022302462516E-15,
-1.));
#12955=DIRECTION('ref_axis',(-0.707106781186546,0.707106781186549,7.85046229341892E-16));
#12956=DIRECTION('',(-3.53858499469356E-34,1.11022302462516E-15,-1.));
#12957=DIRECTION('center_axis',(3.53858499469356E-34,-1.11022302462516E-15,
1.));
#12958=DIRECTION('ref_axis',(-0.707106781186546,0.707106781186549,7.85046229341892E-16));
#12959=DIRECTION('',(3.53858499469356E-34,-1.11022302462516E-15,1.));
#12960=DIRECTION('center_axis',(2.22734643137795E-17,1.,1.11022302462516E-15));
#12961=DIRECTION('ref_axis',(1.,-2.22734643137795E-17,-2.50823714187942E-32));
#12962=DIRECTION('',(1.,2.77555756156289E-17,3.04610206107265E-32));
#12963=DIRECTION('',(-3.53858499469356E-34,1.11022302462516E-15,-1.));
#12964=DIRECTION('',(-1.,-2.77555756156289E-17,-3.04610206107265E-32));
#12965=DIRECTION('center_axis',(3.53858499469356E-34,-1.11022302462516E-15,
1.));
#12966=DIRECTION('ref_axis',(-2.22734643137795E-17,-1.,-1.11022302462516E-15));
#12967=DIRECTION('',(2.22734643137795E-17,1.,1.11022302462516E-15));
#12968=DIRECTION('',(-1.,-2.77555756156289E-17,-3.04610206107265E-32));
#12969=DIRECTION('',(-1.,-2.77555756156289E-17,-3.04610206107265E-32));
#12970=DIRECTION('',(2.22734643137795E-17,1.,1.11022302462516E-15));
#12971=DIRECTION('center_axis',(2.22734643137795E-17,1.,1.11022302462516E-15));
#12972=DIRECTION('ref_axis',(1.,-2.22734643137795E-17,-2.50823714187942E-32));
#12973=DIRECTION('',(-3.53858499469356E-34,1.11022302462516E-15,-1.));
#12974=DIRECTION('',(-3.53858499469356E-34,1.11022302462516E-15,-1.));
#12975=DIRECTION('',(1.,2.77555756156289E-17,3.04610206107265E-32));
#12976=DIRECTION('center_axis',(-1.,-2.77555756156289E-17,-3.04610206107265E-32));
#12977=DIRECTION('ref_axis',(-2.77555756156289E-17,1.,1.11022302462516E-15));
#12978=DIRECTION('',(2.22734643137795E-17,1.,1.11022302462516E-15));
#12979=DIRECTION('center_axis',(-3.53858499469356E-34,1.11022302462516E-15,
-1.));
#12980=DIRECTION('ref_axis',(1.,2.77555756156289E-17,3.04610206107265E-32));
#12981=DIRECTION('',(2.22734643137795E-17,1.,1.11022302462516E-15));
#12982=DIRECTION('',(1.,2.77555756156289E-17,3.04610206107265E-32));
#12983=DIRECTION('center_axis',(2.22734643137795E-17,1.,1.11022302462516E-15));
#12984=DIRECTION('ref_axis',(1.,-2.22734643137795E-17,-2.50823714187942E-32));
#12985=DIRECTION('',(3.53858499469356E-34,-1.11022302462516E-15,1.));
#12986=DIRECTION('',(-3.53858499469356E-34,1.11022302462516E-15,-1.));
#12987=DIRECTION('',(1.,2.77555756156289E-17,3.04610206107265E-32));
#12988=DIRECTION('',(3.53858499469356E-34,-1.11022302462516E-15,1.));
#12989=DIRECTION('',(1.,2.77555756156289E-17,3.04610206107265E-32));
#12990=DIRECTION('center_axis',(2.22734643137795E-17,1.,1.11022302462516E-15));
#12991=DIRECTION('ref_axis',(1.,-2.22734643137795E-17,-2.50823714187942E-32));
#12992=DIRECTION('',(-3.53858499469356E-34,1.11022302462516E-15,-1.));
#12993=DIRECTION('',(1.,2.77555756156289E-17,3.04610206107265E-32));
#12994=DIRECTION('',(-3.53858499469356E-34,1.11022302462516E-15,-1.));
#12995=DIRECTION('',(3.53858499469356E-34,-1.11022302462516E-15,1.));
#12996=DIRECTION('center_axis',(1.,2.77555756156289E-17,3.04610206107265E-32));
#12997=DIRECTION('ref_axis',(-3.53858499469356E-34,1.11022302462516E-15,
-1.));
#12998=DIRECTION('',(2.22734643137795E-17,1.,1.11022302462516E-15));
#12999=DIRECTION('',(-3.53858499469356E-34,1.11022302462516E-15,-1.));
#13000=DIRECTION('center_axis',(3.53858499469356E-34,-1.11022302462516E-15,
1.));
#13001=DIRECTION('ref_axis',(-2.22734643137795E-17,-1.,-1.11022302462516E-15));
#13002=DIRECTION('',(1.,2.77555756156289E-17,3.04610206107265E-32));
#13003=DIRECTION('center_axis',(2.22734643137795E-17,1.,1.11022302462516E-15));
#13004=DIRECTION('ref_axis',(1.,-2.22734643137795E-17,-2.50823714187942E-32));
#13005=DIRECTION('',(3.53858499469356E-34,-1.11022302462516E-15,1.));
#13006=DIRECTION('center_axis',(2.22734643137795E-17,1.,1.11022302462516E-15));
#13007=DIRECTION('ref_axis',(1.,-2.22734643137795E-17,-2.50823714187942E-32));
#13008=DIRECTION('',(3.53858499469356E-34,-1.11022302462516E-15,1.));
#13009=DIRECTION('',(-1.,-2.77555756156289E-17,-3.04610206107265E-32));
#13010=DIRECTION('center_axis',(-3.53858499469356E-34,1.11022302462516E-15,
-1.));
#13011=DIRECTION('ref_axis',(1.,2.77555756156289E-17,3.04610206107265E-32));
#13012=DIRECTION('',(1.,2.77555756156289E-17,3.04610206107265E-32));
#13013=DIRECTION('',(2.22734643137795E-17,1.,1.11022302462516E-15));
#13014=DIRECTION('center_axis',(2.22734643137795E-17,1.,1.11022302462516E-15));
#13015=DIRECTION('ref_axis',(1.,-2.22734643137795E-17,-2.50823714187942E-32));
#13016=DIRECTION('',(1.,2.77555756156289E-17,3.04610206107265E-32));
#13017=DIRECTION('',(-3.53858499469356E-34,1.11022302462516E-15,-1.));
#13018=DIRECTION('center_axis',(2.22734643137795E-17,1.,1.11022302462516E-15));
#13019=DIRECTION('ref_axis',(1.,-2.22734643137795E-17,-2.50823714187942E-32));
#13020=DIRECTION('',(3.53858499469356E-34,-1.11022302462516E-15,1.));
#13021=DIRECTION('',(3.53858499469356E-34,-1.11022302462516E-15,1.));
#13022=DIRECTION('',(-1.,-2.77555756156289E-17,-3.04610206107265E-32));
#13023=DIRECTION('center_axis',(1.,2.77555756156289E-17,3.04610206107265E-32));
#13024=DIRECTION('ref_axis',(-3.53858499469356E-34,1.11022302462516E-15,
-1.));
#13025=DIRECTION('',(2.22734643137795E-17,1.,1.11022302462516E-15));
#13026=DIRECTION('center_axis',(3.53858499469356E-34,-1.11022302462516E-15,
1.));
#13027=DIRECTION('ref_axis',(-2.22734643137795E-17,-1.,-1.11022302462516E-15));
#13028=DIRECTION('center_axis',(3.53858499469356E-34,-1.11022302462516E-15,
1.));
#13029=DIRECTION('ref_axis',(-2.22734643137795E-17,-1.,-1.11022302462516E-15));
#13030=DIRECTION('',(1.,2.77555756156289E-17,3.04610206107265E-32));
#13031=DIRECTION('',(2.22734643137795E-17,1.,1.11022302462516E-15));
#13032=DIRECTION('center_axis',(2.22734643137795E-17,1.,1.11022302462516E-15));
#13033=DIRECTION('ref_axis',(1.,-2.22734643137795E-17,-2.50823714187942E-32));
#13034=DIRECTION('',(1.,2.77555756156289E-17,3.04610206107265E-32));
#13035=DIRECTION('',(-3.53858499469356E-34,1.11022302462516E-15,-1.));
#13036=DIRECTION('center_axis',(2.22734643137795E-17,1.,1.11022302462516E-15));
#13037=DIRECTION('ref_axis',(1.,0.,0.));
#13038=DIRECTION('center_axis',(0.,1.11022302462516E-15,-1.));
#13039=DIRECTION('ref_axis',(-1.,0.,0.));
#13040=DIRECTION('center_axis',(-2.22734643137795E-17,-1.,-1.11022302462516E-15));
#13041=DIRECTION('ref_axis',(1.,-2.22734643137795E-17,-2.50823714187942E-32));
#13042=DIRECTION('center_axis',(-2.22734643137795E-17,-1.,-1.11022302462516E-15));
#13043=DIRECTION('ref_axis',(1.,-2.22734643137795E-17,-2.50823714187942E-32));
#13044=DIRECTION('center_axis',(-2.22734643137795E-17,-1.,-1.11022302462516E-15));
#13045=DIRECTION('ref_axis',(1.,-2.22734643137795E-17,-2.50823714187942E-32));
#13046=DIRECTION('',(-2.22734643137795E-17,-1.,-1.11022302462516E-15));
#13047=DIRECTION('center_axis',(2.22734643137795E-17,1.,1.11022302462516E-15));
#13048=DIRECTION('ref_axis',(1.,-2.22734643137795E-17,-2.50823714187942E-32));
#13049=DIRECTION('center_axis',(-2.22734643137795E-17,-1.,-1.11022302462516E-15));
#13050=DIRECTION('ref_axis',(3.53858499469358E-34,-1.11022302462516E-15,
1.));
#13051=DIRECTION('center_axis',(2.22734643137795E-17,1.,1.11022302462516E-15));
#13052=DIRECTION('ref_axis',(1.,-2.22734643137795E-17,-2.50823714187942E-32));
#13053=DIRECTION('center_axis',(-2.22734643137795E-17,-1.,-1.11022302462516E-15));
#13054=DIRECTION('ref_axis',(1.,-2.22734643137795E-17,-2.50823714187942E-32));
#13055=DIRECTION('',(-3.53858499469356E-34,1.11022302462516E-15,-1.));
#13056=DIRECTION('',(-1.,-2.77555756156289E-17,-3.04610206107265E-32));
#13057=DIRECTION('',(3.53858499469356E-34,-1.11022302462516E-15,1.));
#13058=DIRECTION('',(-1.,-2.77555756156289E-17,-3.04610206107265E-32));
#13059=DIRECTION('',(-3.53858499469356E-34,1.11022302462516E-15,-1.));
#13060=DIRECTION('center_axis',(-2.22734643137795E-17,-1.,-1.11022302462516E-15));
#13061=DIRECTION('ref_axis',(1.,-2.22734643137795E-17,-2.50823714187942E-32));
#13062=DIRECTION('',(-2.22734643137795E-17,-1.,-1.11022302462516E-15));
#13063=DIRECTION('center_axis',(1.,2.77555756156289E-17,3.04610206107265E-32));
#13064=DIRECTION('ref_axis',(-3.53858499469356E-34,1.11022302462516E-15,
-1.));
#13065=DIRECTION('',(-2.22734643137795E-17,-1.,-1.11022302462516E-15));
#13066=DIRECTION('',(-2.22734643137795E-17,-1.,-1.11022302462516E-15));
#13067=DIRECTION('center_axis',(1.,2.77555756156289E-17,3.04610206107265E-32));
#13068=DIRECTION('ref_axis',(-3.53858499469356E-34,1.11022302462516E-15,
-1.));
#13069=DIRECTION('center_axis',(3.53858499469356E-34,-1.11022302462516E-15,
1.));
#13070=DIRECTION('ref_axis',(-2.22734643137795E-17,-1.,-1.11022302462516E-15));
#13071=DIRECTION('',(-2.22734643137795E-17,-1.,-1.11022302462516E-15));
#13072=DIRECTION('center_axis',(3.53858499469356E-34,-1.11022302462516E-15,
1.));
#13073=DIRECTION('ref_axis',(1.,2.77555756156289E-17,3.04610206107265E-32));
#13074=DIRECTION('',(-2.22734643137795E-17,-1.,-1.11022302462516E-15));
#13075=DIRECTION('',(2.22734643137795E-17,1.,1.11022302462516E-15));
#13076=DIRECTION('',(2.22734643137795E-17,1.,1.11022302462516E-15));
#13077=DIRECTION('center_axis',(3.53858499469356E-34,-1.11022302462516E-15,
1.));
#13078=DIRECTION('ref_axis',(1.,2.77555756156289E-17,3.04610206107265E-32));
#13079=DIRECTION('center_axis',(1.,2.77555756156289E-17,3.04610206107265E-32));
#13080=DIRECTION('ref_axis',(-3.53858499469356E-34,1.11022302462516E-15,
-1.));
#13081=DIRECTION('',(-3.53858499469356E-34,1.11022302462516E-15,-1.));
#13082=DIRECTION('center_axis',(-3.53858499469356E-34,1.11022302462516E-15,
-1.));
#13083=DIRECTION('ref_axis',(1.,2.77555756156289E-17,3.04610206107265E-32));
#13084=DIRECTION('center_axis',(1.,2.77555756156289E-17,3.04610206107265E-32));
#13085=DIRECTION('ref_axis',(-3.53858499469356E-34,1.11022302462516E-15,
-1.));
#13086=DIRECTION('',(-3.53858499469356E-34,1.11022302462516E-15,-1.));
#13087=DIRECTION('center_axis',(-1.,-2.77555756156289E-17,-3.04610206107265E-32));
#13088=DIRECTION('ref_axis',(-2.77555756156289E-17,1.,1.11022302462516E-15));
#13089=DIRECTION('',(-3.53858499469356E-34,1.11022302462516E-15,-1.));
#13090=DIRECTION('center_axis',(-3.53858499469356E-34,1.11022302462516E-15,
-1.));
#13091=DIRECTION('ref_axis',(-1.2933087539066E-15,-1.,-1.11022302462516E-15));
#13092=DIRECTION('center_axis',(-1.,-2.77555756156289E-17,-3.04610206107265E-32));
#13093=DIRECTION('ref_axis',(-2.77555756156289E-17,1.,1.11022302462516E-15));
#13094=DIRECTION('',(2.22734643137795E-17,1.,1.11022302462516E-15));
#13095=DIRECTION('center_axis',(3.53858499469356E-34,-1.11022302462516E-15,
1.));
#13096=DIRECTION('ref_axis',(-1.98232732358613E-15,-1.,-1.11022302462516E-15));
#13097=DIRECTION('center_axis',(3.53858499469356E-34,-1.11022302462516E-15,
1.));
#13098=DIRECTION('ref_axis',(1.,2.77555756156289E-17,3.04610206107265E-32));
#13099=DIRECTION('center_axis',(-3.53858499469356E-34,1.11022302462516E-15,
-1.));
#13100=DIRECTION('ref_axis',(1.,2.77555756156289E-17,3.04610206107265E-32));
#13101=DIRECTION('',(3.53858499469356E-34,-1.11022302462516E-15,1.));
#13102=DIRECTION('center_axis',(-1.,-2.77555756156289E-17,-3.04610206107265E-32));
#13103=DIRECTION('ref_axis',(-2.77555756156289E-17,1.,1.11022302462516E-15));
#13104=DIRECTION('',(2.22734643137795E-17,1.,1.11022302462516E-15));
#13105=DIRECTION('',(-2.22734643137795E-17,-1.,-1.11022302462516E-15));
#13106=DIRECTION('center_axis',(1.,2.77555756156289E-17,3.04610206107265E-32));
#13107=DIRECTION('ref_axis',(-3.53858499469356E-34,1.11022302462516E-15,
-1.));
#13108=DIRECTION('',(2.22734643137795E-17,1.,1.11022302462516E-15));
#13109=DIRECTION('',(2.22734643137795E-17,1.,1.11022302462516E-15));
#13110=DIRECTION('',(3.53858499469356E-34,-1.11022302462516E-15,1.));
#13111=DIRECTION('center_axis',(3.53858499469356E-34,-1.11022302462516E-15,
1.));
#13112=DIRECTION('ref_axis',(1.,2.77555756156289E-17,3.04610206107265E-32));
#13113=DIRECTION('center_axis',(3.53858499469356E-34,-1.11022302462516E-15,
1.));
#13114=DIRECTION('ref_axis',(1.,2.77555756156289E-17,3.04610206107265E-32));
#13115=DIRECTION('center_axis',(-3.53858499469356E-34,1.11022302462516E-15,
-1.));
#13116=DIRECTION('ref_axis',(1.,2.77555756156289E-17,3.04610206107265E-32));
#13117=DIRECTION('',(3.53858499469356E-34,-1.11022302462516E-15,1.));
#13118=DIRECTION('center_axis',(-1.,-2.77555756156289E-17,-3.04610206107265E-32));
#13119=DIRECTION('ref_axis',(-2.77555756156289E-17,1.,1.11022302462516E-15));
#13120=DIRECTION('',(2.22734643137795E-17,1.,1.11022302462516E-15));
#13121=DIRECTION('',(2.22734643137795E-17,1.,1.11022302462516E-15));
#13122=DIRECTION('center_axis',(3.53858499469356E-34,-1.11022302462516E-15,
1.));
#13123=DIRECTION('ref_axis',(-2.22734643137795E-17,-1.,-1.11022302462516E-15));
#13124=DIRECTION('center_axis',(3.53858499469356E-34,-1.11022302462516E-15,
1.));
#13125=DIRECTION('ref_axis',(-2.22734643137795E-17,-1.,-1.11022302462516E-15));
#13126=DIRECTION('axis',(0.,0.,1.));
#13127=DIRECTION('refdir',(1.,0.,0.));
#13128=DIRECTION('center_axis',(-2.42833204006769E-16,-2.41473507855972E-15,
1.));
#13129=DIRECTION('ref_axis',(0.422618261740706,0.906307787036647,2.29111895189949E-15));
#13130=DIRECTION('center_axis',(2.42833204006769E-16,2.41473507855972E-15,
-1.));
#13131=DIRECTION('ref_axis',(0.422618261740706,0.906307787036647,2.29111895189949E-15));
#13132=DIRECTION('',(0.298836238730124,0.640856382055788,-0.707106781186546));
#13133=DIRECTION('center_axis',(-2.42833204006769E-16,-2.41473507855972E-15,
1.));
#13134=DIRECTION('ref_axis',(0.422618261740706,0.906307787036647,2.29111895189949E-15));
#13135=DIRECTION('center_axis',(-2.42833204006769E-16,-2.41473507855972E-15,
1.));
#13136=DIRECTION('ref_axis',(0.422618261740706,0.906307787036647,2.29111895189949E-15));
#13137=DIRECTION('center_axis',(-2.42833204006769E-16,-2.41473507855972E-15,
1.));
#13138=DIRECTION('ref_axis',(0.422618261740706,0.906307787036647,2.29111895189949E-15));
#13139=DIRECTION('',(2.42833204006769E-16,2.41473507855972E-15,-1.));
#13140=DIRECTION('center_axis',(-2.42833204006769E-16,-2.41473507855972E-15,
1.));
#13141=DIRECTION('ref_axis',(0.422618261740706,0.906307787036647,2.29111895189949E-15));
#13142=DIRECTION('center_axis',(-2.42833204006769E-16,-2.41473507855972E-15,
1.));
#13143=DIRECTION('ref_axis',(0.422618261740706,0.906307787036647,2.29111895189949E-15));
#13144=DIRECTION('axis',(0.,0.,1.));
#13145=DIRECTION('refdir',(1.,0.,0.));
#13146=DIRECTION('center_axis',(-5.55111512312578E-17,1.,-3.44969278837093E-14));
#13147=DIRECTION('ref_axis',(2.08166817117221E-16,3.44969278837093E-14,
1.));
#13148=DIRECTION('',(5.55111512312578E-17,-1.,3.44969278837093E-14));
#13149=DIRECTION('center_axis',(-5.55111512326456E-17,1.,-6.70116359450593E-12));
#13150=DIRECTION('ref_axis',(2.08166817116851E-16,6.70116359450593E-12,
1.));
#13151=DIRECTION('center_axis',(-5.55111512312578E-17,1.,-3.44969278837093E-14));
#13152=DIRECTION('ref_axis',(2.08166817117221E-16,3.44969278837093E-14,
1.));
#13153=DIRECTION('',(5.55111512312578E-17,-1.,3.44969278837093E-14));
#13154=DIRECTION('center_axis',(-5.55111512312578E-17,1.,-3.44969278837093E-14));
#13155=DIRECTION('ref_axis',(2.08166817117221E-16,3.44969278837093E-14,
1.));
#13156=DIRECTION('',(5.55111512312578E-17,-1.,3.44969278837093E-14));
#13157=DIRECTION('center_axis',(-5.55111512312578E-17,1.,-3.44969278837093E-14));
#13158=DIRECTION('ref_axis',(2.08166817117221E-16,3.44969278837093E-14,
1.));
#13159=DIRECTION('',(5.55111512312578E-17,-1.,3.44969278837093E-14));
#13160=DIRECTION('center_axis',(-5.55111512312578E-17,1.,-3.44969278837093E-14));
#13161=DIRECTION('ref_axis',(2.08166817117221E-16,3.44969278837093E-14,
1.));
#13162=DIRECTION('',(5.55111512312578E-17,-1.,3.44969278837093E-14));
#13163=DIRECTION('center_axis',(-5.55111512312578E-17,1.,-3.44969278837093E-14));
#13164=DIRECTION('ref_axis',(2.08166817117221E-16,3.44969278837093E-14,
1.));
#13165=DIRECTION('',(5.55111512312578E-17,-1.,3.44969278837093E-14));
#13166=DIRECTION('center_axis',(-5.55111512312578E-17,1.,-3.44969278837093E-14));
#13167=DIRECTION('ref_axis',(2.08166817117221E-16,3.44969278837093E-14,
1.));
#13168=DIRECTION('',(5.55111512312578E-17,-1.,3.44969278837093E-14));
#13169=DIRECTION('center_axis',(-5.55111512312578E-17,1.,-3.44969278837093E-14));
#13170=DIRECTION('ref_axis',(2.08166817117221E-16,3.44969278837093E-14,
1.));
#13171=DIRECTION('',(5.55111512312578E-17,-1.,3.44969278837093E-14));
#13172=DIRECTION('center_axis',(-5.55111512312578E-17,1.,-3.44969278837093E-14));
#13173=DIRECTION('ref_axis',(2.08166817117221E-16,3.44969278837093E-14,
1.));
#13174=DIRECTION('',(5.55111512312578E-17,-1.,3.44969278837093E-14));
#13175=DIRECTION('center_axis',(-5.55111512312578E-17,1.,-3.44969278837093E-14));
#13176=DIRECTION('ref_axis',(2.08166817117221E-16,3.44969278837093E-14,
1.));
#13177=DIRECTION('',(5.55111512312578E-17,-1.,3.44969278837093E-14));
#13178=DIRECTION('center_axis',(-5.55111512312578E-17,1.,-3.44969278837093E-14));
#13179=DIRECTION('ref_axis',(2.08166817117221E-16,3.44969278837093E-14,
1.));
#13180=DIRECTION('',(5.55111512312578E-17,-1.,3.44969278837093E-14));
#13181=DIRECTION('center_axis',(-5.55111512312578E-17,1.,-3.44969278837093E-14));
#13182=DIRECTION('ref_axis',(2.08166817117221E-16,3.44969278837093E-14,
1.));
#13183=DIRECTION('',(5.55111512312578E-17,-1.,3.44969278837093E-14));
#13184=DIRECTION('center_axis',(-5.55111512312578E-17,1.,-3.44969278837093E-14));
#13185=DIRECTION('ref_axis',(2.08166817117221E-16,3.44969278837093E-14,
1.));
#13186=DIRECTION('',(5.55111512312578E-17,-1.,3.44969278837093E-14));
#13187=DIRECTION('center_axis',(-5.55111512312578E-17,1.,-3.44969278837093E-14));
#13188=DIRECTION('ref_axis',(2.08166817117221E-16,3.44969278837093E-14,
1.));
#13189=DIRECTION('',(5.55111512312578E-17,-1.,3.44969278837093E-14));
#13190=DIRECTION('center_axis',(-5.55111512312578E-17,1.,-3.44969278837093E-14));
#13191=DIRECTION('ref_axis',(2.08166817117221E-16,3.44969278837093E-14,
1.));
#13192=DIRECTION('',(5.55111512312578E-17,-1.,3.44969278837093E-14));
#13193=DIRECTION('center_axis',(5.55111512312577E-17,-1.,3.39243069331623E-14));
#13194=DIRECTION('ref_axis',(-2.08166817117221E-16,-3.39243069331623E-14,
-1.));
#13195=DIRECTION('',(-5.55111512312577E-17,1.,-3.39243069331623E-14));
#13196=DIRECTION('center_axis',(8.50884136963852E-12,1.,-8.54339380881831E-12));
#13197=DIRECTION('ref_axis',(-8.51176958293838E-12,-8.54339380874589E-12,
-1.));
#13198=DIRECTION('center_axis',(5.55111512312577E-17,-1.,3.39243069331623E-14));
#13199=DIRECTION('ref_axis',(-2.08166817117221E-16,-3.39243069331623E-14,
-1.));
#13200=DIRECTION('',(-5.55111512312577E-17,1.,-3.39243069331623E-14));
#13201=DIRECTION('center_axis',(5.55111512312577E-17,-1.,3.39243069331623E-14));
#13202=DIRECTION('ref_axis',(-2.08166817117221E-16,-3.39243069331623E-14,
-1.));
#13203=DIRECTION('',(-5.55111512312577E-17,1.,-3.39243069331623E-14));
#13204=DIRECTION('center_axis',(5.55111512312577E-17,-1.,3.39243069331623E-14));
#13205=DIRECTION('ref_axis',(-2.08166817117221E-16,-3.39243069331623E-14,
-1.));
#13206=DIRECTION('',(-5.55111512312577E-17,1.,-3.39243069331623E-14));
#13207=DIRECTION('center_axis',(5.55111512312577E-17,-1.,3.39243069331623E-14));
#13208=DIRECTION('ref_axis',(-2.08166817117221E-16,-3.39243069331623E-14,
-1.));
#13209=DIRECTION('',(-5.55111512312577E-17,1.,-3.39243069331623E-14));
#13210=DIRECTION('center_axis',(5.55111512312577E-17,-1.,3.39243069331623E-14));
#13211=DIRECTION('ref_axis',(-2.08166817117221E-16,-3.39243069331623E-14,
-1.));
#13212=DIRECTION('',(-5.55111512312577E-17,1.,-3.39243069331623E-14));
#13213=DIRECTION('center_axis',(5.55111512312577E-17,-1.,3.39243069331623E-14));
#13214=DIRECTION('ref_axis',(-2.08166817117221E-16,-3.39243069331623E-14,
-1.));
#13215=DIRECTION('',(-5.55111512312577E-17,1.,-3.39243069331623E-14));
#13216=DIRECTION('center_axis',(5.55111512312577E-17,-1.,3.39243069331623E-14));
#13217=DIRECTION('ref_axis',(-2.08166817117221E-16,-3.39243069331623E-14,
-1.));
#13218=DIRECTION('',(-5.55111512312577E-17,1.,-3.39243069331623E-14));
#13219=DIRECTION('center_axis',(5.55111512312577E-17,-1.,3.39243069331623E-14));
#13220=DIRECTION('ref_axis',(-2.08166817117221E-16,-3.39243069331623E-14,
-1.));
#13221=DIRECTION('',(-5.55111512312577E-17,1.,-3.39243069331623E-14));
#13222=DIRECTION('center_axis',(5.55111512312577E-17,-1.,3.39243069331623E-14));
#13223=DIRECTION('ref_axis',(-2.08166817117221E-16,-3.39243069331623E-14,
-1.));
#13224=DIRECTION('',(-5.55111512312577E-17,1.,-3.39243069331623E-14));
#13225=DIRECTION('center_axis',(5.55111512312577E-17,-1.,3.39243069331623E-14));
#13226=DIRECTION('ref_axis',(-2.08166817117221E-16,-3.39243069331623E-14,
-1.));
#13227=DIRECTION('',(-5.55111512312577E-17,1.,-3.39243069331623E-14));
#13228=DIRECTION('center_axis',(5.55111512312577E-17,-1.,3.39243069331623E-14));
#13229=DIRECTION('ref_axis',(-2.08166817117221E-16,-3.39243069331623E-14,
-1.));
#13230=DIRECTION('',(-5.55111512312577E-17,1.,-3.39243069331623E-14));
#13231=DIRECTION('center_axis',(5.55111512312577E-17,-1.,3.39243069331623E-14));
#13232=DIRECTION('ref_axis',(-2.08166817117221E-16,-3.39243069331623E-14,
-1.));
#13233=DIRECTION('',(-5.55111512312577E-17,1.,-3.39243069331623E-14));
#13234=DIRECTION('center_axis',(5.55111512312577E-17,-1.,3.39243069331623E-14));
#13235=DIRECTION('ref_axis',(-2.08166817117221E-16,-3.39243069331623E-14,
-1.));
#13236=DIRECTION('',(-5.55111512312577E-17,1.,-3.39243069331623E-14));
#13237=DIRECTION('center_axis',(5.55111512312577E-17,-1.,3.39243069331623E-14));
#13238=DIRECTION('ref_axis',(-2.08166817117221E-16,-3.39243069331623E-14,
-1.));
#13239=DIRECTION('',(-5.55111512312577E-17,1.,-3.39243069331623E-14));
#13240=DIRECTION('center_axis',(5.55111512312577E-17,-1.,3.39243069331623E-14));
#13241=DIRECTION('ref_axis',(-2.08166817117221E-16,-3.39243069331623E-14,
-1.));
#13242=DIRECTION('',(-5.55111512312577E-17,1.,-3.39243069331623E-14));
#13243=DIRECTION('center_axis',(5.55111512312577E-17,-1.,3.39243069331623E-14));
#13244=DIRECTION('ref_axis',(-2.08166817117221E-16,-3.39243069331623E-14,
-1.));
#13245=DIRECTION('center_axis',(-5.55111512330291E-17,1.,-8.54339380874589E-12));
#13246=DIRECTION('ref_axis',(-2.08166817116748E-16,-8.54339380874589E-12,
-1.));
#13247=DIRECTION('center_axis',(-5.55111512312578E-17,1.,-3.44969278837093E-14));
#13248=DIRECTION('ref_axis',(2.08166817117221E-16,3.44969278837093E-14,
1.));
#13249=DIRECTION('center_axis',(5.55111512326456E-17,-1.,6.70116359450593E-12));
#13250=DIRECTION('ref_axis',(2.08166817116851E-16,6.70116359450593E-12,
1.));
#13251=DIRECTION('center_axis',(5.55111512312578E-17,-1.,3.43614026121486E-14));
#13252=DIRECTION('ref_axis',(1.,5.55111512312506E-17,-2.08166817117223E-16));
#13253=DIRECTION('center_axis',(5.55111512312578E-17,-1.,3.43614026121486E-14));
#13254=DIRECTION('ref_axis',(1.,5.55111512312506E-17,-2.08166817117223E-16));
#13255=DIRECTION('center_axis',(5.55111512312578E-17,-1.,3.43614026121486E-14));
#13256=DIRECTION('ref_axis',(1.,5.55111512312506E-17,-2.08166817117223E-16));
#13257=DIRECTION('center_axis',(5.55111512312578E-17,-1.,3.43614026121486E-14));
#13258=DIRECTION('ref_axis',(1.,5.55111512312506E-17,-2.08166817117223E-16));
#13259=DIRECTION('',(-5.55111512312578E-17,1.,-3.43614026121486E-14));
#13260=DIRECTION('center_axis',(5.55111512312578E-17,-1.,3.43614026121486E-14));
#13261=DIRECTION('ref_axis',(1.,5.55111512312506E-17,-2.08166817117223E-16));
#13262=DIRECTION('center_axis',(1.,0.,6.56279692788602E-15));
#13263=DIRECTION('ref_axis',(6.56279692788602E-15,-3.50015836153921E-14,
-1.));
#13264=DIRECTION('center_axis',(5.55111512312578E-17,-1.,3.43614026121486E-14));
#13265=DIRECTION('ref_axis',(1.,5.55111512312506E-17,-2.08166817117223E-16));
#13266=DIRECTION('center_axis',(5.55111512312578E-17,-1.,3.44969278837093E-14));
#13267=DIRECTION('ref_axis',(-2.08166817117221E-16,-3.44969278837093E-14,
-1.));
#13268=DIRECTION('',(-9.98528738451518E-17,0.707106781186525,-0.70710678118657));
#13269=DIRECTION('center_axis',(-5.55111512331082E-17,1.,-8.92338581669359E-12));
#13270=DIRECTION('ref_axis',(2.08166817116727E-16,8.92338581669359E-12,
1.));
#13271=DIRECTION('center_axis',(-5.55111512312578E-17,1.,-3.44969278837093E-14));
#13272=DIRECTION('ref_axis',(-2.08166817117221E-16,-3.44969278837093E-14,
-1.));
#13273=DIRECTION('center_axis',(-5.55111512312578E-17,1.,-3.43614026121486E-14));
#13274=DIRECTION('ref_axis',(-2.08166817117221E-16,-3.43614026121486E-14,
-1.));
#13275=DIRECTION('center_axis',(5.55111512312578E-17,-1.,3.43614026121486E-14));
#13276=DIRECTION('ref_axis',(1.,5.55111512312506E-17,-2.08166817117223E-16));
#13277=DIRECTION('center_axis',(5.55111512312578E-17,-1.,3.43614026121486E-14));
#13278=DIRECTION('ref_axis',(1.,5.55111512312506E-17,-2.08166817117223E-16));
#13279=DIRECTION('center_axis',(5.55111512312578E-17,-1.,3.43614026121486E-14));
#13280=DIRECTION('ref_axis',(1.,5.55111512312506E-17,-2.08166817117223E-16));
#13281=DIRECTION('center_axis',(5.55111512312578E-17,-1.,3.43614026121486E-14));
#13282=DIRECTION('ref_axis',(1.,5.55111512312506E-17,-2.08166817117223E-16));
#13283=DIRECTION('center_axis',(5.55111512312578E-17,-1.,3.43614026121486E-14));
#13284=DIRECTION('ref_axis',(1.,5.55111512312506E-17,-2.08166817117223E-16));
#13285=DIRECTION('center_axis',(5.55111512312578E-17,-1.,3.43614026121486E-14));
#13286=DIRECTION('ref_axis',(1.,5.55111512312506E-17,-2.08166817117223E-16));
#13287=DIRECTION('center_axis',(5.55111512312578E-17,-1.,3.43614026121486E-14));
#13288=DIRECTION('ref_axis',(1.,5.55111512312506E-17,-2.08166817117223E-16));
#13289=DIRECTION('center_axis',(5.55111512312578E-17,-1.,3.43614026121486E-14));
#13290=DIRECTION('ref_axis',(1.,5.55111512312506E-17,-2.08166817117223E-16));
#13291=DIRECTION('center_axis',(5.55111512312578E-17,-1.,3.43614026121486E-14));
#13292=DIRECTION('ref_axis',(-1.,-5.55111512312617E-17,-1.13457712818104E-16));
#13293=DIRECTION('center_axis',(5.55111512312578E-17,-1.,3.43614026121486E-14));
#13294=DIRECTION('ref_axis',(1.,5.55111512312506E-17,-2.08166817117223E-16));
#13295=DIRECTION('center_axis',(5.55111512312578E-17,-1.,3.43614026121486E-14));
#13296=DIRECTION('ref_axis',(1.,5.55111512312506E-17,-2.08166817117223E-16));
#13297=DIRECTION('center_axis',(5.55111512312578E-17,-1.,3.43614026121486E-14));
#13298=DIRECTION('ref_axis',(1.,5.55111512312506E-17,-2.08166817117223E-16));
#13299=DIRECTION('',(0.866025403784438,1.71326272389147E-14,0.500000000000001));
#13300=DIRECTION('',(2.08166817117221E-16,3.43614026121486E-14,1.));
#13301=DIRECTION('',(-0.866025403784438,1.72287753732339E-14,0.500000000000001));
#13302=DIRECTION('',(-0.866025403784438,-1.71326272389147E-14,-0.500000000000001));
#13303=DIRECTION('',(9.97962250772482E-15,-3.43614026121486E-14,-1.));
#13304=DIRECTION('',(0.866025403784438,-1.72287753732339E-14,-0.500000000000001));
#13305=DIRECTION('center_axis',(1.,-5.5511151231265E-17,-2.08166817117219E-16));
#13306=DIRECTION('ref_axis',(2.08166817117221E-16,3.43614026121486E-14,
1.));
#13307=DIRECTION('',(5.55111512312578E-17,-1.,3.43614026121486E-14));
#13308=DIRECTION('',(5.55111512312578E-17,-1.,3.43614026121486E-14));
#13309=DIRECTION('center_axis',(0.5,2.97300919961701E-14,0.866025403784439));
#13310=DIRECTION('ref_axis',(-2.77555756156401E-17,1.,-3.43133285449891E-14));
#13311=DIRECTION('',(5.55111512312578E-17,-1.,3.43614026121486E-14));
#13312=DIRECTION('center_axis',(-0.5,2.97856031474013E-14,0.866025403784439));
#13313=DIRECTION('ref_axis',(2.77555756156334E-17,-1.,3.44094766793082E-14));
#13314=DIRECTION('',(5.55111512312578E-17,-1.,3.43614026121486E-14));
#13315=DIRECTION('center_axis',(-1.,5.55111512312585E-17,2.0377492275074E-17));
#13316=DIRECTION('ref_axis',(2.03774922750759E-17,3.43614026121486E-14,
1.));
#13317=DIRECTION('',(5.55111512312578E-17,-1.,3.43614026121486E-14));
#13318=DIRECTION('center_axis',(-0.5,-2.97300919961701E-14,-0.866025403784439));
#13319=DIRECTION('ref_axis',(-0.866025403784439,1.72287753732339E-14,0.5));
#13320=DIRECTION('',(5.55111512312578E-17,-1.,3.43614026121486E-14));
#13321=DIRECTION('center_axis',(0.5,-2.97856031474012E-14,-0.866025403784438));
#13322=DIRECTION('ref_axis',(-2.77555756156474E-17,1.,-3.44094766793081E-14));
#13323=DIRECTION('axis',(0.,0.,1.));
#13324=DIRECTION('refdir',(1.,0.,0.));
#13325=DIRECTION('center_axis',(0.984807753012209,-0.173648177666927,-6.9026791896102E-15));
#13326=DIRECTION('ref_axis',(6.74488507274914E-15,-1.49880108324396E-15,
1.));
#13327=DIRECTION('center_axis',(0.984807753012209,-0.173648177666927,-6.9026791896102E-15));
#13328=DIRECTION('ref_axis',(-0.173648177666927,-0.984807753012209,-1.41609297436625E-15));
#13329=DIRECTION('center_axis',(-6.74488507274914E-15,1.49880108324396E-15,
-1.));
#13330=DIRECTION('ref_axis',(-0.173648177666927,-0.984807753012209,-3.04793925546002E-16));
#13331=DIRECTION('center_axis',(1.31243041282465E-11,-2.31385942497016E-12,
-1.));
#13332=DIRECTION('ref_axis',(-0.173648177666927,-0.984807753012209,-3.04793925546223E-16));
#13333=DIRECTION('',(6.74488507274914E-15,-1.49880108324396E-15,1.));
#13334=DIRECTION('center_axis',(1.31243041282465E-11,-2.31385942497016E-12,
-1.));
#13335=DIRECTION('ref_axis',(-0.173648177666927,-0.984807753012209,-3.04793925546223E-16));
#13336=DIRECTION('center_axis',(1.31243041282465E-11,-2.31385942497016E-12,
-1.));
#13337=DIRECTION('ref_axis',(-0.173648177666927,-0.984807753012209,-3.04793925546223E-16));
#13338=DIRECTION('center_axis',(0.173648177666927,0.984807753012209,1.41609297436625E-15));
#13339=DIRECTION('ref_axis',(-6.47630097698008E-15,1.85037170770859E-15,
-1.));
#13340=DIRECTION('center_axis',(-0.173648177666927,-0.984807753012209,-1.41609297436625E-15));
#13341=DIRECTION('ref_axis',(-6.31282311555423E-15,2.55105953078819E-15,
-1.));
#13342=DIRECTION('center_axis',(0.984807753012209,-0.173648177666927,-6.9026791896102E-15));
#13343=DIRECTION('ref_axis',(-0.173648177666927,-0.984807753012209,-1.41609297436625E-15));
#13344=DIRECTION('center_axis',(0.984807753012209,-0.173648177666927,-6.9026791896102E-15));
#13345=DIRECTION('ref_axis',(-0.173648177666927,-0.984807753012209,-1.41609297436625E-15));
#13346=DIRECTION('center_axis',(0.984807753012209,-0.173648177666927,-6.9026791896102E-15));
#13347=DIRECTION('ref_axis',(-0.173648177666927,-0.984807753012209,-1.41609297436625E-15));
#13348=DIRECTION('',(-0.984807753012209,0.173648177666927,6.9026791896102E-15));
#13349=DIRECTION('center_axis',(-6.46591174117934E-15,1.44961055799008E-15,
-1.));
#13350=DIRECTION('ref_axis',(-0.173648177666927,-0.984807753012209,-3.04793925546006E-16));
#13351=DIRECTION('axis',(0.,0.,1.));
#13352=DIRECTION('refdir',(1.,0.,0.));
#13353=DIRECTION('center_axis',(2.42833204006769E-16,2.41473507855972E-15,
-1.));
#13354=DIRECTION('ref_axis',(0.422618261740706,0.906307787036647,2.29111895189949E-15));
#13355=DIRECTION('center_axis',(3.62526098085663E-11,-1.69023416117786E-11,
-1.));
#13356=DIRECTION('ref_axis',(0.422618261740706,0.906307787036647,2.29111895186089E-15));
#13357=DIRECTION('',(-2.42833204006769E-16,-2.41473507855972E-15,1.));
#13358=DIRECTION('center_axis',(3.62526098085663E-11,-1.69023416117786E-11,
-1.));
#13359=DIRECTION('ref_axis',(0.422618261740706,0.906307787036647,2.29111895186089E-15));
#13360=DIRECTION('center_axis',(3.62526098085663E-11,-1.69023416117786E-11,
-1.));
#13361=DIRECTION('ref_axis',(0.422618261740706,0.906307787036647,2.29111895186089E-15));
#13362=DIRECTION('center_axis',(0.422618261740706,0.906307787036647,1.97116866169388E-15));
#13363=DIRECTION('ref_axis',(1.33440267382831E-16,2.1350442781253E-15,-1.));
#13364=DIRECTION('center_axis',(-0.422618261740706,-0.906307787036647,-1.97116866169388E-15));
#13365=DIRECTION('ref_axis',(3.8032634610719E-16,1.99759488807599E-15,-1.));
#13366=DIRECTION('center_axis',(0.906307787036647,-0.422618261740706,-8.00429517722823E-16));
#13367=DIRECTION('ref_axis',(0.422618261740706,0.906307787036647,1.97116866169388E-15));
#13368=DIRECTION('center_axis',(0.906307787036647,-0.422618261740706,-8.00429517722823E-16));
#13369=DIRECTION('ref_axis',(0.422618261740706,0.906307787036647,1.97116866169388E-15));
#13370=DIRECTION('center_axis',(0.906307787036647,-0.422618261740706,-8.00429517722823E-16));
#13371=DIRECTION('ref_axis',(0.422618261740706,0.906307787036647,1.97116866169388E-15));
#13372=DIRECTION('',(-0.906307787036647,0.422618261740706,8.00429517722823E-16));
#13373=DIRECTION('center_axis',(0.906307787036647,-0.422618261740706,-8.00429517722823E-16));
#13374=DIRECTION('ref_axis',(0.422618261740706,0.906307787036647,1.97116866169388E-15));
#13375=DIRECTION('center_axis',(2.98328550528607E-16,2.38885717348462E-15,
-1.));
#13376=DIRECTION('ref_axis',(0.906307787036647,-0.422618261740706,-7.39197177765454E-16));
#13377=DIRECTION('center_axis',(0.906307787036647,-0.422618261740706,-8.00429517722823E-16));
#13378=DIRECTION('ref_axis',(2.42833204006769E-16,2.41473507855972E-15,
-1.));
#13379=DIRECTION('axis',(0.,0.,1.));
#13380=DIRECTION('refdir',(1.,0.,0.));
#13381=DIRECTION('center_axis',(0.,1.,1.09634523681734E-15));
#13382=DIRECTION('ref_axis',(1.,0.,0.));
#13383=DIRECTION('',(0.,-1.,-1.09634523681734E-15));
#13384=DIRECTION('center_axis',(0.,1.,1.09634523681734E-15));
#13385=DIRECTION('ref_axis',(1.,0.,0.));
#13386=DIRECTION('center_axis',(0.,1.,1.09634523681734E-15));
#13387=DIRECTION('ref_axis',(0.0907903645015774,-1.09181736006036E-15,0.995870026516347));
#13388=DIRECTION('',(0.,-1.,-1.09634523681734E-15));
#13389=DIRECTION('center_axis',(0.,-1.,-1.09634523681734E-15));
#13390=DIRECTION('ref_axis',(1.,2.83177819361768E-27,-2.58292561368557E-12));
#13391=DIRECTION('center_axis',(0.,1.,1.09634523681734E-15));
#13392=DIRECTION('ref_axis',(0.0907903645015774,-1.09181736006036E-15,0.995870026516347));
#13393=DIRECTION('center_axis',(0.,1.,1.09634523681734E-15));
#13394=DIRECTION('ref_axis',(1.,2.83177819361768E-27,-2.58292561368557E-12));
#13395=DIRECTION('center_axis',(0.,1.,1.09634523681734E-15));
#13396=DIRECTION('ref_axis',(1.,0.,0.));
#13397=DIRECTION('center_axis',(0.,1.,1.09634523681734E-15));
#13398=DIRECTION('ref_axis',(1.,0.,0.));
#13399=DIRECTION('center_axis',(0.,-1.,-1.09634523681734E-15));
#13400=DIRECTION('ref_axis',(1.,0.,0.));
#13401=DIRECTION('center_axis',(0.,1.,1.09634523681734E-15));
#13402=DIRECTION('ref_axis',(1.,0.,0.));
#13403=DIRECTION('',(-0.707106781186547,-0.707106781186548,-8.61828757098662E-16));
#13404=DIRECTION('center_axis',(0.,-1.,-1.09634523681734E-15));
#13405=DIRECTION('ref_axis',(1.,0.,0.));
#13406=DIRECTION('center_axis',(0.,1.,1.09634523681734E-15));
#13407=DIRECTION('ref_axis',(1.,0.,0.));
#13408=DIRECTION('',(0.,1.,1.09634523681734E-15));
#13409=DIRECTION('center_axis',(0.,-1.,-1.09634523681734E-15));
#13410=DIRECTION('ref_axis',(1.,0.,0.));
#13411=DIRECTION('center_axis',(0.,1.,1.09634523681734E-15));
#13412=DIRECTION('ref_axis',(1.,0.,0.));
#13413=DIRECTION('center_axis',(0.,1.,1.09634523681734E-15));
#13414=DIRECTION('ref_axis',(1.,0.,0.));
#13415=DIRECTION('',(-0.707106781186547,0.707106781186548,8.61828757098662E-16));
#13416=DIRECTION('center_axis',(0.,1.,1.09634523681734E-15));
#13417=DIRECTION('ref_axis',(1.,0.,0.));
#13418=DIRECTION('center_axis',(0.,1.,1.09634523681734E-15));
#13419=DIRECTION('ref_axis',(1.,0.,0.));
#13420=DIRECTION('center_axis',(0.,-1.,-1.09634523681734E-15));
#13421=DIRECTION('ref_axis',(1.,0.,0.));
#13422=DIRECTION('center_axis',(0.,1.,1.09634523681734E-15));
#13423=DIRECTION('ref_axis',(1.,0.,0.));
#13424=DIRECTION('center_axis',(0.,1.,1.09634523681734E-15));
#13425=DIRECTION('ref_axis',(1.,0.,0.));
#13426=DIRECTION('center_axis',(0.,1.,1.09634523681734E-15));
#13427=DIRECTION('ref_axis',(1.,0.,0.));
#13428=DIRECTION('center_axis',(0.,-1.,-1.09634523681734E-15));
#13429=DIRECTION('ref_axis',(1.,0.,0.));
#13430=DIRECTION('',(0.707106781186547,0.707106781186548,8.61828757098662E-16));
#13431=DIRECTION('',(6.08761714816612E-5,-0.999999998147046,-1.55027293578175E-16));
#13432=DIRECTION('',(0.999999998147046,6.08761714816612E-5,4.44089209027163E-16));
#13433=DIRECTION('',(6.08761714816612E-5,-0.999999998147046,-1.55027293578175E-16));
#13434=DIRECTION('',(0.999999998147046,6.08761714816612E-5,4.44089209027163E-16));
#13435=DIRECTION('',(6.08761714816612E-5,-0.999999998147046,-1.55027293578175E-16));
#13436=DIRECTION('',(0.999999998147046,6.08761714816612E-5,4.44089209027163E-16));
#13437=DIRECTION('',(6.08761714816612E-5,-0.999999998147046,-1.55027293578175E-16));
#13438=DIRECTION('',(0.999999998147046,6.08761714816612E-5,4.44089209027163E-16));
#13439=DIRECTION('',(6.08761714816612E-5,-0.999999998147046,-1.55027293578175E-16));
#13440=DIRECTION('',(0.999999998147046,6.08761714816612E-5,4.44089209027163E-16));
#13441=DIRECTION('',(6.08761714816612E-5,-0.999999998147046,-1.55027293578175E-16));
#13442=DIRECTION('',(0.999999998147046,6.08761714816612E-5,4.44089209027163E-16));
#13443=DIRECTION('',(6.08761714816612E-5,-0.999999998147046,-1.55027293578175E-16));
#13444=DIRECTION('',(0.999999998147046,6.08761714816612E-5,4.44089209027163E-16));
#13445=DIRECTION('',(6.08761714816612E-5,-0.999999998147046,-1.55027293578175E-16));
#13446=DIRECTION('',(0.999999998147046,6.08761714816612E-5,4.44089209027163E-16));
#13447=DIRECTION('',(6.08761714816612E-5,-0.999999998147046,-1.55027293578175E-16));
#13448=DIRECTION('',(0.999999998147046,6.08761714816612E-5,4.44089209027163E-16));
#13449=DIRECTION('',(6.08761714816612E-5,-0.999999998147046,-1.55027293578175E-16));
#13450=DIRECTION('',(0.999999998147046,6.08761714816612E-5,4.44089209027163E-16));
#13451=DIRECTION('',(6.08761714816612E-5,-0.999999998147046,-1.55027293578175E-16));
#13452=DIRECTION('',(0.999999998147046,6.08761714816612E-5,4.44089209027163E-16));
#13453=DIRECTION('',(6.08761714816612E-5,-0.999999998147046,-1.55027293578175E-16));
#13454=DIRECTION('',(0.999999998147046,6.08761714816612E-5,4.44089209027163E-16));
#13455=DIRECTION('',(6.08761714816612E-5,-0.999999998147046,-1.55027293578175E-16));
#13456=DIRECTION('',(0.999999998147046,6.08761714816612E-5,4.44089209027163E-16));
#13457=DIRECTION('',(6.08761714816612E-5,-0.999999998147046,-1.55027293578175E-16));
#13458=DIRECTION('',(0.999999998147046,6.08761714816612E-5,4.44089209027163E-16));
#13459=DIRECTION('',(6.08761714816612E-5,-0.999999998147046,-1.55027293578175E-16));
#13460=DIRECTION('',(0.999999998147046,6.08761714816612E-5,4.44089209027163E-16));
#13461=DIRECTION('',(6.08761714816612E-5,-0.999999998147046,-1.55027293578175E-16));
#13462=DIRECTION('',(0.999999998147046,6.08761714816612E-5,4.44089209027163E-16));
#13463=DIRECTION('',(6.08761714816612E-5,-0.999999998147046,-1.55027293578175E-16));
#13464=DIRECTION('',(0.999999998147046,6.08761714816612E-5,4.44089209027163E-16));
#13465=DIRECTION('',(6.08761714816612E-5,-0.999999998147046,-1.55027293578175E-16));
#13466=DIRECTION('',(0.999999998147046,6.08761714816612E-5,4.44089209027163E-16));
#13467=DIRECTION('',(6.08761714816612E-5,-0.999999998147046,-1.55027293578175E-16));
#13468=DIRECTION('',(0.999999998147046,6.08761714816612E-5,4.44089209027163E-16));
#13469=DIRECTION('',(6.08761714816612E-5,-0.999999998147046,-1.55027293578175E-16));
#13470=DIRECTION('',(0.999999998147046,6.08761714816612E-5,4.44089209027163E-16));
#13471=CARTESIAN_POINT('',(0.,0.,0.));
#13472=CARTESIAN_POINT('',(0.,0.,0.));
#13473=CARTESIAN_POINT('Origin',(0.006,-0.0355287743898724,-0.0045758532865581));
#13474=CARTESIAN_POINT('',(0.00652827282717588,-0.0343958896560766,-0.0043758532865481));
#13475=CARTESIAN_POINT('Origin',(0.006,-0.0355287743898724,-0.0043758532865481));
#13476=CARTESIAN_POINT('',(0.00652827282717588,-0.0343958896560766,-0.0045758532865481));
#13477=CARTESIAN_POINT('',(0.00652827282717588,-0.0343958896560766,-0.0045758532865581));
#13478=CARTESIAN_POINT('Origin',(0.006,-0.0355287743898724,-0.0045758532865481));
#13479=CARTESIAN_POINT('Origin',(0.006,-0.0355287743898724,-0.0043758532865581));
#13480=CARTESIAN_POINT('Origin',(0.006,-0.0355287743898724,-0.0045758532865581));
#13481=CARTESIAN_POINT('',(0.,0.,0.));
#13482=CARTESIAN_POINT('Origin',(-0.00508700257531012,-0.0309105091425022,
0.0016241467134419));
#13483=CARTESIAN_POINT('',(-0.0052454844234719,-0.0312503745626367,0.0016241467134419));
#13484=CARTESIAN_POINT('Origin',(-0.00508700257532341,-0.0309105091425071,
0.0016241467134519));
#13485=CARTESIAN_POINT('Origin',(0.00578869086912964,-0.0359819282833906,
-0.0013758532865581));
#13486=CARTESIAN_POINT('',(0.00563020902097688,-0.0363217937035293,-0.0043758532865581));
#13487=CARTESIAN_POINT('Origin',(0.00578869086912542,-0.0359819282833998,
-0.0043758532865481));
#13488=CARTESIAN_POINT('',(0.00563020902097688,-0.0363217937035293,-0.0013758532865381));
#13489=CARTESIAN_POINT('',(0.00563020902097688,-0.0363217937035293,-0.0013758532865581));
#13490=CARTESIAN_POINT('',(0.00544882544898185,-0.0358234464352337,-0.0013758532865581));
#13491=CARTESIAN_POINT('Origin',(0.00578869086912542,-0.0359819282833998,
-0.0013758532865481));
#13492=CARTESIAN_POINT('Origin',(0.00578869086912542,-0.0359819282833998,
-0.0013758532865481));
#13493=CARTESIAN_POINT('Origin',(0.0030697675080197,-0.0347140734981686,
-0.0013758532865581));
#13494=CARTESIAN_POINT('',(0.00306976750801062,-0.0347140734981644,0.0012491467134419));
#13495=CARTESIAN_POINT('Origin',(0.0030697675080197,-0.0347140734981686,
-0.0013758532865581));
#13496=CARTESIAN_POINT('',(0.00291128565985791,-0.035053938918303,0.0016241467134419));
#13497=CARTESIAN_POINT('Origin',(0.00306976750800641,-0.0347140734981734,
0.0016241467134519));
#13498=CARTESIAN_POINT('Origin',(0.00306976750800641,-0.0347140734981734,
0.0016241467134519));
#13499=CARTESIAN_POINT('Origin',(-0.01052484929753,-0.0283747995720579,
0.00162414671344191));
#13500=CARTESIAN_POINT('',(-0.0106833311456828,-0.0287146649921966,0.00162414671344191));
#13501=CARTESIAN_POINT('Origin',(0.00578869086912964,-0.0359819282833906,
-0.0043758532865581));
#13502=CARTESIAN_POINT('',(0.,0.,0.));
#13503=CARTESIAN_POINT('Origin',(-0.00466438431356942,-0.0300042013554656,
0.00162414671344191));
#13504=CARTESIAN_POINT('',(-0.00482286616173126,-0.0303440667756001,0.0016241467134419));
#13505=CARTESIAN_POINT('Origin',(-0.00466438431357425,-0.0300042013554523,
0.00162414671345191));
#13506=CARTESIAN_POINT('Origin',(0.00621130913087035,-0.035075620496354,
-0.0013758532865581));
#13507=CARTESIAN_POINT('',(0.00605282728271759,-0.0354154859164927,-0.0043758532865581));
#13508=CARTESIAN_POINT('Origin',(0.00621130913087458,-0.035075620496345,
-0.0043758532865481));
#13509=CARTESIAN_POINT('',(0.00605282728271759,-0.0354154859164927,-0.0013758532865381));
#13510=CARTESIAN_POINT('',(0.00605282728271759,-0.0354154859164927,-0.0013758532865581));
#13511=CARTESIAN_POINT('',(0.00587144371072257,-0.034917138648197,-0.0013758532865581));
#13512=CARTESIAN_POINT('Origin',(0.00621130913087458,-0.035075620496345,
-0.0013758532865481));
#13513=CARTESIAN_POINT('Origin',(0.00621130913087458,-0.035075620496345,
-0.0013758532865481));
#13514=CARTESIAN_POINT('Origin',(0.00349238576976041,-0.0338077657111319,
-0.0013758532865581));
#13515=CARTESIAN_POINT('',(0.00349238576975134,-0.0338077657111277,0.0012491467134419));
#13516=CARTESIAN_POINT('Origin',(0.00349238576976041,-0.0338077657111319,
-0.0013758532865581));
#13517=CARTESIAN_POINT('',(0.00333390392159855,-0.0341476311312665,0.0016241467134419));
#13518=CARTESIAN_POINT('Origin',(0.00349238576975557,-0.0338077657111186,
0.0016241467134519));
#13519=CARTESIAN_POINT('Origin',(0.00349238576975557,-0.0338077657111186,
0.0016241467134519));
#13520=CARTESIAN_POINT('Origin',(-0.0101022310357893,-0.0274684917850214,
0.00162414671344191));
#13521=CARTESIAN_POINT('',(-0.0102607128839421,-0.0278083572051601,0.00162414671344191));
#13522=CARTESIAN_POINT('Origin',(0.00621130913087035,-0.035075620496354,
-0.0043758532865581));
#13523=CARTESIAN_POINT('',(0.,0.,0.));
#13524=CARTESIAN_POINT('Origin',(0.,0.0159712256101277,-0.012175853286558));
#13525=CARTESIAN_POINT('',(0.0028500000000131,0.0163712256101177,-0.012175853286558));
#13526=CARTESIAN_POINT('Origin',(0.,0.0163712256101177,-0.012175853286558));
#13527=CARTESIAN_POINT('',(0.00245000000001309,0.0159712256101177,-0.012175853286558));
#13528=CARTESIAN_POINT('Origin',(0.00285,0.0159712256101277,-0.012175853286558));
#13529=CARTESIAN_POINT('Origin',(0.,0.0159712256101177,-0.012175853286558));
#13530=CARTESIAN_POINT('Origin',(0.,0.0163712256101277,-0.012175853286558));
#13531=CARTESIAN_POINT('',(-0.00345,0.0163712256101177,-0.012175853286558));
#13532=CARTESIAN_POINT('Origin',(0.,0.0163712256101177,-0.012175853286558));
#13533=CARTESIAN_POINT('Origin',(0.,0.0163712256101277,-0.012175853286558));
#13534=CARTESIAN_POINT('',(0.00213600093632938,0.0129712256101277,-0.013375853286558));
#13535=CARTESIAN_POINT('',(0.00245,0.0129712256101177,-0.012175853286558));
#13536=CARTESIAN_POINT('Origin',(0.,0.0129712256101177,-0.012175853286558));
#13537=CARTESIAN_POINT('',(0.00213600093632938,0.0153712256101277,-0.013375853286558));
#13538=CARTESIAN_POINT('',(0.00213600093633938,0.0163712256101177,-0.013375853286568));
#13539=CARTESIAN_POINT('',(0.00095,0.0153712256101277,-0.0144341712446852));
#13540=CARTESIAN_POINT('Origin',(0.,0.0153712256101177,-0.012175853286558));
#13541=CARTESIAN_POINT('',(0.00095,0.0129712256101277,-0.0144341712446852));
#13542=CARTESIAN_POINT('',(0.00095000000001,0.0163712256101177,-0.0144341712446952));
#13543=CARTESIAN_POINT('',(-0.00095,0.0129712256101277,-0.0144341712446852));
#13544=CARTESIAN_POINT('Origin',(0.,0.0129712256101177,-0.012175853286558));
#13545=CARTESIAN_POINT('',(-0.00095,0.0153712256101277,-0.0144341712446852));
#13546=CARTESIAN_POINT('',(-0.00095000000001,0.0163712256101177,-0.0144341712446952));
#13547=CARTESIAN_POINT('',(-0.00213600093632938,0.0153712256101277,-0.013375853286558));
#13548=CARTESIAN_POINT('Origin',(0.,0.0153712256101177,-0.012175853286558));
#13549=CARTESIAN_POINT('',(-0.00213600093632938,0.0129712256101277,-0.013375853286558));
#13550=CARTESIAN_POINT('',(-0.00213600093633938,0.0163712256101177,-0.013375853286568));
#13551=CARTESIAN_POINT('',(-0.00213600093632938,0.0129712256101277,-0.010975853286558));
#13552=CARTESIAN_POINT('Origin',(0.,0.0129712256101177,-0.012175853286558));
#13553=CARTESIAN_POINT('',(-0.00213600093632938,0.0153712256101277,-0.010975853286558));
#13554=CARTESIAN_POINT('',(-0.00213600093633938,0.0163712256101177,-0.010975853286548));
#13555=CARTESIAN_POINT('',(-0.00095,0.0153712256101277,-0.00991753532843076));
#13556=CARTESIAN_POINT('Origin',(0.,0.0153712256101177,-0.012175853286558));
#13557=CARTESIAN_POINT('',(-0.00095,0.0129712256101277,-0.00991753532843077));
#13558=CARTESIAN_POINT('',(-0.00095000000001,0.0163712256101177,-0.00991753532842076));
#13559=CARTESIAN_POINT('',(0.00095,0.0129712256101277,-0.00991753532843077));
#13560=CARTESIAN_POINT('Origin',(0.,0.0129712256101177,-0.012175853286558));
#13561=CARTESIAN_POINT('',(0.00095,0.0153712256101277,-0.00991753532843076));
#13562=CARTESIAN_POINT('',(0.00095000000001,0.0163712256101177,-0.00991753532842076));
#13563=CARTESIAN_POINT('',(0.00213600093632938,0.0153712256101277,-0.010975853286558));
#13564=CARTESIAN_POINT('Origin',(0.,0.0153712256101177,-0.012175853286558));
#13565=CARTESIAN_POINT('',(0.00213600093632938,0.0129712256101277,-0.010975853286558));
#13566=CARTESIAN_POINT('',(0.00213600093633938,0.0163712256101177,-0.010975853286548));
#13567=CARTESIAN_POINT('Origin',(0.,0.0129712256101177,-0.012175853286558));
#13568=CARTESIAN_POINT('',(0.00245,0.0163712256101277,-0.012175853286558));
#13569=CARTESIAN_POINT('Origin',(0.,0.0171212256101277,-0.012175853286558));
#13570=CARTESIAN_POINT('',(0.00200000000001,0.0171212256101177,-0.012175853286558));
#13571=CARTESIAN_POINT('Origin',(0.,0.0171212256101177,-0.012175853286558));
#13572=CARTESIAN_POINT('',(0.00240000000001,0.0175212256101277,-0.012175853286558));
#13573=CARTESIAN_POINT('Origin',(0.0024,0.0171212256101277,-0.012175853286558));
#13574=CARTESIAN_POINT('Origin',(0.,0.0175212256101277,-0.012175853286558));
#13575=CARTESIAN_POINT('Origin',(0.,0.0129712256101277,-0.012175853286558));
#13576=CARTESIAN_POINT('',(0.002,0.0109712256101177,-0.012175853286558));
#13577=CARTESIAN_POINT('',(0.002,0.0129712256101277,-0.012175853286558));
#13578=CARTESIAN_POINT('',(0.0016,0.0109712256101277,-0.010975853286558));
#13579=CARTESIAN_POINT('Origin',(0.,0.0109712256101177,-0.012175853286558));
#13580=CARTESIAN_POINT('',(0.00151986841535707,0.0121712256101277,-0.010875853286558));
#13581=CARTESIAN_POINT('Origin',(0.,-0.0034287743898823,-0.012175853286558));
#13582=CARTESIAN_POINT('',(0.00151986841535707,0.0124712256101277,-0.010875853286558));
#13583=CARTESIAN_POINT('',(0.00151986841536707,0.0129712256101177,-0.010875853286548));
#13584=CARTESIAN_POINT('',(0.0016,0.0129712256101277,-0.010975853286558));
#13585=CARTESIAN_POINT('Origin',(0.,0.0189712256101377,-0.012175853286558));
#13586=CARTESIAN_POINT('',(0.0016,0.0153712256101277,-0.010975853286558));
#13587=CARTESIAN_POINT('',(0.00160000000001,0.0163712256101177,-0.010975853286548));
#13588=CARTESIAN_POINT('',(0.00095,0.0153712256101277,-0.0104158816958782));
#13589=CARTESIAN_POINT('Origin',(0.,0.0153712256101177,-0.012175853286558));
#13590=CARTESIAN_POINT('',(0.00095,0.0129712256101277,-0.0104158816958782));
#13591=CARTESIAN_POINT('',(0.00095000000001,0.0163712256101177,-0.0104158816958682));
#13592=CARTESIAN_POINT('',(0.00105,0.0124712256101277,-0.0104736488335031));
#13593=CARTESIAN_POINT('Origin',(0.,0.0177212256101377,-0.012175853286558));
#13594=CARTESIAN_POINT('',(0.00105,0.0121712256101277,-0.0104736488335031));
#13595=CARTESIAN_POINT('',(0.00105000000001,0.0129712256101177,-0.0104736488334931));
#13596=CARTESIAN_POINT('',(0.00095,0.0109712256101277,-0.0104158816958782));
#13597=CARTESIAN_POINT('Origin',(0.,-0.0004287743898823,-0.012175853286558));
#13598=CARTESIAN_POINT('',(-0.00095,0.0109712256101277,-0.0104158816958782));
#13599=CARTESIAN_POINT('Origin',(0.,0.0109712256101177,-0.012175853286558));
#13600=CARTESIAN_POINT('',(-0.00105,0.0121712256101277,-0.0104736488335031));
#13601=CARTESIAN_POINT('Origin',(0.,-0.0004287743898823,-0.012175853286558));
#13602=CARTESIAN_POINT('',(-0.00105,0.0124712256101277,-0.0104736488335031));
#13603=CARTESIAN_POINT('',(-0.00105000000001,0.0129712256101177,-0.0104736488334931));
#13604=CARTESIAN_POINT('',(-0.00095,0.0129712256101277,-0.0104158816958782));
#13605=CARTESIAN_POINT('Origin',(0.,0.0177212256101377,-0.012175853286558));
#13606=CARTESIAN_POINT('',(-0.00095,0.0153712256101277,-0.0104158816958782));
#13607=CARTESIAN_POINT('',(-0.00095000000001,0.0163712256101177,-0.0104158816958682));
#13608=CARTESIAN_POINT('',(-0.0016,0.0153712256101277,-0.010975853286558));
#13609=CARTESIAN_POINT('Origin',(0.,0.0153712256101177,-0.012175853286558));
#13610=CARTESIAN_POINT('',(-0.0016,0.0129712256101277,-0.010975853286558));
#13611=CARTESIAN_POINT('',(-0.00160000000001,0.0163712256101177,-0.010975853286548));
#13612=CARTESIAN_POINT('',(-0.00151986841535707,0.0124712256101277,-0.010875853286558));
#13613=CARTESIAN_POINT('Origin',(0.,0.0189712256101377,-0.012175853286558));
#13614=CARTESIAN_POINT('',(-0.00151986841535707,0.0121712256101277,-0.010875853286558));
#13615=CARTESIAN_POINT('',(-0.00151986841536707,0.0129712256101177,-0.010875853286548));
#13616=CARTESIAN_POINT('',(-0.0016,0.0109712256101277,-0.010975853286558));
#13617=CARTESIAN_POINT('Origin',(0.,-0.0034287743898823,-0.012175853286558));
#13618=CARTESIAN_POINT('',(-0.0016,0.0109712256101277,-0.013375853286558));
#13619=CARTESIAN_POINT('Origin',(0.,0.0109712256101177,-0.012175853286558));
#13620=CARTESIAN_POINT('',(-0.00151986841535707,0.0121712256101277,-0.013475853286558));
#13621=CARTESIAN_POINT('Origin',(0.,-0.0034287743898823,-0.012175853286558));
#13622=CARTESIAN_POINT('',(-0.00151986841535707,0.0124712256101277,-0.013475853286558));
#13623=CARTESIAN_POINT('',(-0.00151986841536707,0.0129712256101177,-0.013475853286568));
#13624=CARTESIAN_POINT('',(-0.0016,0.0129712256101277,-0.013375853286558));
#13625=CARTESIAN_POINT('Origin',(0.,0.0189712256101377,-0.012175853286558));
#13626=CARTESIAN_POINT('',(-0.0016,0.0153712256101277,-0.013375853286558));
#13627=CARTESIAN_POINT('',(-0.00160000000001,0.0163712256101177,-0.013375853286568));
#13628=CARTESIAN_POINT('',(-0.00095,0.0153712256101277,-0.0139358248772378));
#13629=CARTESIAN_POINT('Origin',(0.,0.0153712256101177,-0.012175853286558));
#13630=CARTESIAN_POINT('',(-0.00095,0.0129712256101277,-0.0139358248772378));
#13631=CARTESIAN_POINT('',(-0.00095000000001,0.0163712256101177,-0.0139358248772478));
#13632=CARTESIAN_POINT('',(-0.00105,0.0124712256101277,-0.0138780577396129));
#13633=CARTESIAN_POINT('Origin',(0.,0.0177212256101377,-0.012175853286558));
#13634=CARTESIAN_POINT('',(-0.00105,0.0121712256101277,-0.0138780577396129));
#13635=CARTESIAN_POINT('',(-0.00105000000001,0.0129712256101177,-0.0138780577396229));
#13636=CARTESIAN_POINT('',(-0.00095,0.0109712256101277,-0.0139358248772378));
#13637=CARTESIAN_POINT('Origin',(0.,-0.0004287743898823,-0.012175853286558));
#13638=CARTESIAN_POINT('',(0.00095,0.0109712256101277,-0.0139358248772378));
#13639=CARTESIAN_POINT('Origin',(0.,0.0109712256101177,-0.012175853286558));
#13640=CARTESIAN_POINT('',(0.00105,0.0121712256101277,-0.0138780577396129));
#13641=CARTESIAN_POINT('Origin',(0.,-0.0004287743898823,-0.012175853286558));
#13642=CARTESIAN_POINT('',(0.00105,0.0124712256101277,-0.0138780577396129));
#13643=CARTESIAN_POINT('',(0.00105000000001,0.0129712256101177,-0.0138780577396229));
#13644=CARTESIAN_POINT('',(0.00095,0.0129712256101277,-0.0139358248772378));
#13645=CARTESIAN_POINT('Origin',(0.,0.0177212256101377,-0.012175853286558));
#13646=CARTESIAN_POINT('',(0.00095,0.0153712256101277,-0.0139358248772378));
#13647=CARTESIAN_POINT('',(0.00095000000001,0.0163712256101177,-0.0139358248772478));
#13648=CARTESIAN_POINT('',(0.0016,0.0153712256101277,-0.013375853286558));
#13649=CARTESIAN_POINT('Origin',(0.,0.0153712256101177,-0.012175853286558));
#13650=CARTESIAN_POINT('',(0.0016,0.0129712256101277,-0.013375853286558));
#13651=CARTESIAN_POINT('',(0.00160000000001,0.0163712256101177,-0.013375853286568));
#13652=CARTESIAN_POINT('',(0.00151986841535707,0.0124712256101277,-0.013475853286558));
#13653=CARTESIAN_POINT('Origin',(0.,0.0189712256101377,-0.012175853286558));
#13654=CARTESIAN_POINT('',(0.00151986841535707,0.0121712256101277,-0.013475853286558));
#13655=CARTESIAN_POINT('',(0.00151986841536707,0.0129712256101177,-0.013475853286568));
#13656=CARTESIAN_POINT('',(0.0016,0.0109712256101277,-0.013375853286558));
#13657=CARTESIAN_POINT('Origin',(0.,-0.0034287743898823,-0.012175853286558));
#13658=CARTESIAN_POINT('Origin',(0.,0.0109712256101177,-0.012175853286558));
#13659=CARTESIAN_POINT('Origin',(0.,0.0175212256101277,-0.012175853286558));
#13660=CARTESIAN_POINT('',(-0.00345,0.0175212256101277,-0.012175853286558));
#13661=CARTESIAN_POINT('Origin',(0.,0.0175212256101277,-0.012175853286558));
#13662=CARTESIAN_POINT('Origin',(0.001,0.0115712256101277,-0.0143575051632916));
#13663=CARTESIAN_POINT('',(0.00095,0.0109712256101277,-0.0143252718125785));
#13664=CARTESIAN_POINT('',(0.00095000000001,0.0109712256101177,-0.0143575051633016));
#13665=CARTESIAN_POINT('',(0.00105,0.0121712256101277,-0.0148253815464564));
#13666=CARTESIAN_POINT('Ctrl Pts',(0.00095000000001,0.0109712256101177,
-0.0143252718125885));
#13667=CARTESIAN_POINT('Ctrl Pts',(0.000994789380303646,0.0115086981736415,
-0.014550321192835));
#13668=CARTESIAN_POINT('Ctrl Pts',(0.00105000000001,0.0121712256101177,
-0.0148253815464664));
#13669=CARTESIAN_POINT('',(0.00105000000001,0.0121712256101177,-0.0143575051633016));
#13670=CARTESIAN_POINT('Origin',(0.,0.0115712256101277,-0.012175853286558));
#13671=CARTESIAN_POINT('',(-0.00095,0.0109712256101277,-0.0143252718125785));
#13672=CARTESIAN_POINT('Origin',(0.,0.0109712256101177,-0.012175853286558));
#13673=CARTESIAN_POINT('',(-0.00105,0.0121712256101277,-0.0148253815464564));
#13674=CARTESIAN_POINT('Ctrl Pts',(-0.00105000000001,0.0121712256101177,
-0.0148253815464664));
#13675=CARTESIAN_POINT('Ctrl Pts',(-0.000994789380303646,0.0115086981736415,
-0.014550321192835));
#13676=CARTESIAN_POINT('Ctrl Pts',(-0.00095000000001,0.0109712256101177,
-0.0143252718125885));
#13677=CARTESIAN_POINT('Origin',(0.,0.0121712256101177,-0.012175853286558));
#13678=CARTESIAN_POINT('Origin',(1.38777878078145E-19,0.0109712256101277,
-0.0142808390818979));
#13679=CARTESIAN_POINT('',(-0.00095000000001,0.0109712256101177,-0.0141083319795779));
#13680=CARTESIAN_POINT('Origin',(-0.001,0.0115712256101277,-0.0141083319795679));
#13681=CARTESIAN_POINT('',(-0.00105000000001,0.0121712256101177,-0.0141083319795779));
#13682=CARTESIAN_POINT('Origin',(-0.00208050046816469,0.0115712256101277,
-0.013425853286558));
#13683=CARTESIAN_POINT('',(-0.00202051973511768,0.0109712256101277,-0.013375853286558));
#13684=CARTESIAN_POINT('',(-0.00208050046817469,0.0109712256101177,-0.013375853286568));
#13685=CARTESIAN_POINT('',(-0.00253623737059448,0.0121712256101277,-0.013475853286558));
#13686=CARTESIAN_POINT('Ctrl Pts',(-0.00202051973512767,0.0109712256101177,
-0.013375853286568));
#13687=CARTESIAN_POINT('Ctrl Pts',(-0.00225204403530932,0.0115033197344889,
-0.0134201944635989));
#13688=CARTESIAN_POINT('Ctrl Pts',(-0.00253623737060448,0.0121712256101177,
-0.013475853286568));
#13689=CARTESIAN_POINT('',(-0.00208050046817469,0.0121712256101177,-0.013475853286568));
#13690=CARTESIAN_POINT('Origin',(-0.002025,0.0109712256101277,-0.012175853286558));
#13691=CARTESIAN_POINT('',(-0.00202051973511768,0.0109712256101277,-0.010975853286558));
#13692=CARTESIAN_POINT('',(-0.00181250000001,0.0109712256101177,-0.010975853286548));
#13693=CARTESIAN_POINT('Origin',(0.,0.0109712256101177,-0.012175853286558));
#13694=CARTESIAN_POINT('Origin',(0.0018125,0.0115712256101277,-0.013425853286558));
#13695=CARTESIAN_POINT('',(0.00253623737059448,0.0121712256101277,-0.013475853286558));
#13696=CARTESIAN_POINT('',(0.00202051973511768,0.0109712256101277,-0.013375853286558));
#13697=CARTESIAN_POINT('Ctrl Pts',(0.00253623737060448,0.0121712256101177,
-0.013475853286568));
#13698=CARTESIAN_POINT('Ctrl Pts',(0.00225204403530932,0.0115033197344889,
-0.0134201944635989));
#13699=CARTESIAN_POINT('Ctrl Pts',(0.00202051973512767,0.0109712256101177,
-0.013375853286568));
#13700=CARTESIAN_POINT('',(0.00181250000001,0.0109712256101177,-0.013375853286568));
#13701=CARTESIAN_POINT('',(0.00181250000001,0.0121712256101177,-0.013475853286568));
#13702=CARTESIAN_POINT('Origin',(0.002025,0.0109712256101277,-0.012175853286558));
#13703=CARTESIAN_POINT('',(0.00202051973511768,0.0109712256101277,-0.010975853286558));
#13704=CARTESIAN_POINT('Origin',(0.,0.0109712256101177,-0.012175853286558));
#13705=CARTESIAN_POINT('',(0.00208050046817469,0.0109712256101177,-0.010975853286548));
#13706=CARTESIAN_POINT('Origin',(0.00208050046816469,0.0115712256101277,
-0.010925853286558));
#13707=CARTESIAN_POINT('',(0.00253623737059448,0.0121712256101277,-0.010875853286558));
#13708=CARTESIAN_POINT('Ctrl Pts',(0.00202051973512767,0.0109712256101177,
-0.010975853286548));
#13709=CARTESIAN_POINT('Ctrl Pts',(0.00225204403530932,0.0115033197344889,
-0.0109315121095171));
#13710=CARTESIAN_POINT('Ctrl Pts',(0.00253623737060448,0.0121712256101177,
-0.010875853286548));
#13711=CARTESIAN_POINT('',(0.00208050046817469,0.0121712256101177,-0.010875853286548));
#13712=CARTESIAN_POINT('Origin',(0.001,0.0115712256101277,-0.0102433745935482));
#13713=CARTESIAN_POINT('',(0.00105,0.0121712256101277,-0.00952632502665966));
#13714=CARTESIAN_POINT('',(0.00095,0.0109712256101277,-0.0100264347605375));
#13715=CARTESIAN_POINT('Ctrl Pts',(0.00105000000001,0.0121712256101177,
-0.00952632502664966));
#13716=CARTESIAN_POINT('Ctrl Pts',(0.000994789380303646,0.0115086981736415,
-0.00980138538028098));
#13717=CARTESIAN_POINT('Ctrl Pts',(0.00095000000001,0.0109712256101177,
-0.0100264347605275));
#13718=CARTESIAN_POINT('',(0.00095000000001,0.0109712256101177,-0.0102433745935382));
#13719=CARTESIAN_POINT('',(0.00105000000001,0.0121712256101177,-0.0102433745935382));
#13720=CARTESIAN_POINT('Origin',(1.38777878078145E-19,0.0109712256101277,
-0.0100708674912181));
#13721=CARTESIAN_POINT('',(-0.00095,0.0109712256101277,-0.0100264347605375));
#13722=CARTESIAN_POINT('Origin',(0.,0.0109712256101177,-0.012175853286558));
#13723=CARTESIAN_POINT('',(-0.00095000000001,0.0109712256101177,-0.00999420140981444));
#13724=CARTESIAN_POINT('Origin',(0.,0.0115712256101277,-0.012175853286558));
#13725=CARTESIAN_POINT('',(-0.00105,0.0121712256101277,-0.00952632502665966));
#13726=CARTESIAN_POINT('Origin',(0.,0.0121712256101177,-0.012175853286558));
#13727=CARTESIAN_POINT('Ctrl Pts',(-0.00095000000001,0.0109712256101177,
-0.0100264347605275));
#13728=CARTESIAN_POINT('Ctrl Pts',(-0.000994789380303646,0.0115086981736415,
-0.00980138538028098));
#13729=CARTESIAN_POINT('Ctrl Pts',(-0.00105000000001,0.0121712256101177,
-0.00952632502664966));
#13730=CARTESIAN_POINT('Origin',(-0.0018125,0.0115712256101277,-0.010925853286558));
#13731=CARTESIAN_POINT('',(-0.00253623737059448,0.0121712256101277,-0.010875853286558));
#13732=CARTESIAN_POINT('Ctrl Pts',(-0.00253623737060448,0.0121712256101177,
-0.010875853286548));
#13733=CARTESIAN_POINT('Ctrl Pts',(-0.00225204403530932,0.0115033197344889,
-0.0109315121095171));
#13734=CARTESIAN_POINT('Ctrl Pts',(-0.00202051973512767,0.0109712256101177,
-0.010975853286548));
#13735=CARTESIAN_POINT('',(-0.00181250000001,0.0121712256101177,-0.010875853286548));
#13736=CARTESIAN_POINT('Origin',(0.,0.0115712256101277,-0.012175853286558));
#13737=CARTESIAN_POINT('Origin',(0.,0.0121712256101177,-0.012175853286558));
#13738=CARTESIAN_POINT('Origin',(-0.001,0.0115712256101277,-0.00999420140982444));
#13739=CARTESIAN_POINT('',(-0.00105000000001,0.0121712256101177,-0.00999420140981444));
#13740=CARTESIAN_POINT('Origin',(-0.00105,0.0129712256101277,-0.00991753532843077));
#13741=CARTESIAN_POINT('',(-0.00105,0.0124712256101277,-0.00952632502665966));
#13742=CARTESIAN_POINT('',(-0.00105000000001,0.0129712256101177,-0.00952632502664966));
#13743=CARTESIAN_POINT('',(-0.00105000000001,0.0124712256101177,-0.00999420140981444));
#13744=CARTESIAN_POINT('Origin',(-0.00208050046816469,0.0127212256101277,
-0.013425853286558));
#13745=CARTESIAN_POINT('',(-0.00253623737059448,0.0124712256101277,-0.013475853286558));
#13746=CARTESIAN_POINT('',(-0.00208050046817469,0.0124712256101177,-0.013475853286568));
#13747=CARTESIAN_POINT('',(-0.00225,0.0129712256101277,-0.013375853286558));
#13748=CARTESIAN_POINT('Origin',(0.417653699675352,-0.218496268260033,-0.0596693520771347));
#13749=CARTESIAN_POINT('',(-0.00208050046817469,0.0129712256101177,-0.013375853286568));
#13750=CARTESIAN_POINT('',(-0.00208050046817469,0.0129712256101177,-0.013375853286568));
#13751=CARTESIAN_POINT('Origin',(-0.002025,0.0129712256101277,-0.012175853286558));
#13752=CARTESIAN_POINT('',(-0.00225,0.0129712256101277,-0.010975853286558));
#13753=CARTESIAN_POINT('Origin',(0.,0.0129712256101177,-0.012175853286558));
#13754=CARTESIAN_POINT('',(-0.00181250000001,0.0129712256101177,-0.010975853286548));
#13755=CARTESIAN_POINT('Origin',(0.,0.0127212256101277,-0.012175853286558));
#13756=CARTESIAN_POINT('',(-0.00253623737059448,0.0124712256101277,-0.010875853286558));
#13757=CARTESIAN_POINT('Origin',(0.,0.0124712256101177,-0.012175853286558));
#13758=CARTESIAN_POINT('Origin',(0.417653699675352,-0.218496268260033,0.0353176455040183));
#13759=CARTESIAN_POINT('Origin',(-0.001,0.0127212256101277,-0.0141083319795679));
#13760=CARTESIAN_POINT('',(-0.00095,0.0129712256101277,-0.0145422851997979));
#13761=CARTESIAN_POINT('',(-0.00105,0.0124712256101277,-0.0148253815464564));
#13762=CARTESIAN_POINT('Ctrl Pts',(-0.000950000000000006,0.0129712256101277,
-0.0145422851997978));
#13763=CARTESIAN_POINT('Ctrl Pts',(-0.000997178044325374,0.0127353353885008,
-0.0146758588281839));
#13764=CARTESIAN_POINT('Ctrl Pts',(-0.00105,0.0124712256101277,-0.0148253815464564));
#13765=CARTESIAN_POINT('',(-0.00105000000001,0.0124712256101177,-0.0141083319795779));
#13766=CARTESIAN_POINT('',(-0.00095000000001,0.0129712256101177,-0.0141083319795779));
#13767=CARTESIAN_POINT('',(-0.00095000000001,0.0129712256101177,-0.0141083319795779));
#13768=CARTESIAN_POINT('Origin',(0.,0.0127212256101277,-0.012175853286558));
#13769=CARTESIAN_POINT('',(0.00095,0.0129712256101277,-0.0145422851997979));
#13770=CARTESIAN_POINT('Origin',(0.,0.0129712256101177,-0.012175853286558));
#13771=CARTESIAN_POINT('',(0.00105,0.0124712256101277,-0.0148253815464564));
#13772=CARTESIAN_POINT('Ctrl Pts',(0.00105,0.0124712256101277,-0.0148253815464564));
#13773=CARTESIAN_POINT('Ctrl Pts',(0.000997178044325414,0.0127353353885006,
-0.0146758588281841));
#13774=CARTESIAN_POINT('Ctrl Pts',(0.000950000000000005,0.0129712256101277,
-0.0145422851997979));
#13775=CARTESIAN_POINT('Origin',(0.,0.0124712256101177,-0.012175853286558));
#13776=CARTESIAN_POINT('Origin',(1.38777878078145E-19,0.0129712256101277,
-0.0142808390818979));
#13777=CARTESIAN_POINT('',(0.00095000000001,0.0129712256101177,-0.0143575051633016));
#13778=CARTESIAN_POINT('Origin',(0.001,0.0127212256101277,-0.0143575051632916));
#13779=CARTESIAN_POINT('',(0.00105000000001,0.0124712256101177,-0.0143575051633016));
#13780=CARTESIAN_POINT('',(0.00095000000001,0.0129712256101177,-0.0143575051633016));
#13781=CARTESIAN_POINT('Origin',(0.00105,0.0129712256101277,-0.0144341712446852));
#13782=CARTESIAN_POINT('',(0.00105000000001,0.0129712256101177,-0.0148253815464664));
#13783=CARTESIAN_POINT('Origin',(0.0018125,0.0127212256101277,-0.013425853286558));
#13784=CARTESIAN_POINT('',(0.00225,0.0129712256101277,-0.013375853286558));
#13785=CARTESIAN_POINT('',(0.00253623737059448,0.0124712256101277,-0.013475853286558));
#13786=CARTESIAN_POINT('Origin',(-0.417653699675352,-0.218496268260033,
-0.0596693520771347));
#13787=CARTESIAN_POINT('',(0.00181250000001,0.0124712256101177,-0.013475853286568));
#13788=CARTESIAN_POINT('',(0.00181250000001,0.0129712256101177,-0.013375853286568));
#13789=CARTESIAN_POINT('',(0.00181250000001,0.0129712256101177,-0.013375853286568));
#13790=CARTESIAN_POINT('Origin',(0.,0.0127212256101277,-0.012175853286558));
#13791=CARTESIAN_POINT('',(0.00225,0.0129712256101277,-0.010975853286558));
#13792=CARTESIAN_POINT('Origin',(0.,0.0129712256101177,-0.012175853286558));
#13793=CARTESIAN_POINT('',(0.00253623737059448,0.0124712256101277,-0.010875853286558));
#13794=CARTESIAN_POINT('Origin',(-0.417653699675352,-0.218496268260033,
0.0353176455040183));
#13795=CARTESIAN_POINT('Origin',(0.,0.0124712256101177,-0.012175853286558));
#13796=CARTESIAN_POINT('Origin',(0.002025,0.0129712256101277,-0.012175853286558));
#13797=CARTESIAN_POINT('',(0.00208050046817469,0.0129712256101177,-0.010975853286548));
#13798=CARTESIAN_POINT('Origin',(0.00208050046816469,0.0127212256101277,
-0.010925853286558));
#13799=CARTESIAN_POINT('',(0.00208050046817469,0.0124712256101177,-0.010875853286548));
#13800=CARTESIAN_POINT('',(0.00208050046817469,0.0129712256101177,-0.010975853286548));
#13801=CARTESIAN_POINT('Origin',(0.00213600093632938,0.0129712256101277,
-0.010875853286558));
#13802=CARTESIAN_POINT('',(0.00253623737060448,0.0129712256101177,-0.010875853286548));
#13803=CARTESIAN_POINT('Origin',(0.001,0.0127212256101277,-0.0102433745935482));
#13804=CARTESIAN_POINT('',(0.00095,0.0129712256101277,-0.00980942137331815));
#13805=CARTESIAN_POINT('',(0.00105,0.0124712256101277,-0.00952632502665966));
#13806=CARTESIAN_POINT('Ctrl Pts',(0.00095,0.0129712256101277,-0.00980942137331815));
#13807=CARTESIAN_POINT('Ctrl Pts',(0.000997178044311125,0.0127353353885721,
-0.00967584774497245));
#13808=CARTESIAN_POINT('Ctrl Pts',(0.00105,0.0124712256101277,-0.00952632502665967));
#13809=CARTESIAN_POINT('',(0.00105000000001,0.0124712256101177,-0.0102433745935382));
#13810=CARTESIAN_POINT('',(0.00095000000001,0.0129712256101177,-0.0102433745935382));
#13811=CARTESIAN_POINT('',(0.00095000000001,0.0129712256101177,-0.0102433745935382));
#13812=CARTESIAN_POINT('Origin',(0.,0.0127212256101277,-0.012175853286558));
#13813=CARTESIAN_POINT('',(-0.00095,0.0129712256101277,-0.00980942137331815));
#13814=CARTESIAN_POINT('Origin',(0.,0.0129712256101177,-0.012175853286558));
#13815=CARTESIAN_POINT('Ctrl Pts',(-0.00104999999999999,0.0124712256101277,
-0.00952632502665963));
#13816=CARTESIAN_POINT('Ctrl Pts',(-0.000997178044319801,0.0127353353885287,
-0.00967584774494786));
#13817=CARTESIAN_POINT('Ctrl Pts',(-0.00095,0.0129712256101277,-0.00980942137331816));
#13818=CARTESIAN_POINT('Origin',(0.,0.0124712256101177,-0.012175853286558));
#13819=CARTESIAN_POINT('Origin',(1.38777878078145E-19,0.0129712256101277,
-0.0100708674912181));
#13820=CARTESIAN_POINT('',(-0.00095000000001,0.0129712256101177,-0.00999420140981443));
#13821=CARTESIAN_POINT('Origin',(-0.0018125,0.0127212256101277,-0.010925853286558));
#13822=CARTESIAN_POINT('',(-0.00181250000001,0.0124712256101177,-0.010875853286548));
#13823=CARTESIAN_POINT('',(-0.00181250000001,0.0129712256101177,-0.010975853286548));
#13824=CARTESIAN_POINT('Origin',(-0.001,0.0127212256101277,-0.00999420140982444));
#13825=CARTESIAN_POINT('',(-0.00095000000001,0.0129712256101177,-0.00999420140981443));
#13826=CARTESIAN_POINT('Origin',(-0.00095,0.0163712256101277,-0.0139358248772378));
#13827=CARTESIAN_POINT('',(-0.00095000000001,0.0153712256101177,-0.0144341712446952));
#13828=CARTESIAN_POINT('Origin',(0.00095,0.0163712256101277,-0.0144341712446852));
#13829=CARTESIAN_POINT('',(0.00095000000001,0.0153712256101177,-0.0139358248772478));
#13830=CARTESIAN_POINT('Origin',(-0.0016,0.0163712256101277,-0.010975853286558));
#13831=CARTESIAN_POINT('',(-0.00213600093633938,0.0153712256101177,-0.010975853286548));
#13832=CARTESIAN_POINT('Origin',(-0.00213600093632938,0.0163712256101277,
-0.013375853286558));
#13833=CARTESIAN_POINT('',(-0.00160000000001,0.0153712256101177,-0.013375853286568));
#13834=CARTESIAN_POINT('Origin',(0.0016,0.0163712256101277,-0.013375853286558));
#13835=CARTESIAN_POINT('',(0.00213600093633938,0.0153712256101177,-0.013375853286568));
#13836=CARTESIAN_POINT('Origin',(0.00213600093632938,0.0163712256101277,
-0.010975853286558));
#13837=CARTESIAN_POINT('',(0.00160000000001,0.0153712256101177,-0.010975853286548));
#13838=CARTESIAN_POINT('Origin',(0.00095,0.0163712256101277,-0.0104158816958782));
#13839=CARTESIAN_POINT('',(0.00095000000001,0.0153712256101177,-0.00991753532842076));
#13840=CARTESIAN_POINT('Origin',(-0.00095,0.0163712256101277,-0.00991753532843076));
#13841=CARTESIAN_POINT('',(-0.00095000000001,0.0153712256101177,-0.0104158816958682));
#13842=CARTESIAN_POINT('Origin',(-0.00154300046816469,0.0153712256101277,
-0.0139050122656216));
#13843=CARTESIAN_POINT('Origin',(-0.00154300046816469,0.0153712256101277,
-0.0104466943074944));
#13844=CARTESIAN_POINT('Origin',(0.00154300046816469,0.0153712256101277,
-0.0139050122656216));
#13845=CARTESIAN_POINT('Origin',(0.00154300046816469,0.0153712256101277,
-0.0104466943074944));
#13846=CARTESIAN_POINT('Origin',(0.,0.0175212256101277,-0.012175853286558));
#13847=CARTESIAN_POINT('',(-0.00345,0.0175212256101277,-0.012175853286558));
#13848=CARTESIAN_POINT('Origin',(-0.00213600093632938,0.0129712256101277,
-0.013475853286558));
#13849=CARTESIAN_POINT('',(-0.00253623737060448,0.0129712256101177,-0.013475853286568));
#13850=CARTESIAN_POINT('Origin',(0.,0.0129712256101277,-0.012175853286558));
#13851=CARTESIAN_POINT('',(-0.00253623737060448,0.0129712256101177,-0.010875853286548));
#13852=CARTESIAN_POINT('Origin',(-0.0016,0.0129712256101277,-0.010875853286558));
#13853=CARTESIAN_POINT('Origin',(0.,0.0115712256101277,-0.012175853286558));
#13854=CARTESIAN_POINT('Origin',(0.,0.0121712256101177,-0.012175853286558));
#13855=CARTESIAN_POINT('Origin',(0.,0.0129712256101277,-0.012175853286558));
#13856=CARTESIAN_POINT('',(0.00253623737060448,0.0129712256101177,-0.013475853286568));
#13857=CARTESIAN_POINT('Origin',(0.0016,0.0129712256101277,-0.013475853286558));
#13858=CARTESIAN_POINT('Origin',(0.,0.0129712256101277,-0.012175853286558));
#13859=CARTESIAN_POINT('',(0.00105000000001,0.0129712256101177,-0.00952632502664966));
#13860=CARTESIAN_POINT('Origin',(0.00105,0.0129712256101277,-0.0104158816958782));
#13861=CARTESIAN_POINT('Origin',(0.,0.0129712256101277,-0.012175853286558));
#13862=CARTESIAN_POINT('',(-0.00105000000001,0.0129712256101177,-0.0148253815464664));
#13863=CARTESIAN_POINT('Origin',(-0.00105,0.0129712256101277,-0.0139358248772378));
#13864=CARTESIAN_POINT('',(0.,0.,0.));
#13865=CARTESIAN_POINT('Origin',(0.,-0.0291247811395418,-0.0121758532865581));
#13866=CARTESIAN_POINT('',(0.00307327823453674,-0.0236251335354893,-0.0121742489211595));
#13867=CARTESIAN_POINT('',(0.00307327999164594,-0.0226251873529714,-0.0121774473169523));
#13868=CARTESIAN_POINT('Ctrl Pts',(0.00307266966487839,-0.0236261040574453,
-0.0121759154876736));
#13869=CARTESIAN_POINT('Ctrl Pts',(0.00307016915329888,-0.0235977132371358,
-0.0127445659805958));
#13870=CARTESIAN_POINT('Ctrl Pts',(0.00291138345935846,-0.0235660101645814,
-0.0133130648648865));
#13871=CARTESIAN_POINT('Ctrl Pts',(0.00261246228220724,-0.0235347411284561,
-0.0137968579377696));
#13872=CARTESIAN_POINT('Ctrl Pts',(0.00256279224538186,-0.0235295453300498,
-0.0138772470891003));
#13873=CARTESIAN_POINT('Ctrl Pts',(0.00250945992878158,-0.0235245080538991,
-0.0139553652459075));
#13874=CARTESIAN_POINT('Ctrl Pts',(0.00245251305124659,-0.0235196091447056,
-0.0140307197566707));
#13875=CARTESIAN_POINT('Ctrl Pts',(0.00236729119587557,-0.0235122778537054,
-0.0141434889109384));
#13876=CARTESIAN_POINT('Ctrl Pts',(0.00227396676332056,-0.0235052564434052,
-0.0142500644674973));
#13877=CARTESIAN_POINT('Ctrl Pts',(0.00217394442652592,-0.0234984773627037,
-0.0143496603071668));
#13878=CARTESIAN_POINT('Ctrl Pts',(0.00177992504288088,-0.0234717724357315,
-0.0147419995847498));
#13879=CARTESIAN_POINT('Ctrl Pts',(0.00127516616801139,-0.0234445247812332,
-0.0150239885753106));
#13880=CARTESIAN_POINT('Ctrl Pts',(0.00073465934568833,-0.0234142110768737,
-0.0151592520636632));
#13881=CARTESIAN_POINT('Ctrl Pts',(0.000494490103978782,-0.023400741460786,
-0.0152193551522589));
#13882=CARTESIAN_POINT('Ctrl Pts',(0.000247123644285777,-0.023386522593376,
-0.0152501029941088));
#13883=CARTESIAN_POINT('Ctrl Pts',(1.40972321978975E-7,-0.0233730175728703,
-0.0152504987812254));
#13884=CARTESIAN_POINT('Ctrl Pts',(-7.83185877626713E-5,-0.0233687274015826,
-0.0152506245118397));
#13885=CARTESIAN_POINT('Ctrl Pts',(-0.000156800353640954,-0.0233645659408657,
-0.0152477937223375));
#13886=CARTESIAN_POINT('Ctrl Pts',(-0.000235091041689717,-0.0233605024316512,
-0.0152418357342434));
#13887=CARTESIAN_POINT('Ctrl Pts',(-0.000695274669722541,-0.0233366175934987,
-0.0152068153678981));
#13888=CARTESIAN_POINT('Ctrl Pts',(-0.00115014572941729,-0.0233161169334347,
-0.015062471823434));
#13889=CARTESIAN_POINT('Ctrl Pts',(-0.00154928198099346,-0.0232927539572789,
-0.0148289427165404));
#13890=CARTESIAN_POINT('Ctrl Pts',(-0.00177706402867699,-0.0232794210001052,
-0.0146956705871563));
#13891=CARTESIAN_POINT('Ctrl Pts',(-0.00198730690683751,-0.0232652961508513,
-0.0145337037807864));
#13892=CARTESIAN_POINT('Ctrl Pts',(-0.00217300374575874,-0.023250687363939,
-0.014348841907857));
#13893=CARTESIAN_POINT('Ctrl Pts',(-0.00238459919233331,-0.0232340411312481,
-0.014138197877596));
#13894=CARTESIAN_POINT('Ctrl Pts',(-0.00256713902217867,-0.0232182993007945,
-0.0138989931398254));
#13895=CARTESIAN_POINT('Ctrl Pts',(-0.0027091022637822,-0.023202981860163,
-0.0136364623794192));
#13896=CARTESIAN_POINT('Ctrl Pts',(-0.00290226137111884,-0.023182140527395,
-0.0132792557761064));
#13897=CARTESIAN_POINT('Ctrl Pts',(-0.00302027471933705,-0.0231620848706945,
-0.0128785372613051));
#13898=CARTESIAN_POINT('Ctrl Pts',(-0.00305878637852152,-0.0231416057675226,
-0.0124657293521869));
#13899=CARTESIAN_POINT('Ctrl Pts',(-0.00306774188078499,-0.0231368435563198,
-0.012369734989888));
#13900=CARTESIAN_POINT('Ctrl Pts',(-0.00307226364115996,-0.0231319708591869,
-0.0122729662540278));
#13901=CARTESIAN_POINT('Ctrl Pts',(-0.00307223516061164,-0.0231269651224307,
-0.0121757719601571));
#13902=CARTESIAN_POINT('Ctrl Pts',(-0.00307211467525599,-0.0231057886350063,
-0.0117645969739148));
#13903=CARTESIAN_POINT('Ctrl Pts',(-0.00298797170067459,-0.0230814861616835,
-0.011344231287885));
#13904=CARTESIAN_POINT('Ctrl Pts',(-0.00282463481379235,-0.0230585539910371,
-0.0109620988921809));
#13905=CARTESIAN_POINT('Ctrl Pts',(-0.00278445639446726,-0.0230529130217137,
-0.0108681000660409));
#13906=CARTESIAN_POINT('Ctrl Pts',(-0.0027398227705807,-0.0230475030896191,
-0.0107763253627915));
#13907=CARTESIAN_POINT('Ctrl Pts',(-0.00269066644906558,-0.0230422565180116,
-0.0106872915136893));
#13908=CARTESIAN_POINT('Ctrl Pts',(-0.0025399881165119,-0.0230261742596757,
-0.0104143770337189));
#13909=CARTESIAN_POINT('Ctrl Pts',(-0.00234664362815788,-0.0230116269359496,
-0.0101670750656678));
#13910=CARTESIAN_POINT('Ctrl Pts',(-0.00212290995656839,-0.0229966653588366,
-0.00995470874154361));
#13911=CARTESIAN_POINT('Ctrl Pts',(-0.00171792617680668,-0.0229695831766718,
-0.00957030117326437));
#13912=CARTESIAN_POINT('Ctrl Pts',(-0.00120940308263932,-0.0229397098462347,
-0.00929766716641838));
#13913=CARTESIAN_POINT('Ctrl Pts',(-0.000670241834339137,-0.0229087613604071,
-0.00917583945292269));
#13914=CARTESIAN_POINT('Ctrl Pts',(-0.000515800944709547,-0.0228998962728308,
-0.00914094232240165));
#13915=CARTESIAN_POINT('Ctrl Pts',(-0.000358970911346579,-0.0228912777688333,
-0.00911794398325095));
#13916=CARTESIAN_POINT('Ctrl Pts',(-0.000201812288102591,-0.0228830565703485,
-0.00910763794284517));
#13917=CARTESIAN_POINT('Ctrl Pts',(-0.000103652758974647,-0.0228779217011604,
-0.00910120090456802));
#13918=CARTESIAN_POINT('Ctrl Pts',(-5.36347989276417E-6,-0.0228729418253322,
-0.00909970729402443));
#13919=CARTESIAN_POINT('Ctrl Pts',(9.25541750715132E-5,-0.0228681536676443,
-0.00910282920369337));
#13920=CARTESIAN_POINT('Ctrl Pts',(0.000650123353395021,-0.0228408886238822,
-0.00912060618793129));
#13921=CARTESIAN_POINT('Ctrl Pts',(0.00119953279408264,-0.0228146503881801,
-0.00929613564276958));
#13922=CARTESIAN_POINT('Ctrl Pts',(0.00166459553365405,-0.0227849878508226,
-0.00959380052075975));
#13923=CARTESIAN_POINT('Ctrl Pts',(0.0018684611856092,-0.0227719849331462,
-0.00972428537635481));
#13924=CARTESIAN_POINT('Ctrl Pts',(0.00205606806776706,-0.0227582037588869,
-0.00987855234620668));
#13925=CARTESIAN_POINT('Ctrl Pts',(0.00222231380956152,-0.0227448458698992,
-0.0100517128871323));
#13926=CARTESIAN_POINT('Ctrl Pts',(0.0023120057077202,-0.0227376391023406,
-0.0101451354159391));
#13927=CARTESIAN_POINT('Ctrl Pts',(0.00239582829502692,-0.0227307808936713,
-0.0102438423450844));
#13928=CARTESIAN_POINT('Ctrl Pts',(0.00247270790098799,-0.0227241552630883,
-0.0103475351539342));
#13929=CARTESIAN_POINT('Ctrl Pts',(0.00273607139307683,-0.0227014580967096,
-0.0107027515979027));
#13930=CARTESIAN_POINT('Ctrl Pts',(0.00291787292036907,-0.0226814902703287,
-0.0111174335847037));
#13931=CARTESIAN_POINT('Ctrl Pts',(0.00300723758665274,-0.0226595892781931,
-0.0115466031829495));
#13932=CARTESIAN_POINT('Ctrl Pts',(0.00305043961649606,-0.0226490015665708,
-0.011754078895245));
#13933=CARTESIAN_POINT('Ctrl Pts',(0.00307226150597443,-0.022637922840801,
-0.0119653371521074));
#13934=CARTESIAN_POINT('Ctrl Pts',(0.00307261119196602,-0.0226264261836896,
-0.0121759442462848));
#13935=CARTESIAN_POINT('',(0.00307349983335769,-0.0216248189898234,-0.0121765573521433));
#13936=CARTESIAN_POINT('Ctrl Pts',(0.00307349929150754,-0.0226247811395518,
-0.0121779401748277));
#13937=CARTESIAN_POINT('Ctrl Pts',(0.00307311430164888,-0.0225954191960958,
-0.0127449403707989));
#13938=CARTESIAN_POINT('Ctrl Pts',(0.00291152735071005,-0.0225660572526398,
-0.013311969538757));
#13939=CARTESIAN_POINT('Ctrl Pts',(0.00261308932736971,-0.0225366953091838,
-0.013793928197428));
#13940=CARTESIAN_POINT('Ctrl Pts',(0.0024880548265633,-0.0225243937401624,
-0.0139958510610824));
#13941=CARTESIAN_POINT('Ctrl Pts',(0.00233962293493056,-0.0225120921711411,
-0.0141830137117398));
#13942=CARTESIAN_POINT('Ctrl Pts',(0.00217200314735264,-0.0224997906021197,
-0.0143504347584488));
#13943=CARTESIAN_POINT('Ctrl Pts',(0.00177929151526496,-0.0224709696059985,
-0.0147426807662081));
#13944=CARTESIAN_POINT('Ctrl Pts',(0.0012756988519483,-0.0224421486098772,
-0.0150270336580492));
#13945=CARTESIAN_POINT('Ctrl Pts',(0.000734866705221547,-0.022413327613756,
-0.0151602080200904));
#13946=CARTESIAN_POINT('Ctrl Pts',(0.000493874143373817,-0.0224004850973999,
-0.0152195499635659));
#13947=CARTESIAN_POINT('Ctrl Pts',(0.000245874960503312,-0.0223876425810437,
-0.0152494784326798));
#13948=CARTESIAN_POINT('Ctrl Pts',(-1.5594132469024E-6,-0.0223748000646876,
-0.0152493528909554));
#13949=CARTESIAN_POINT('Ctrl Pts',(-0.000558901941837568,-0.0223458724729755,
-0.0152490701099455));
#13950=CARTESIAN_POINT('Ctrl Pts',(-0.0011180148393364,-0.0223169448812633,
-0.0150928521766949));
#13951=CARTESIAN_POINT('Ctrl Pts',(-0.00159573531068977,-0.0222880172895512,
-0.0148026443075984));
#13952=CARTESIAN_POINT('Ctrl Pts',(-0.00180606080655659,-0.022275281368786,
-0.0146748747904176));
#13953=CARTESIAN_POINT('Ctrl Pts',(-0.00200076576455277,-0.0222625454480207,
-0.0145218188158553));
#13954=CARTESIAN_POINT('Ctrl Pts',(-0.0021742086799485,-0.0222498095272555,
-0.0143482296043347));
#13955=CARTESIAN_POINT('Ctrl Pts',(-0.00256808227296006,-0.0222208873723167,
-0.0139540237857016));
#13956=CARTESIAN_POINT('Ctrl Pts',(-0.0028529831357351,-0.0221919652173779,
-0.0134483316010587));
#13957=CARTESIAN_POINT('Ctrl Pts',(-0.00298564563878129,-0.0221630430624391,
-0.0129054575420462));
#13958=CARTESIAN_POINT('Ctrl Pts',(-0.00304408873843441,-0.0221503017049005,
-0.0126662999654782));
#13959=CARTESIAN_POINT('Ctrl Pts',(-0.00307358224738798,-0.022137560347362,
-0.0124203009577403));
#13960=CARTESIAN_POINT('Ctrl Pts',(-0.0030734998267616,-0.0221248189898234,
-0.0121748213483798));
#13961=CARTESIAN_POINT('Ctrl Pts',(-0.0030733127366404,-0.0220958968348846,
-0.0116175966354908));
#13962=CARTESIAN_POINT('Ctrl Pts',(-0.00291725456535694,-0.0220669746799457,
-0.0110585559437886));
#13963=CARTESIAN_POINT('Ctrl Pts',(-0.00262723032005655,-0.0220380525250069,
-0.0105808413444788));
#13964=CARTESIAN_POINT('Ctrl Pts',(-0.00249946312525238,-0.0220253111674683,
-0.0103703890969173));
#13965=CARTESIAN_POINT('Ctrl Pts',(-0.00234638295676836,-0.0220125698099298,
-0.0101755642197633));
#13966=CARTESIAN_POINT('Ctrl Pts',(-0.00217274942421638,-0.0219998284523912,
-0.0100020174625899));
#13967=CARTESIAN_POINT('Ctrl Pts',(-0.00177853711818865,-0.0219709008606791,
-0.00960800216874991));
#13968=CARTESIAN_POINT('Ctrl Pts',(-0.00127278554717199,-0.0219419732689669,
-0.00932298654933162));
#13969=CARTESIAN_POINT('Ctrl Pts',(-0.000729818611945095,-0.0219130456772548,
-0.00919026003836461));
#13970=CARTESIAN_POINT('Ctrl Pts',(-0.000490767123179356,-0.0219003097564896,
-0.00913182467520187));
#13971=CARTESIAN_POINT('Ctrl Pts',(-0.000244876181528169,-0.0218875738357243,
-0.00910231305287151));
#13972=CARTESIAN_POINT('Ctrl Pts',(5.04463079185754E-7,-0.0218748379149591,
-0.00910235332795764));
#13973=CARTESIAN_POINT('Ctrl Pts',(0.000555793298242175,-0.0218460169188379,
-0.00910244446923611));
#13974=CARTESIAN_POINT('Ctrl Pts',(0.00111307090434215,-0.0218171959227166,
-0.00925735919509966));
#13975=CARTESIAN_POINT('Ctrl Pts',(0.00158968958608715,-0.0217883749265954,
-0.0095453990919586));
#13976=CARTESIAN_POINT('Ctrl Pts',(0.00180206889422062,-0.0217755324102393,
-0.00967374847554921));
#13977=CARTESIAN_POINT('Ctrl Pts',(0.00199858963676925,-0.0217626898938831,
-0.00982783015738682));
#13978=CARTESIAN_POINT('Ctrl Pts',(0.00217346290396063,-0.021749847377527,
-0.010002730819897));
#13979=CARTESIAN_POINT('Ctrl Pts',(0.00257327699341549,-0.021720485434071,
-0.0104026075434791));
#13980=CARTESIAN_POINT('Ctrl Pts',(0.00286066137097504,-0.0216911234906151,
-0.0109168534823359));
#13981=CARTESIAN_POINT('Ctrl Pts',(0.00299114972208898,-0.0216617615471591,
-0.0114691527912653));
#13982=CARTESIAN_POINT('Ctrl Pts',(0.0030458195180486,-0.0216494599781377,
-0.0117005457874222));
#13983=CARTESIAN_POINT('Ctrl Pts',(0.00307349822130347,-0.0216371584091163,
-0.0119382780953225));
#13984=CARTESIAN_POINT('Ctrl Pts',(0.00307349999991385,-0.0216248568400949,
-0.0121758302745233));
#13985=CARTESIAN_POINT('',(0.0030734993528554,-0.0206247116996209,-0.0121744194201276));
#13986=CARTESIAN_POINT('Ctrl Pts',(0.00307349966680153,-0.0216247811395518,
-0.0121772844297633));
#13987=CARTESIAN_POINT('Ctrl Pts',(0.0030732356479493,-0.0215954136692731,
-0.0127442869850705));
#13988=CARTESIAN_POINT('Ctrl Pts',(0.00291176844050567,-0.0215660461989944,
-0.0133113525384645));
#13989=CARTESIAN_POINT('Ctrl Pts',(0.00261343117209257,-0.0215366787287157,
-0.0137933760093459));
#13990=CARTESIAN_POINT('Ctrl Pts',(0.00248848650987813,-0.0215243795323277,
-0.0139952490775987));
#13991=CARTESIAN_POINT('Ctrl Pts',(0.00234015906022308,-0.0215120803359398,
-0.014182378104514));
#13992=CARTESIAN_POINT('Ctrl Pts',(0.002172652235586,-0.0214997811395518,
-0.0143497862462427));
#13993=CARTESIAN_POINT('Ctrl Pts',(0.00178005414938768,-0.021470954606817,
-0.0147421530420382));
#13994=CARTESIAN_POINT('Ctrl Pts',(0.00127654165317278,-0.0214421280740823,
-0.0150266571933579));
#13995=CARTESIAN_POINT('Ctrl Pts',(0.000735744851787406,-0.0214133015413475,
-0.0151599916484757));
#13996=CARTESIAN_POINT('Ctrl Pts',(0.000494859018460462,-0.0214004614074156,
-0.0152193824977743));
#13997=CARTESIAN_POINT('Ctrl Pts',(0.000246963129670334,-0.0213876212734837,
-0.0152493838499329));
#13998=CARTESIAN_POINT('Ctrl Pts',(-3.80074158312444E-7,-0.0213747811395518,
-0.0152493532630578));
#13999=CARTESIAN_POINT('Ctrl Pts',(-0.000557727405901423,-0.0213458480042346,
-0.0152492843405526));
#14000=CARTESIAN_POINT('Ctrl Pts',(-0.00111690398182406,-0.0213169148689173,
-0.0150932784200768));
#14001=CARTESIAN_POINT('Ctrl Pts',(-0.00159473782610428,-0.0212879817336001,
-0.0148032500049834));
#14002=CARTESIAN_POINT('Ctrl Pts',(-0.00180503346704472,-0.0212752482022506,
-0.0146756079131285));
#14003=CARTESIAN_POINT('Ctrl Pts',(-0.00199972987390663,-0.0212625146709012,
-0.0145226923737388));
#14004=CARTESIAN_POINT('Ctrl Pts',(-0.00217318983351514,-0.0212497811395518,
-0.0143492488321288));
#14005=CARTESIAN_POINT('Ctrl Pts',(-0.00256725147934152,-0.0212208534473509,
-0.0139552244842675));
#14006=CARTESIAN_POINT('Ctrl Pts',(-0.00285239027995229,-0.02119192575515,
-0.013449661601223));
#14007=CARTESIAN_POINT('Ctrl Pts',(-0.00298530606556781,-0.0211629980629491,
-0.0129068457248801));
#14008=CARTESIAN_POINT('Ctrl Pts',(-0.00304383858822103,-0.0211502590884833,
-0.0126678042714409));
#14009=CARTESIAN_POINT('Ctrl Pts',(-0.00307344635440524,-0.0211375201140176,
-0.0124219130413494));
#14010=CARTESIAN_POINT('Ctrl Pts',(-0.00307349992675546,-0.0211247811395518,
-0.012176524281491));
#14011=CARTESIAN_POINT('Ctrl Pts',(-0.00307362157897022,-0.0210958534473509,
-0.0116192949272901));
#14012=CARTESIAN_POINT('Ctrl Pts',(-0.00291787070471117,-0.02106692575515,
-0.0110601641731118));
#14013=CARTESIAN_POINT('Ctrl Pts',(-0.00262810741779381,-0.0210379980629491,
-0.0105822869557965));
#14014=CARTESIAN_POINT('Ctrl Pts',(-0.00250050349116459,-0.0210252590884833,
-0.0103718427341533));
#14015=CARTESIAN_POINT('Ctrl Pts',(-0.00234759692874837,-0.0210125201140176,
-0.0101770002697919));
#14016=CARTESIAN_POINT('Ctrl Pts',(-0.00217413860137922,-0.0209997811395518,
-0.0100034068333646));
#14017=CARTESIAN_POINT('Ctrl Pts',(-0.00178017492155852,-0.0209708480042346,
-0.00960913628985804));
#14018=CARTESIAN_POINT('Ctrl Pts',(-0.00127460120093978,-0.0209419148689173,
-0.00932379654364457));
#14019=CARTESIAN_POINT('Ctrl Pts',(-0.0007317150245235,-0.0209129817336001,
-0.00919072424866265));
#14020=CARTESIAN_POINT('Ctrl Pts',(-0.000492789720688787,-0.0209002482022506,
-0.00913215886259882));
#14021=CARTESIAN_POINT('Ctrl Pts',(-0.000247011714850828,-0.0208875146709012,
-0.0091024912033574));
#14022=CARTESIAN_POINT('Ctrl Pts',(-1.72206394589758E-6,-0.0208747811395518,
-0.00910235376898928));
#14023=CARTESIAN_POINT('Ctrl Pts',(0.000553571668584063,-0.020845954606817,
-0.009102042641133));
#14024=CARTESIAN_POINT('Ctrl Pts',(0.00111096533262494,-0.0208171280740823,
-0.0092565562732921));
#14025=CARTESIAN_POINT('Ctrl Pts',(0.00158779473491439,-0.0207883015413475,
-0.00954425488828792));
#14026=CARTESIAN_POINT('Ctrl Pts',(0.00180018772176464,-0.0207754614074156,
-0.00967240379827177));
#14027=CARTESIAN_POINT('Ctrl Pts',(0.00199675249277233,-0.0207626212734837,
-0.00982627724709428));
#14028=CARTESIAN_POINT('Ctrl Pts',(0.00217170281880654,-0.0207497811395518,
-0.0100009718836334));
#14029=CARTESIAN_POINT('Ctrl Pts',(0.00257184260919384,-0.0207204136692731,
-0.0104005268706466));
#14030=CARTESIAN_POINT('Ctrl Pts',(0.00285964364699999,-0.0206910461989944,
-0.0109145426511768));
#14031=CARTESIAN_POINT('Ctrl Pts',(0.00299057826765684,-0.0206616787287157,
-0.0114667384333653));
#14032=CARTESIAN_POINT('Ctrl Pts',(0.00304541413190247,-0.0206493795323277,
-0.0116979999041451));
#14033=CARTESIAN_POINT('Ctrl Pts',(0.00307328449308178,-0.0206370803359398,
-0.0119356176270179));
#14034=CARTESIAN_POINT('Ctrl Pts',(0.00307349874893983,-0.0206247811395518,
-0.0121730801538007));
#14035=CARTESIAN_POINT('',(0.00307349999999997,-0.0196247725843239,-0.0121758528436125));
#14036=CARTESIAN_POINT('Ctrl Pts',(0.00307349999999974,-0.0206246372891225,
-0.0121758545522439));
#14037=CARTESIAN_POINT('Ctrl Pts',(0.00307349976650647,-0.0205952804094407,
-0.0127428527552078));
#14038=CARTESIAN_POINT('Ctrl Pts',(0.00291229877631606,-0.0205659235297588,
-0.0133099896588568));
#14039=CARTESIAN_POINT('Ctrl Pts',(0.00261418979853331,-0.020536566650077,
-0.01379214965395));
#14040=CARTESIAN_POINT('Ctrl Pts',(0.00248924902626763,-0.02052426285686,
-0.0139942282447748));
#14041=CARTESIAN_POINT('Ctrl Pts',(0.00234088438044462,-0.0205119590636431,
-0.0141815521404052));
#14042=CARTESIAN_POINT('Ctrl Pts',(0.00217330663059751,-0.0204996552704261,
-0.0143491320398249));
#14043=CARTESIAN_POINT('Ctrl Pts',(0.00178083356867207,-0.0204708393482553,
-0.0147416101361259));
#14044=CARTESIAN_POINT('Ctrl Pts',(0.00127741589242395,-0.0204420234260845,
-0.0150262640632941));
#14045=CARTESIAN_POINT('Ctrl Pts',(0.000736667807712326,-0.0204132075039136,
-0.0151597639405624));
#14046=CARTESIAN_POINT('Ctrl Pts',(0.00049562834648803,-0.0204003627531857,
-0.015219271758343));
#14047=CARTESIAN_POINT('Ctrl Pts',(0.000247559663784795,-0.0203875180024577,
-0.0152493500093755));
#14048=CARTESIAN_POINT('Ctrl Pts',(4.06901849174428E-8,-0.0203746732517298,
-0.0152493532862887));
#14049=CARTESIAN_POINT('Ctrl Pts',(-0.000557297518273502,-0.0203457507402363,
-0.0152493606649108));
#14050=CARTESIAN_POINT('Ctrl Pts',(-0.00111648816619293,-0.0203168282287427,
-0.015093436186547));
#14051=CARTESIAN_POINT('Ctrl Pts',(-0.00159435775550837,-0.0202879057172492,
-0.0148034806569153));
#14052=CARTESIAN_POINT('Ctrl Pts',(-0.00180482287921371,-0.020275167555844,
-0.0146757773508723));
#14053=CARTESIAN_POINT('Ctrl Pts',(-0.00199966987372288,-0.0202624293944387,
-0.0145227618305072));
#14054=CARTESIAN_POINT('Ctrl Pts',(-0.00217324908559339,-0.0202496912330335,
-0.0143491895840435));
#14055=CARTESIAN_POINT('Ctrl Pts',(-0.00256729371252134,-0.0202207741524419,
-0.0139551607693842));
#14056=CARTESIAN_POINT('Ctrl Pts',(-0.00285241708289534,-0.0201918570718504,
-0.0134495984803389));
#14057=CARTESIAN_POINT('Ctrl Pts',(-0.0029853204821425,-0.0201629399912588,
-0.0129067868463982));
#14058=CARTESIAN_POINT('Ctrl Pts',(-0.00304389025134481,-0.0201501963989516,
-0.0126675728586422));
#14059=CARTESIAN_POINT('Ctrl Pts',(-0.00307349339570498,-0.0201374528066444,
-0.0124214998062665));
#14060=CARTESIAN_POINT('Ctrl Pts',(-0.00307349999888883,-0.0201247092143371,
-0.0121759359326137));
#14061=CARTESIAN_POINT('Ctrl Pts',(-0.00307351498248176,-0.0200957921337456,
-0.0116187154759645));
#14062=CARTESIAN_POINT('Ctrl Pts',(-0.00291766184917668,-0.020066875053154,
-0.0110596216408992));
#14063=CARTESIAN_POINT('Ctrl Pts',(-0.00262781436243296,-0.0200379579725625,
-0.0105818037495013));
#14064=CARTESIAN_POINT('Ctrl Pts',(-0.00250008022998325,-0.0200252143802553,
-0.0103712321329855));
#14065=CARTESIAN_POINT('Ctrl Pts',(-0.0023470098422513,-0.020012470787948,
-0.0101762894566337));
#14066=CARTESIAN_POINT('Ctrl Pts',(-0.00217336596396837,-0.0199997271956408,
-0.0100026338690432));
#14067=CARTESIAN_POINT('Ctrl Pts',(-0.00177926852704949,-0.0199708046841473,
-0.00960850985699746));
#14068=CARTESIAN_POINT('Ctrl Pts',(-0.00127360194940171,-0.0199418821726537,
-0.00932335160670282));
#14069=CARTESIAN_POINT('Ctrl Pts',(-0.000730676576994284,-0.0199129596611602,
-0.00919046989579705));
#14070=CARTESIAN_POINT('Ctrl Pts',(-0.000491559340364625,-0.019900221499755,
-0.0091319456323803));
#14071=CARTESIAN_POINT('Ctrl Pts',(-0.000245589593893761,-0.0198874833383497,
-0.00910236324041321));
#14072=CARTESIAN_POINT('Ctrl Pts',(-1.24601926384675E-7,-0.0198747451769445,
-0.00910235328908382));
#14073=CARTESIAN_POINT('Ctrl Pts',(0.000555159624672213,-0.0198459292547737,
-0.00910233077745721));
#14074=CARTESIAN_POINT('Ctrl Pts',(0.00111246523677488,-0.0198171133326028,
-0.00925712897680344));
#14075=CARTESIAN_POINT('Ctrl Pts',(0.00158914084161407,-0.019788297410432,
-0.00954506754166853));
#14076=CARTESIAN_POINT('Ctrl Pts',(0.00180161987615457,-0.019775452659704,
-0.00967341669075106));
#14077=CARTESIAN_POINT('Ctrl Pts',(0.00199823474569244,-0.0197626079089761,
-0.00982751922627757));
#14078=CARTESIAN_POINT('Ctrl Pts',(0.00217318974903144,-0.0197497631582481,
-0.0100024576565117));
#14079=CARTESIAN_POINT('Ctrl Pts',(0.00257305215909598,-0.0197204062785663,
-0.0104022821884846));
#14080=CARTESIAN_POINT('Ctrl Pts',(0.0028605007836907,-0.0196910493988845,
-0.0109164895181404));
#14081=CARTESIAN_POINT('Ctrl Pts',(0.0029910593252564,-0.0196616925192027,
-0.0114687702908661));
#14082=CARTESIAN_POINT('Ctrl Pts',(0.00304577785513911,-0.0196493887259857,
-0.0117002372757422));
#14083=CARTESIAN_POINT('Ctrl Pts',(0.00307348711766066,-0.0196370849327688,
-0.0119380515063182));
#14084=CARTESIAN_POINT('Ctrl Pts',(0.00307349999548699,-0.0196247811395518,
-0.012175686728761));
#14085=CARTESIAN_POINT('',(0.00307349937524521,-0.0186248572848198,-0.0121772131837633));
#14086=CARTESIAN_POINT('Ctrl Pts',(0.00307349999999997,-0.0196247725843239,
-0.0121758528436125));
#14087=CARTESIAN_POINT('Ctrl Pts',(0.00307350008171438,-0.0195954163064465,
-0.0127428507721285));
#14088=CARTESIAN_POINT('Ctrl Pts',(0.00291229955620968,-0.0195660600285692,
-0.013309987530298));
#14089=CARTESIAN_POINT('Ctrl Pts',(0.00261419109876588,-0.0195367037506918,
-0.0137921475509584));
#14090=CARTESIAN_POINT('Ctrl Pts',(0.00248924695606628,-0.0195243998563183,
-0.0139942319565535));
#14091=CARTESIAN_POINT('Ctrl Pts',(0.00234087759884723,-0.0195120959619448,
-0.0141815608434973));
#14092=CARTESIAN_POINT('Ctrl Pts',(0.00217329417145387,-0.0194997920675713,
-0.0143491444990569));
#14093=CARTESIAN_POINT('Ctrl Pts',(0.00178081915956632,-0.0194709767415835,
-0.0147416200453026));
#14094=CARTESIAN_POINT('Ctrl Pts',(0.00127740025025495,-0.0194421614155956,
-0.0150262710078965));
#14095=CARTESIAN_POINT('Ctrl Pts',(0.000736651773140311,-0.0194133460896077,
-0.0151597678991315));
#14096=CARTESIAN_POINT('Ctrl Pts',(0.000495604489924695,-0.0194005011971331,
-0.015219276273749));
#14097=CARTESIAN_POINT('Ctrl Pts',(0.000247527703741473,-0.0193876563046585,
-0.0152493532008676));
#14098=CARTESIAN_POINT('Ctrl Pts',(1.06400358957003E-9,-0.0193748114121839,
-0.0152493532865579));
#14099=CARTESIAN_POINT('Ctrl Pts',(-0.000557336746359336,-0.0193458894979458,
-0.0152493534795006));
#14100=CARTESIAN_POINT('Ctrl Pts',(-0.00111652506637318,-0.0193169675837076,
-0.0150934220048482));
#14101=CARTESIAN_POINT('Ctrl Pts',(-0.0015943907447657,-0.0192880456694695,
-0.014803460639837));
#14102=CARTESIAN_POINT('Ctrl Pts',(-0.00180486085195263,-0.0192753073652451,
-0.0146757506946925));
#14103=CARTESIAN_POINT('Ctrl Pts',(-0.00199971152818518,-0.0192625690610208,
-0.0145227271382931));
#14104=CARTESIAN_POINT('Ctrl Pts',(-0.00217329266672608,-0.0192498307567964,
-0.0143491460037857));
#14105=CARTESIAN_POINT('Ctrl Pts',(-0.00256732911840163,-0.0192209142729023,
-0.0139551095612665));
#14106=CARTESIAN_POINT('Ctrl Pts',(-0.00285244227892529,-0.0191919977890082,
-0.0134495419197709));
#14107=CARTESIAN_POINT('Ctrl Pts',(-0.00298533489846075,-0.0191630813051141,
-0.0129067279639361));
#14108=CARTESIAN_POINT('Ctrl Pts',(-0.00304390177940186,-0.0191503375705457,
-0.0126675053461888));
#14109=CARTESIAN_POINT('Ctrl Pts',(-0.0030735000793069,-0.0191375938359773,
-0.0124214238050535));
#14110=CARTESIAN_POINT('Ctrl Pts',(-0.00307349999999984,-0.0191248501014089,
-0.0121758522939746));
#14111=CARTESIAN_POINT('Ctrl Pts',(-0.00307349982004621,-0.0190959336175149,
-0.0116186322258037));
#14112=CARTESIAN_POINT('Ctrl Pts',(-0.00291763168036504,-0.0190670171336208,
-0.0110595429415768));
#14113=CARTESIAN_POINT('Ctrl Pts',(-0.00262777150819455,-0.0190381006497267,
-0.0105817331057935));
#14114=CARTESIAN_POINT('Ctrl Pts',(-0.00250002772338218,-0.0190253569151583,
-0.0103711583435332));
#14115=CARTESIAN_POINT('Ctrl Pts',(-0.00234694651141168,-0.0190126131805899,
-0.0101762141856548));
#14116=CARTESIAN_POINT('Ctrl Pts',(-0.00217329126300049,-0.0189998694460215,
-0.0100025591656058));
#14117=CARTESIAN_POINT('Ctrl Pts',(-0.00177918055906308,-0.0189709475317834,
-0.00960844897993668));
#14118=CARTESIAN_POINT('Ctrl Pts',(-0.00127350455405528,-0.0189420256175452,
-0.00932330818517744));
#14119=CARTESIAN_POINT('Ctrl Pts',(-0.000730574967265789,-0.0189131037033071,
-0.00919044502851287));
#14120=CARTESIAN_POINT('Ctrl Pts',(-0.000491448255527693,-0.0189003653990827,
-0.00913192707234067));
#14121=CARTESIAN_POINT('Ctrl Pts',(-0.000245469588832847,-0.0188876270948584,
-0.00910235304303009));
#14122=CARTESIAN_POINT('Ctrl Pts',(3.04917062178946E-9,-0.018874888790634,
-0.00910235328655961));
#14123=CARTESIAN_POINT('Ctrl Pts',(0.000555286857799042,-0.0188460734646461,
-0.00910235383744787));
#14124=CARTESIAN_POINT('Ctrl Pts',(0.00111258570577606,-0.0188172581386582,
-0.00925717495982157));
#14125=CARTESIAN_POINT('Ctrl Pts',(0.00158924916809846,-0.0187884428126704,
-0.00954513297993134));
#14126=CARTESIAN_POINT('Ctrl Pts',(0.00180172953089864,-0.0187755979201957,
-0.00967349487342752));
#14127=CARTESIAN_POINT('Ctrl Pts',(0.00199834367379624,-0.0187627530277211,
-0.00982761111220334));
#14128=CARTESIAN_POINT('Ctrl Pts',(0.00217329557517749,-0.0187499081352465,
-0.0100025634777857));
#14129=CARTESIAN_POINT('Ctrl Pts',(0.0025731383406563,-0.018720551853384,
-0.0104024073041701));
#14130=CARTESIAN_POINT('Ctrl Pts',(0.00286056189175292,-0.0186911955715216,
-0.0109166284047005));
#14131=CARTESIAN_POINT('Ctrl Pts',(0.00299109361119617,-0.0186618392896591,
-0.0114689153408645));
#14132=CARTESIAN_POINT('Ctrl Pts',(0.0030458026512524,-0.0186495353530591,
-0.0117003923201153));
#14133=CARTESIAN_POINT('Ctrl Pts',(0.0030735003947725,-0.0186372314164591,
-0.0119382156415932));
#14134=CARTESIAN_POINT('Ctrl Pts',(0.00307349999999576,-0.0186249274798591,
-0.0121758583923158));
#14135=CARTESIAN_POINT('',(0.00307349990129765,-0.017624751935175,-0.0121753126773873));
#14136=CARTESIAN_POINT('Ctrl Pts',(0.00307349869753639,-0.0186247811395518,
-0.0121786828169311));
#14137=CARTESIAN_POINT('Ctrl Pts',(0.00307297670297644,-0.018595414100554,
-0.0127456848945252));
#14138=CARTESIAN_POINT('Ctrl Pts',(0.00291125166932543,-0.0185660470615561,
-0.0133126766736151));
#14139=CARTESIAN_POINT('Ctrl Pts',(0.00261269539128645,-0.0185366800225583,
-0.0137945642065035));
#14140=CARTESIAN_POINT('Ctrl Pts',(0.00248765278626428,-0.0185243803948895,
-0.0139963903842542));
#14141=CARTESIAN_POINT('Ctrl Pts',(0.00233923178850257,-0.0185120807672206,
-0.014183460423467));
#14142=CARTESIAN_POINT('Ctrl Pts',(0.00217163872964959,-0.0184997811395518,
-0.0143507986830878));
#14143=CARTESIAN_POINT('Ctrl Pts',(0.00177885827015184,-0.0184709550447214,
-0.0147429819808644));
#14144=CARTESIAN_POINT('Ctrl Pts',(0.00127521384053096,-0.0184421289498909,
-0.0150272512926739));
#14145=CARTESIAN_POINT('Ctrl Pts',(0.000734355529584412,-0.0184133028550605,
-0.0151603338454106));
#14146=CARTESIAN_POINT('Ctrl Pts',(0.000493430422115672,-0.0184004622832242,
-0.015219615412637));
#14147=CARTESIAN_POINT('Ctrl Pts',(0.000245508262046727,-0.018387621711388,
-0.0152495013622853));
#14148=CARTESIAN_POINT('Ctrl Pts',(-1.84680271542727E-6,-0.0183747811395518,
-0.0152493527317052));
#14149=CARTESIAN_POINT('Ctrl Pts',(-0.000559193420020552,-0.0183458484419979,
-0.0152490178335656));
#14150=CARTESIAN_POINT('Ctrl Pts',(-0.0011182949906921,-0.0183169157444441,
-0.0150927454132629));
#14151=CARTESIAN_POINT('Ctrl Pts',(-0.0015959901063058,-0.0182879830468902,
-0.0148024895062455));
#14152=CARTESIAN_POINT('Ctrl Pts',(-0.00180623510113311,-0.0182752490777774,
-0.014674740970255));
#14153=CARTESIAN_POINT('Ctrl Pts',(-0.00200086728772786,-0.0182625151086646,
-0.0145217239548106));
#14154=CARTESIAN_POINT('Ctrl Pts',(-0.00217425092061059,-0.0182497811395518,
-0.0143481873272213));
#14155=CARTESIAN_POINT('Ctrl Pts',(-0.00256811967853617,-0.0182208538843402,
-0.0139539710172573));
#14156=CARTESIAN_POINT('Ctrl Pts',(-0.00285301144956077,-0.0181919266291286,
-0.0134482695177798));
#14157=CARTESIAN_POINT('Ctrl Pts',(-0.00298566230667035,-0.0181629993739169,
-0.0129053893312659));
#14158=CARTESIAN_POINT('Ctrl Pts',(-0.00304408104831109,-0.0181502599624619,
-0.0126663077448451));
#14159=CARTESIAN_POINT('Ctrl Pts',(-0.00307356886975759,-0.0181375205510068,
-0.0124203898267037));
#14160=CARTESIAN_POINT('Ctrl Pts',(-0.00307349987853825,-0.0181247811395518,
-0.0121749892116891));
#14161=CARTESIAN_POINT('Ctrl Pts',(-0.00307334322086089,-0.0180958538843402,
-0.0116177604696338));
#14162=CARTESIAN_POINT('Ctrl Pts',(-0.00291731342951439,-0.0180669266291286,
-0.0110587080557867));
#14163=CARTESIAN_POINT('Ctrl Pts',(-0.00262731199399766,-0.0180379993739169,
-0.0105809758818037));
#14164=CARTESIAN_POINT('Ctrl Pts',(-0.00249959688302106,-0.0180252599624619,
-0.0103705851383627));
#14165=CARTESIAN_POINT('Ctrl Pts',(-0.00234658445395589,-0.0180125205510068,
-0.0101758103009194));
#14166=CARTESIAN_POINT('Ctrl Pts',(-0.00217302912958789,-0.0179997811395518,
-0.0100022970641515));
#14167=CARTESIAN_POINT('Ctrl Pts',(-0.00177886463254465,-0.0179708484419979,
-0.00960822815298435));
#14168=CARTESIAN_POINT('Ctrl Pts',(-0.00127314587228529,-0.017941915744444,
-0.00932314669040304));
#14169=CARTESIAN_POINT('Ctrl Pts',(-0.000730192371507065,-0.0179129830468902,
-0.00919035142747428));
#14170=CARTESIAN_POINT('Ctrl Pts',(-0.000491225607494931,-0.0179002490777774,
-0.00913190507025817));
#14171=CARTESIAN_POINT('Ctrl Pts',(-0.000245420214478279,-0.0178875151086646,
-0.00910236275876294));
#14172=CARTESIAN_POINT('Ctrl Pts',(-1.18653065741516E-7,-0.0178747811395518,
-0.00910235328884841));
#14173=CARTESIAN_POINT('Ctrl Pts',(0.000555174516620966,-0.0178459550447214,
-0.00910233185164749));
#14174=CARTESIAN_POINT('Ctrl Pts',(0.00111248697751199,-0.0178171289498909,
-0.00925713590221569));
#14175=CARTESIAN_POINT('Ctrl Pts',(0.00158916594125725,-0.0177883028550605,
-0.00954508270341179));
#14176=CARTESIAN_POINT('Ctrl Pts',(0.00180150238546827,-0.0177754622832242,
-0.00967334848507651));
#14177=CARTESIAN_POINT('Ctrl Pts',(0.00199799566702671,-0.017762621711388,
-0.00982733305485337));
#14178=CARTESIAN_POINT('Ctrl Pts',(0.00217286130198874,-0.0177497811395518,
-0.0100021292902053));
#14179=CARTESIAN_POINT('Ctrl Pts',(0.00257278787744105,-0.017720414100554,
-0.0104018971452298));
#14180=CARTESIAN_POINT('Ctrl Pts',(0.00286031494897729,-0.0176910470615562,
-0.0109160658455345));
#14181=CARTESIAN_POINT('Ctrl Pts',(0.0029909554462368,-0.0176616800225583,
-0.0114683310122611));
#14182=CARTESIAN_POINT('Ctrl Pts',(0.00304567085267882,-0.0176493803948895,
-0.0116996330487283));
#14183=CARTESIAN_POINT('Ctrl Pts',(0.00307341470433931,-0.0176370807672207,
-0.0119372776082813));
#14184=CARTESIAN_POINT('Ctrl Pts',(0.00307349980266144,-0.0176247811395518,
-0.0121747519055697));
#14185=CARTESIAN_POINT('',(0.00307349956938691,-0.0166247219214524,-0.0121746998012189));
#14186=CARTESIAN_POINT('Ctrl Pts',(0.00307349999993387,-0.0176247227307983,
-0.0121758734492049));
#14187=CARTESIAN_POINT('Ctrl Pts',(0.0030734962803204,-0.017595359946596,
-0.0127428740067176));
#14188=CARTESIAN_POINT('Ctrl Pts',(0.0029122905308065,-0.0175659971623937,
-0.0133100118969287));
#14189=CARTESIAN_POINT('Ctrl Pts',(0.00261417645067601,-0.0175366343781914,
-0.0137921712425095));
#14190=CARTESIAN_POINT('Ctrl Pts',(0.00248928246725899,-0.0175243329294251,
-0.0139941704278045));
#14191=CARTESIAN_POINT('Ctrl Pts',(0.00234098296327957,-0.0175120314806588,
-0.0141814262629012));
#14192=CARTESIAN_POINT('Ctrl Pts',(0.00217348357710258,-0.0174997300318925,
-0.0143489550766419));
#14193=CARTESIAN_POINT('Ctrl Pts',(0.00178103880370149,-0.017470908199265,
-0.0147414687977199));
#14194=CARTESIAN_POINT('Ctrl Pts',(0.00127763942897038,-0.0174420863666376,
-0.015026164674513));
#14195=CARTESIAN_POINT('Ctrl Pts',(0.000736897654871983,-0.0174132645340101,
-0.0151597071865076));
#14196=CARTESIAN_POINT('Ctrl Pts',(0.000495954532555534,-0.017400422133669,
-0.0152192109114707));
#14197=CARTESIAN_POINT('Ctrl Pts',(0.000247985299515979,-0.0173875797333278,
-0.0152493081466551));
#14198=CARTESIAN_POINT('Ctrl Pts',(5.6009102431774E-7,-0.0173747373329867,
-0.0152493532355248));
#14199=CARTESIAN_POINT('Ctrl Pts',(-0.000556782977434645,-0.0173458089030335,
-0.0152494548014448));
#14200=CARTESIAN_POINT('Ctrl Pts',(-0.00111600385162446,-0.0173168804730803,
-0.0150936222173342));
#14201=CARTESIAN_POINT('Ctrl Pts',(-0.00159392454543696,-0.0172879520431271,
-0.0148037434656663));
#14202=CARTESIAN_POINT('Ctrl Pts',(-0.00180433015069223,-0.0172752162401117,
-0.0146761237266909));
#14203=CARTESIAN_POINT('Ctrl Pts',(-0.00199913382837564,-0.0172624804370963,
-0.0145232086804128));
#14204=CARTESIAN_POINT('Ctrl Pts',(-0.0021726914140132,-0.0172497446340809,
-0.014349747090191));
#14205=CARTESIAN_POINT('Ctrl Pts',(-0.00256684047077401,-0.017220821641593,
-0.0139558160388974));
#14206=CARTESIAN_POINT('Ctrl Pts',(-0.00285209442065788,-0.017191898649105,
-0.0134503224554305));
#14207=CARTESIAN_POINT('Ctrl Pts',(-0.00298513579568746,-0.0171629756566171,
-0.0129075407412171));
#14208=CARTESIAN_POINT('Ctrl Pts',(-0.00304374356782033,-0.0171502344161364,
-0.0126684329672826));
#14209=CARTESIAN_POINT('Ctrl Pts',(-0.00307340871282563,-0.0171374931756557,
-0.0124224640790486));
#14210=CARTESIAN_POINT('Ctrl Pts',(-0.00307349978845192,-0.017124751935175,
-0.0121769936312336));
#14211=CARTESIAN_POINT('Ctrl Pts',(-0.00307370653281557,-0.0170958289426871,
-0.0116197684592478));
#14212=CARTESIAN_POINT('Ctrl Pts',(-0.00291804326889372,-0.0170669059501992,
-0.0110606172375488));
#14213=CARTESIAN_POINT('Ctrl Pts',(-0.00262835635395399,-0.0170379829577112,
-0.010582697573318));
#14214=CARTESIAN_POINT('Ctrl Pts',(-0.00250074263456118,-0.0170252417172306,
-0.0103721630176369));
#14215=CARTESIAN_POINT('Ctrl Pts',(-0.00234780681771066,-0.0170125004767499,
-0.0101772367700652));
#14216=CARTESIAN_POINT('Ctrl Pts',(-0.00217430395267995,-0.0169997592362692,
-0.0100035723260559));
#14217=CARTESIAN_POINT('Ctrl Pts',(-0.00178037327651628,-0.016970830806316,
-0.00960927479187941));
#14218=CARTESIAN_POINT('Ctrl Pts',(-0.00127482527644342,-0.0169419023763628,
-0.00932389735964255));
#14219=CARTESIAN_POINT('Ctrl Pts',(-0.000731953004829246,-0.0169129739464096,
-0.00919078259246701));
#14220=CARTESIAN_POINT('Ctrl Pts',(-0.000492952328850823,-0.0169002381433942,
-0.00913217853217292));
#14221=CARTESIAN_POINT('Ctrl Pts',(-0.000247092039078856,-0.0168875023403788,
-0.00910249113135262));
#14222=CARTESIAN_POINT('Ctrl Pts',(-1.72059828612464E-6,-0.0168747665373634,
-0.00910235376816842));
#14223=CARTESIAN_POINT('Ctrl Pts',(0.000553568659056523,-0.0168459447047359,
-0.00910204290762045));
#14224=CARTESIAN_POINT('Ctrl Pts',(0.00111095867085604,-0.0168171228721085,
-0.00925655441912994));
#14225=CARTESIAN_POINT('Ctrl Pts',(0.00158778597419169,-0.016788301039481,
-0.00954424960245972));
#14226=CARTESIAN_POINT('Ctrl Pts',(0.00180025015723536,-0.0167754586391399,
-0.00967244050441554));
#14227=CARTESIAN_POINT('Ctrl Pts',(0.0019968755877652,-0.0167626162387987,
-0.0098263732388435));
#14228=CARTESIAN_POINT('Ctrl Pts',(0.00217187042956542,-0.0167497738384576,
-0.0100011392623289));
#14229=CARTESIAN_POINT('Ctrl Pts',(0.00257197754660007,-0.0167204110542553,
-0.0104007232105927));
#14230=CARTESIAN_POINT('Ctrl Pts',(0.00285973859300779,-0.016691048270053,
-0.0109147587619568));
#14231=CARTESIAN_POINT('Ctrl Pts',(0.00299063140450493,-0.0166616854858507,
-0.0114669625669201));
#14232=CARTESIAN_POINT('Ctrl Pts',(0.00304546854812922,-0.0166493840370844,
-0.0116983066645546));
#14233=CARTESIAN_POINT('Ctrl Pts',(0.0030733213116782,-0.0166370825883181,
-0.011936009349354));
#14234=CARTESIAN_POINT('Ctrl Pts',(0.00307349913877991,-0.0166247811395518,
-0.0121735524347227));
#14235=CARTESIAN_POINT('',(0.00307390633487226,-0.0156241056269589,-0.0121772501359052));
#14236=CARTESIAN_POINT('Ctrl Pts',(0.00307349999999391,-0.0166246627033529,
-0.0121758471677152));
#14237=CARTESIAN_POINT('Ctrl Pts',(0.00307350112877669,-0.0165953700180398,
-0.0127428357199062));
#14238=CARTESIAN_POINT('Ctrl Pts',(0.00291230682244614,-0.0165660689951853,
-0.0133099641739799));
#14239=CARTESIAN_POINT('Ctrl Pts',(0.002614208497438,-0.0165367543867582,
-0.0137921194100424));
#14240=CARTESIAN_POINT('Ctrl Pts',(0.00248926772237858,-0.0165244678705648,
-0.0139942032321872));
#14241=CARTESIAN_POINT('Ctrl Pts',(0.00234090209310256,-0.0165121789678393,
-0.0141815319419045));
#14242=CARTESIAN_POINT('Ctrl Pts',(0.00217332274698239,-0.0164998872921877,
-0.0143491159231138));
#14243=CARTESIAN_POINT('Ctrl Pts',(0.00178084467378571,-0.0164710996564333,
-0.0147416048518896));
#14244=CARTESIAN_POINT('Ctrl Pts',(0.00127741700944676,-0.0164422968107177,
-0.0150262660493983));
#14245=CARTESIAN_POINT('Ctrl Pts',(0.000736656043588142,-0.01641349364647,
-0.0151597668448645));
#14246=CARTESIAN_POINT('Ctrl Pts',(0.000495625379421995,-0.0164006553570093,
-0.0152192714826426));
#14247=CARTESIAN_POINT('Ctrl Pts',(0.000247565780935063,-0.0163878170042657,
-0.0152493488464267));
#14248=CARTESIAN_POINT('Ctrl Pts',(5.5129846927282E-8,-0.0163749799069125,
-0.0152493532860637));
#14249=CARTESIAN_POINT('Ctrl Pts',(-0.000557318558336918,-0.0163460718164288,
-0.0152493632837621));
#14250=CARTESIAN_POINT('Ctrl Pts',(-0.00111654073205856,-0.0163171700921992,
-0.0150934222221862));
#14251=CARTESIAN_POINT('Ctrl Pts',(-0.0015944298199754,-0.0162882195180373,
-0.0148034369292179));
#14252=CARTESIAN_POINT('Ctrl Pts',(-0.00180486528662487,-0.0162754713140344,
-0.0146757437217557));
#14253=CARTESIAN_POINT('Ctrl Pts',(-0.00199968605253971,-0.0162627136379023,
-0.0145227449648848));
#14254=CARTESIAN_POINT('Ctrl Pts',(-0.00217324478123971,-0.0162499417750734,
-0.0143491938882159));
#14255=CARTESIAN_POINT('Ctrl Pts',(-0.00256704881673858,-0.0162209624712921,
-0.0139554072151439));
#14256=CARTESIAN_POINT('Ctrl Pts',(-0.00285208114276245,-0.016191910129541,
-0.0134501990338245));
#14257=CARTESIAN_POINT('Ctrl Pts',(-0.0029850804100728,-0.0161629900239187,
-0.0129077666662688));
#14258=CARTESIAN_POINT('Ctrl Pts',(-0.00304381105415618,-0.0161502193037148,
-0.0126682360059692));
#14259=CARTESIAN_POINT('Ctrl Pts',(-0.0030734935682315,-0.0161374743693433,
-0.0124218235040799));
#14260=CARTESIAN_POINT('Ctrl Pts',(-0.00307349999894891,-0.0161247728966703,
-0.0121759336673099));
#14261=CARTESIAN_POINT('Ctrl Pts',(-0.00307351459136934,-0.0160959510378268,
-0.011617966701677));
#14262=CARTESIAN_POINT('Ctrl Pts',(-0.00291725659147299,-0.0160673529699291,
-0.0110582110209378));
#14263=CARTESIAN_POINT('Ctrl Pts',(-0.00262671455400442,-0.0160387229375742,
-0.0105799921078269));
#14264=CARTESIAN_POINT('Ctrl Pts',(-0.00249926631704068,-0.0160261641795383,
-0.0103702181353934));
#14265=CARTESIAN_POINT('Ctrl Pts',(-0.00234666050317676,-0.0160135992709085,
-0.0101759774061611));
#14266=CARTESIAN_POINT('Ctrl Pts',(-0.00217360002710924,-0.0160010066243327,
-0.0100028679731814));
#14267=CARTESIAN_POINT('Ctrl Pts',(-0.00177991703981202,-0.0159723605068909,
-0.00960907361728126));
#14268=CARTESIAN_POINT('Ctrl Pts',(-0.00127479307298006,-0.0159435708498243,
-0.00932397045489184));
#14269=CARTESIAN_POINT('Ctrl Pts',(-0.000732373258603867,-0.0159147081592691,
-0.00919088567197968));
#14270=CARTESIAN_POINT('Ctrl Pts',(-0.000492770773530023,-0.015901958675936,
-0.00913209828282809));
#14271=CARTESIAN_POINT('Ctrl Pts',(-0.000246268960427492,-0.0158891949419885,
-0.00910237570626738));
#14272=CARTESIAN_POINT('Ctrl Pts',(-2.79962873519633E-7,-0.0158764230344964,
-0.0091023532993089));
#14273=CARTESIAN_POINT('Ctrl Pts',(0.00055505745979561,-0.0158475895571469,
-0.00910230271402786));
#14274=CARTESIAN_POINT('Ctrl Pts',(0.00111241738463871,-0.0158187144223219,
-0.00925710145582043));
#14275=CARTESIAN_POINT('Ctrl Pts',(0.00158913524431839,-0.0157897785602021,
-0.0095450641605989));
#14276=CARTESIAN_POINT('Ctrl Pts',(0.00180162169350743,-0.0157768810392236,
-0.00967341717149378));
#14277=CARTESIAN_POINT('Ctrl Pts',(0.00199824333142999,-0.0157639714533495,
-0.00982752549781976));
#14278=CARTESIAN_POINT('Ctrl Pts',(0.00217320411947251,-0.0157510481138661,
-0.0100024720256865));
#14279=CARTESIAN_POINT('Ctrl Pts',(0.00257308049831668,-0.0157215115631165,
-0.0104023158126139));
#14280=CARTESIAN_POINT('Ctrl Pts',(0.00286053074137381,-0.015691903168991,
-0.0109165483225608));
#14281=CARTESIAN_POINT('Ctrl Pts',(0.00299107879379126,-0.0156622296518079,
-0.0114688526505384));
#14282=CARTESIAN_POINT('Ctrl Pts',(0.00304579761884114,-0.0156497920859822,
-0.011700349354911));
#14283=CARTESIAN_POINT('Ctrl Pts',(0.00307350041344759,-0.0156373430790635,
-0.0119381941485527));
#14284=CARTESIAN_POINT('Ctrl Pts',(0.00307349999999535,-0.0156248831259193,
-0.0121758586333623));
#14285=CARTESIAN_POINT('',(0.00307349980039059,-0.0146248225157206,-0.012176624660313));
#14286=CARTESIAN_POINT('Ctrl Pts',(0.00307349936069457,-0.0156247811395518,
-0.012177835661408));
#14287=CARTESIAN_POINT('Ctrl Pts',(0.00307313365158047,-0.0155954195670811,
-0.0127448357564998));
#14288=CARTESIAN_POINT('Ctrl Pts',(0.00291156604386341,-0.0155660579946104,
-0.0133118703234303));
#14289=CARTESIAN_POINT('Ctrl Pts',(0.00261314451277681,-0.0155366964221397,
-0.0137938390730669));
#14290=CARTESIAN_POINT('Ctrl Pts',(0.00248811455764909,-0.0155243947759578,
-0.0139957699824105));
#14291=CARTESIAN_POINT('Ctrl Pts',(0.00233968582882625,-0.0155120931297759,
-0.0141829409193754));
#14292=CARTESIAN_POINT('Ctrl Pts',(0.00217206790103134,-0.015499791483594,
-0.0143503700796202));
#14293=CARTESIAN_POINT('Ctrl Pts',(0.00177936812662347,-0.0154709708571608,
-0.0147426276043517));
#14294=CARTESIAN_POINT('Ctrl Pts',(0.00127578416642009,-0.0154421502307276,
-0.0150269954458057));
#14295=CARTESIAN_POINT('Ctrl Pts',(0.000734956205693867,-0.0154133296042945,
-0.0151601859800948));
#14296=CARTESIAN_POINT('Ctrl Pts',(0.000493960994275608,-0.0154004870120751,
-0.0152195362417322));
#14297=CARTESIAN_POINT('Ctrl Pts',(0.000245958020913104,-0.0153876444198556,
-0.0152494721514421));
#14298=CARTESIAN_POINT('Ctrl Pts',(-1.48088146134381E-6,-0.0153748018276362,
-0.0152493529297971));
#14299=CARTESIAN_POINT('Ctrl Pts',(-0.000558823182087959,-0.0153458746063105,
-0.0152490843897039));
#14300=CARTESIAN_POINT('Ctrl Pts',(-0.00111793988359,-0.0153169473849847,
-0.0150928808685131));
#14301=CARTESIAN_POINT('Ctrl Pts',(-0.00159566766821423,-0.015288020163659,
-0.0148026853981739));
#14302=CARTESIAN_POINT('Ctrl Pts',(-0.00180600034135376,-0.0152752841663321,
-0.0146749189358203));
#14303=CARTESIAN_POINT('Ctrl Pts',(-0.00200071254666846,-0.0152625481690053,
-0.0145218646740806));
#14304=CARTESIAN_POINT('Ctrl Pts',(-0.00217416235453008,-0.0152498121716784,
-0.0143482759678391));
#14305=CARTESIAN_POINT('Ctrl Pts',(-0.00256804419217434,-0.0152208903867933,
-0.0139540787101331));
#14306=CARTESIAN_POINT('Ctrl Pts',(-0.00285295579622096,-0.0151919686019082,
-0.0134483928164419));
#14307=CARTESIAN_POINT('Ctrl Pts',(-0.00298562993797293,-0.0151630468170231,
-0.0129055217890164));
#14308=CARTESIAN_POINT('Ctrl Pts',(-0.00304407926247028,-0.0151503053832556,
-0.0126663610571421));
#14309=CARTESIAN_POINT('Ctrl Pts',(-0.00307357806885326,-0.0151375639494881,
-0.0124203580177665));
#14310=CARTESIAN_POINT('Ctrl Pts',(-0.00307349984395625,-0.0151248225157206,
-0.0121748738985247));
#14311=CARTESIAN_POINT('Ctrl Pts',(-0.00307332228123565,-0.0150959007308355,
-0.0116176494119419));
#14312=CARTESIAN_POINT('Ctrl Pts',(-0.00291727379124065,-0.0150669789459504,
-0.011058606234676));
#14313=CARTESIAN_POINT('Ctrl Pts',(-0.00262725790115753,-0.0150380571610653,
-0.0105808867756854));
#14314=CARTESIAN_POINT('Ctrl Pts',(-0.00249949198803375,-0.0150253157272978,
-0.0103704284353599));
#14315=CARTESIAN_POINT('Ctrl Pts',(-0.00234641189170714,-0.0150125742935303,
-0.0101755976081592));
#14316=CARTESIAN_POINT('Ctrl Pts',(-0.0021727774036934,-0.0149998328597628,
-0.0100020454284438));
#14317=CARTESIAN_POINT('Ctrl Pts',(-0.00177857033436272,-0.0149709056384371,
-0.0096080252258667));
#14318=CARTESIAN_POINT('Ctrl Pts',(-0.00127282265264435,-0.0149419784171113,
-0.00932300314062889));
#14319=CARTESIAN_POINT('Ctrl Pts',(-0.000729857634045862,-0.0149130511957856,
-0.00919026957746116));
#14320=CARTESIAN_POINT('Ctrl Pts',(-0.000490802491224546,-0.0149003151984587,
-0.00913183000987696));
#14321=CARTESIAN_POINT('Ctrl Pts',(-0.000244907263889183,-0.0148875792011319,
-0.00910231516908718));
#14322=CARTESIAN_POINT('Ctrl Pts',(4.7789457918649E-7,-0.014874843203805,
-0.0091023533237117));
#14323=CARTESIAN_POINT('Ctrl Pts',(0.000555766483525987,-0.0148460225773718,
-0.00910243966482436));
#14324=CARTESIAN_POINT('Ctrl Pts',(0.00111304523135227,-0.0148172019509386,
-0.00925734944151976));
#14325=CARTESIAN_POINT('Ctrl Pts',(0.00158966629488911,-0.0147883813245055,
-0.00954538501628879));
#14326=CARTESIAN_POINT('Ctrl Pts',(0.00180205064317471,-0.014775538732286,
-0.00967373487849681));
#14327=CARTESIAN_POINT('Ctrl Pts',(0.00199857606672519,-0.0147626961400666,
-0.00982781813059075));
#14328=CARTESIAN_POINT('Ctrl Pts',(0.00217345330382419,-0.0147498535478472,
-0.0100027212182991));
#14329=CARTESIAN_POINT('Ctrl Pts',(0.00257326905619171,-0.0147204919753765,
-0.0104025960720167));
#14330=CARTESIAN_POINT('Ctrl Pts',(0.0028606556848834,-0.0146911304029058,
-0.0109168406083762));
#14331=CARTESIAN_POINT('Ctrl Pts',(0.00299114651727006,-0.0146617688304351,
-0.0114691392268259));
#14332=CARTESIAN_POINT('Ctrl Pts',(0.00304581838648291,-0.0146494671842532,
-0.0117005363087668));
#14333=CARTESIAN_POINT('Ctrl Pts',(0.00307349817590678,-0.0146371655380713,
-0.0119382730645528));
#14334=CARTESIAN_POINT('Ctrl Pts',(0.0030734999999094,-0.0146248638918894,
-0.0121758296876704));
#14335=CARTESIAN_POINT('',(0.00307349954753674,-0.0136246902846469,-0.0121748470396884));
#14336=CARTESIAN_POINT('Ctrl Pts',(0.00307349960087178,-0.0146247811395518,
-0.0121774196329556));
#14337=CARTESIAN_POINT('Ctrl Pts',(0.00307321063952067,-0.0145954134790752,
-0.0127444223079151));
#14338=CARTESIAN_POINT('Ctrl Pts',(0.00291171841574269,-0.0145660458185986,
-0.0133114808685064));
#14339=CARTESIAN_POINT('Ctrl Pts',(0.00261335982369163,-0.014536678158122,
-0.0137934912812635));
#14340=CARTESIAN_POINT('Ctrl Pts',(0.00248840897262105,-0.014524379151932,
-0.0139953544516346));
#14341=CARTESIAN_POINT('Ctrl Pts',(0.00234007700429877,-0.0145120801457419,
-0.0141824731954777));
#14342=CARTESIAN_POINT('Ctrl Pts',(0.002172567261298,-0.0144997811395518,
-0.0143498711671506));
#14343=CARTESIAN_POINT('Ctrl Pts',(0.00177995363344448,-0.0144709544136982,
-0.014742222822502));
#14344=CARTESIAN_POINT('Ctrl Pts',(0.00127642974412018,-0.0144421276878447,
-0.0150267073464758));
#14345=CARTESIAN_POINT('Ctrl Pts',(0.000735627476184249,-0.0144133009619911,
-0.0151600205851998));
#14346=CARTESIAN_POINT('Ctrl Pts',(0.000494744444681753,-0.014400461021178,
-0.015219400693212));
#14347=CARTESIAN_POINT('Ctrl Pts',(0.000246852814080745,-0.0143876210803649,
-0.0152493922895258));
#14348=CARTESIAN_POINT('Ctrl Pts',(-4.85139050949205E-7,-0.0143747811395518,
-0.0152493532482695));
#14349=CARTESIAN_POINT('Ctrl Pts',(-0.000557832740682571,-0.0143458478111779,
-0.0152492652732931));
#14350=CARTESIAN_POINT('Ctrl Pts',(-0.00111700420073623,-0.0143169144828041,
-0.0150932400919133));
#14351=CARTESIAN_POINT('Ctrl Pts',(-0.00159482824846356,-0.0142879811544302,
-0.0148031951196477));
#14352=CARTESIAN_POINT('Ctrl Pts',(-0.00180511498649533,-0.0142752478161374,
-0.0146755485279988));
#14353=CARTESIAN_POINT('Ctrl Pts',(-0.00199980229410829,-0.0142625144778446,
-0.0145226301155781));
#14354=CARTESIAN_POINT('Ctrl Pts',(-0.0021732534721906,-0.0142497811395518,
-0.0143491851976134));
#14355=CARTESIAN_POINT('Ctrl Pts',(-0.00256730376778178,-0.0142208532546356,
-0.0139551491238987));
#14356=CARTESIAN_POINT('Ctrl Pts',(-0.00285242781397656,-0.0141919253697195,
-0.0134495776419844));
#14357=CARTESIAN_POINT('Ctrl Pts',(-0.00298532763319761,-0.0141629974848033,
-0.012906757639033));
#14358=CARTESIAN_POINT('Ctrl Pts',(-0.0030438518494217,-0.0141502587030528,
-0.0126677195770576));
#14359=CARTESIAN_POINT('Ctrl Pts',(-0.00307345235301464,-0.0141375199213023,
-0.0124218328862067));
#14360=CARTESIAN_POINT('Ctrl Pts',(-0.00307349994219986,-0.0141247811395518,
-0.0121764493549137));
#14361=CARTESIAN_POINT('Ctrl Pts',(-0.00307360801018469,-0.0140958532546356,
-0.0116192197318156));
#14362=CARTESIAN_POINT('Ctrl Pts',(-0.00291784336291199,-0.0140669253697195,
-0.01106009256286));
#14363=CARTESIAN_POINT('Ctrl Pts',(-0.00262806820907844,-0.0140379974848033,
-0.0105822222946308));
#14364=CARTESIAN_POINT('Ctrl Pts',(-0.00250046183716071,-0.0140252587030528,
-0.0103717857186533));
#14365=CARTESIAN_POINT('Ctrl Pts',(-0.00234755430279202,-0.0140125199213023,
-0.0101769508500219));
#14366=CARTESIAN_POINT('Ctrl Pts',(-0.00217409629185899,-0.0139997811395518,
-0.0100033644917136));
#14367=CARTESIAN_POINT('Ctrl Pts',(-0.00178012474201237,-0.0139708478111779,
-0.00960910142915965));
#14368=CARTESIAN_POINT('Ctrl Pts',(-0.00127454520834623,-0.0139419144828041,
-0.00932377147832942));
#14369=CARTESIAN_POINT('Ctrl Pts',(-0.000731656198816013,-0.0139129811544302,
-0.00919070982991583));
#14370=CARTESIAN_POINT('Ctrl Pts',(-0.000492734864759313,-0.0139002478161374,
-0.00913215040802171));
#14371=CARTESIAN_POINT('Ctrl Pts',(-0.000246961692959371,-0.0138875144778446,
-0.00910248760127359));
#14372=CARTESIAN_POINT('Ctrl Pts',(-1.67727568855383E-6,-0.0138747811395518,
-0.00910235374422101));
#14373=CARTESIAN_POINT('Ctrl Pts',(0.000553616747781886,-0.0138459544136982,
-0.00910205070816952));
#14374=CARTESIAN_POINT('Ctrl Pts',(0.00111100838919363,-0.0138171276878447,
-0.00925657261563487));
#14375=CARTESIAN_POINT('Ctrl Pts',(0.00158783372454616,-0.0137883009619911,
-0.0095442784133702));
#14376=CARTESIAN_POINT('Ctrl Pts',(0.00180022028260421,-0.013775461021178,
-0.00967242773678896));
#14377=CARTESIAN_POINT('Ctrl Pts',(0.00199677892354685,-0.0137626210803649,
-0.00982630026110334));
#14378=CARTESIAN_POINT('Ctrl Pts',(0.00217172384864896,-0.0137497811395518,
-0.0100009928829438));
#14379=CARTESIAN_POINT('Ctrl Pts',(0.00257185989579124,-0.0137204134790752,
-0.0104005518591608));
#14380=CARTESIAN_POINT('Ctrl Pts',(0.00285965598737614,-0.0136910458185987,
-0.0109145705767058));
#14381=CARTESIAN_POINT('Ctrl Pts',(0.00299058522067098,-0.0136616781581221,
-0.0114667677572287));
#14382=CARTESIAN_POINT('Ctrl Pts',(0.00304541762558932,-0.013649379151932,
-0.0116980247396096));
#14383=CARTESIAN_POINT('Ctrl Pts',(0.00307328564276539,-0.0136370801457419,
-0.0119356374308079));
#14384=CARTESIAN_POINT('Ctrl Pts',(0.00307349876212316,-0.0136247811395518,
-0.0121730948037442));
#14385=CARTESIAN_POINT('',(-0.00289832479094502,-0.0131787743898721,-0.0131986512412849));
#14386=CARTESIAN_POINT('Ctrl Pts',(0.00307349999999835,-0.0136246379448887,
-0.0121758564690173));
#14387=CARTESIAN_POINT('Ctrl Pts',(0.00307349925680341,-0.0135874826486382,
-0.0128936063191386));
#14388=CARTESIAN_POINT('Ctrl Pts',(0.00254975520022809,-0.0135131720561371,
-0.0143255433828562));
#14389=CARTESIAN_POINT('Ctrl Pts',(0.000563092149707625,-0.0134017061673856,
-0.0154635975636764));
#14390=CARTESIAN_POINT('Ctrl Pts',(-0.00168906107875945,-0.013290240278634,
-0.0150515256885247));
#14391=CARTESIAN_POINT('Ctrl Pts',(-0.00265947231698363,-0.0132159296861329,
-0.0138754926872979));
#14392=CARTESIAN_POINT('Ctrl Pts',(-0.00289832479094299,-0.0131787743898824,
-0.0131986512412907));
#14393=CARTESIAN_POINT('',(-0.00132721716346492,-0.0131811320840746,-0.00940066304710818));
#14394=CARTESIAN_POINT('Origin',(0.,-0.0131787743898824,-0.012175853286568));
#14395=CARTESIAN_POINT('',(0.00307349448959333,-0.0138578957495471,-0.0121758980191793));
#14396=CARTESIAN_POINT('Ctrl Pts',(-0.00132669617051746,-0.0131812255681309,
-0.00940188040761344));
#14397=CARTESIAN_POINT('Ctrl Pts',(-0.0018196919059704,-0.013209392323556,
-0.00963774239526866));
#14398=CARTESIAN_POINT('Ctrl Pts',(-0.00224604746585449,-0.0132329816360925,
-0.0100099352992059));
#14399=CARTESIAN_POINT('Ctrl Pts',(-0.00255047574633007,-0.0132616754020662,
-0.010462835535099));
#14400=CARTESIAN_POINT('Ctrl Pts',(-0.0028069991368114,-0.0132858539117688,
-0.0108444673068898));
#14401=CARTESIAN_POINT('Ctrl Pts',(-0.00297896355371799,-0.013313136885812,
-0.0112851249369724));
#14402=CARTESIAN_POINT('Ctrl Pts',(-0.00304385678131681,-0.0133371739441656,
-0.0117402552548227));
#14403=CARTESIAN_POINT('Ctrl Pts',(-0.00305597537574073,-0.0133416627848677,
-0.0118252493279509));
#14404=CARTESIAN_POINT('Ctrl Pts',(-0.00306438599299585,-0.0133460384264664,
-0.0119107898015695));
#14405=CARTESIAN_POINT('Ctrl Pts',(-0.0030692671948678,-0.0133502595110746,
-0.0119966084976508));
#14406=CARTESIAN_POINT('Ctrl Pts',(-0.00310028648940561,-0.0133770838609308,
-0.0125419732419139));
#14407=CARTESIAN_POINT('Ctrl Pts',(-0.00298081293685468,-0.0134022194800802,
-0.0130948328051767));
#14408=CARTESIAN_POINT('Ctrl Pts',(-0.00273221661189375,-0.0134317107918798,
-0.0135805976612059));
#14409=CARTESIAN_POINT('Ctrl Pts',(-0.00255384908424496,-0.013452870768294,
-0.0139291332898087));
#14410=CARTESIAN_POINT('Ctrl Pts',(-0.00230883215863813,-0.0134753555341454,
-0.0142457915368782));
#14411=CARTESIAN_POINT('Ctrl Pts',(-0.00201232942765066,-0.0134960192056483,
-0.0145016804695592));
#14412=CARTESIAN_POINT('Ctrl Pts',(-0.00189558715694983,-0.0135041551304819,
-0.01460243183515));
#14413=CARTESIAN_POINT('Ctrl Pts',(-0.00177086859135001,-0.0135120087420253,
-0.0146938583727293));
#14414=CARTESIAN_POINT('Ctrl Pts',(-0.00164017617792611,-0.0135193880226992,
-0.0147758852505195));
#14415=CARTESIAN_POINT('Ctrl Pts',(-0.00117755037596263,-0.0135455092454253,
-0.0150662444926982));
#14416=CARTESIAN_POINT('Ctrl Pts',(-0.000636279900124425,-0.0135718670537832,
-0.0152296424015862));
#14417=CARTESIAN_POINT('Ctrl Pts',(-9.08461531836337E-5,-0.0136020240639464,
-0.0152471101049117));
#14418=CARTESIAN_POINT('Ctrl Pts',(0.000232536519338722,-0.0136199038790413,
-0.0152574665462135));
#14419=CARTESIAN_POINT('Ctrl Pts',(0.000558965697174523,-0.0136378116522388,
-0.0152183595818082));
#14420=CARTESIAN_POINT('Ctrl Pts',(0.000869600935216467,-0.0136548250124208,
-0.0151265683100328));
#14421=CARTESIAN_POINT('Ctrl Pts',(0.00108289896946619,-0.0136665072552522,
-0.0150635397304216));
#14422=CARTESIAN_POINT('Ctrl Pts',(0.00128876025895534,-0.0136777677915046,
-0.014975755649426));
#14423=CARTESIAN_POINT('Ctrl Pts',(0.00148321885597551,-0.0136883080044757,
-0.0148679674384441));
#14424=CARTESIAN_POINT('Ctrl Pts',(0.00196087599623186,-0.0137141983896922,
-0.0146032025506996));
#14425=CARTESIAN_POINT('Ctrl Pts',(0.00236635307333829,-0.0137418711774504,
-0.0142092494390052));
#14426=CARTESIAN_POINT('Ctrl Pts',(0.00264532404574679,-0.0137724708213245,
-0.0137401927099414));
#14427=CARTESIAN_POINT('Ctrl Pts',(0.002775992199874,-0.0137868034916645,
-0.0135204896475096));
#14428=CARTESIAN_POINT('Ctrl Pts',(0.00288080040326081,-0.0138005638977075,
-0.0132846571839918));
#14429=CARTESIAN_POINT('Ctrl Pts',(0.00295272353125746,-0.0138138184898977,
-0.0130390338119726));
#14430=CARTESIAN_POINT('Ctrl Pts',(0.00303435323401673,-0.0138288618904118,
-0.0127602616922508));
#14431=CARTESIAN_POINT('Ctrl Pts',(0.00307355007668885,-0.0138432537375257,
-0.0124689291532911));
#14432=CARTESIAN_POINT('Ctrl Pts',(0.00307310808197872,-0.0138570911799035,
-0.0121785284790189));
#14433=CARTESIAN_POINT('',(0.00307349989340788,-0.0148577382240435,-0.0121752793767589));
#14434=CARTESIAN_POINT('Ctrl Pts',(0.00307349999999152,-0.01385790722318,
-0.0121758605072862));
#14435=CARTESIAN_POINT('Ctrl Pts',(0.00307350133207145,-0.0138872385042673,
-0.0116088612229254));
#14436=CARTESIAN_POINT('Ctrl Pts',(0.0029123013203729,-0.0139165723499641,
-0.0110417229255565));
#14437=CARTESIAN_POINT('Ctrl Pts',(0.00261419264222686,-0.0139459126747149,
-0.0105595615185512));
#14438=CARTESIAN_POINT('Ctrl Pts',(0.00248926933561196,-0.01395820782294,
-0.0103575103818322));
#14439=CARTESIAN_POINT('Ctrl Pts',(0.00234092856375039,-0.0139705041089217,
-0.0101702098174937));
#14440=CARTESIAN_POINT('Ctrl Pts',(0.0021733792536772,-0.0139828018207156,
-0.0100026471597294));
#14441=CARTESIAN_POINT('Ctrl Pts',(0.00178091745653428,-0.0140116075619584,
-0.00961015409740957));
#14442=CARTESIAN_POINT('Ctrl Pts',(0.00127750678143459,-0.0140404211261745,
-0.00932548282021525));
#14443=CARTESIAN_POINT('Ctrl Pts',(0.000736760751761841,-0.0140692314072482,
-0.00919196558011481));
#14444=CARTESIAN_POINT('Ctrl Pts',(0.00049575116194729,-0.0140820721007401,
-0.00913245717227823));
#14445=CARTESIAN_POINT('Ctrl Pts',(0.000247713071908436,-0.0140949121420458,
-0.00910237122778308));
#14446=CARTESIAN_POINT('Ctrl Pts',(2.22705864387592E-7,-0.0141077505478671,
-0.00910235329462672));
#14447=CARTESIAN_POINT('Ctrl Pts',(-0.000557104288925352,-0.0141366615323579,
-0.00910231291070271));
#14448=CARTESIAN_POINT('Ctrl Pts',(-0.00111629365783261,-0.0141655642231179,
-0.0092581981881314));
#14449=CARTESIAN_POINT('Ctrl Pts',(-0.00159417362234604,-0.0141944997930902,
-0.00954811419908839));
#14450=CARTESIAN_POINT('Ctrl Pts',(-0.0018046348026978,-0.0142072431903087,
-0.00967579493567463));
#14451=CARTESIAN_POINT('Ctrl Pts',(-0.00199948134856071,-0.0142199929646937,
-0.00982878575482296));
#14452=CARTESIAN_POINT('Ctrl Pts',(-0.00217306428972824,-0.014232752633238,
-0.010002332216334));
#14453=CARTESIAN_POINT('Ctrl Pts',(-0.00256717902049182,-0.0142617230683459,
-0.0103963641211593));
#14454=CARTESIAN_POINT('Ctrl Pts',(-0.00285235991347764,-0.0142907445081475,
-0.0109019563653772));
#14455=CARTESIAN_POINT('Ctrl Pts',(-0.00298529505148537,-0.0143196635229212,
-0.0114448158692004));
#14456=CARTESIAN_POINT('Ctrl Pts',(-0.00304385423221388,-0.0143324026213869,
-0.0116839505951352));
#14457=CARTESIAN_POINT('Ctrl Pts',(-0.00307346616249905,-0.0143451218444243,
-0.0119299420581625));
#14458=CARTESIAN_POINT('Ctrl Pts',(-0.0030734999708532,-0.0143578080768281,
-0.0121754300072245));
#14459=CARTESIAN_POINT('Ctrl Pts',(-0.00307357671814756,-0.01438660669886,
-0.0127327045733367));
#14460=CARTESIAN_POINT('Ctrl Pts',(-0.00291775615137512,-0.0144152353131311,
-0.0132918738548947));
#14461=CARTESIAN_POINT('Ctrl Pts',(-0.00262789661615805,-0.0144438906823375,
-0.0137697672192361));
#14462=CARTESIAN_POINT('Ctrl Pts',(-0.00250020522803293,-0.0144565141893353,
-0.0139802928692646));
#14463=CARTESIAN_POINT('Ctrl Pts',(-0.00234718809325915,-0.0144691428885395,
-0.0141752011655309));
#14464=CARTESIAN_POINT('Ctrl Pts',(-0.0021736016670944,-0.0144817936014535,
-0.0143488369594844));
#14465=CARTESIAN_POINT('Ctrl Pts',(-0.00177965194790562,-0.0145105040537058,
-0.0147428987175403));
#14466=CARTESIAN_POINT('Ctrl Pts',(-0.00127416024100349,-0.0145393278877474,
-0.0150280814152012));
#14467=CARTESIAN_POINT('Ctrl Pts',(-0.000731386520761171,-0.0145682115985004,
-0.0151610628281563));
#14468=CARTESIAN_POINT('Ctrl Pts',(-0.000492097458306903,-0.0145809453691465,
-0.0152196894647142));
#14469=CARTESIAN_POINT('Ctrl Pts',(-0.000245938049725031,-0.0145936907774618,
-0.0152493305261509));
#14470=CARTESIAN_POINT('Ctrl Pts',(-2.84602609272593E-7,-0.0146064432387867,
-0.0152493532733812));
#14471=CARTESIAN_POINT('Ctrl Pts',(0.000555018639657029,-0.0146352703657973,
-0.0152494046938309));
#14472=CARTESIAN_POINT('Ctrl Pts',(0.00111234868679064,-0.0146641335331714,
-0.0150946252343135));
#14473=CARTESIAN_POINT('Ctrl Pts',(0.00158904880133423,-0.0146930471839194,
-0.0148066946266959));
#14474=CARTESIAN_POINT('Ctrl Pts',(0.00180156679688988,-0.0147059371978164,
-0.0146783320907469));
#14475=CARTESIAN_POINT('Ctrl Pts',(0.00199821641796431,-0.0147188372451401,
-0.0145242071941443));
#14476=CARTESIAN_POINT('Ctrl Pts',(0.00217319919795374,-0.0147317486055931,
-0.0143492394685362));
#14477=CARTESIAN_POINT('Ctrl Pts',(0.0025730612372781,-0.0147612530112353,
-0.0139494118307433));
#14478=CARTESIAN_POINT('Ctrl Pts',(0.00286050813803622,-0.014790816493068,
-0.0134352012199921));
#14479=CARTESIAN_POINT('Ctrl Pts',(0.00299106370368742,-0.0148204339609196,
-0.0128829177606223));
#14480=CARTESIAN_POINT('Ctrl Pts',(0.00304579235279836,-0.0148328495480876,
-0.0126514015666794));
#14481=CARTESIAN_POINT('Ctrl Pts',(0.00307350023801115,-0.0148452746220606,
-0.0124135355879753));
#14482=CARTESIAN_POINT('Ctrl Pts',(0.00307349999999846,-0.014857708807874,
-0.0121758502088256));
#14483=CARTESIAN_POINT('',(0.00307349955219906,-0.0158577062176384,-0.012174689201038));
#14484=CARTESIAN_POINT('Ctrl Pts',(0.00307349978681731,-0.0148577676402129,
-0.0121747085446921));
#14485=CARTESIAN_POINT('Ctrl Pts',(0.00307328860483376,-0.0148871267056932,
-0.0116077092929736));
#14486=CARTESIAN_POINT('Ctrl Pts',(0.00291187603779568,-0.0149164857711735,
-0.0110406314886779));
#14487=CARTESIAN_POINT('Ctrl Pts',(0.00261358670794305,-0.0149458448366537,
-0.010558581890019));
#14488=CARTESIAN_POINT('Ctrl Pts',(0.00248859297119646,-0.0149581473192923,
-0.0103565861275044));
#14489=CARTESIAN_POINT('Ctrl Pts',(0.00234018929001624,-0.0149704498019308,
-0.0101693484610414));
#14490=CARTESIAN_POINT('Ctrl Pts',(0.00217258590305342,-0.0149827522845693,
-0.0100018540354419));
#14491=CARTESIAN_POINT('Ctrl Pts',(0.00177998102983827,-0.0150115704052771,
-0.00960950440028021));
#14492=CARTESIAN_POINT('Ctrl Pts',(0.00127646674261242,-0.0150403885259848,
-0.00932501696702219));
#14493=CARTESIAN_POINT('Ctrl Pts',(0.0007356723147371,-0.0150692066466926,
-0.00919169704143128));
#14494=CARTESIAN_POINT('Ctrl Pts',(0.000494655419529813,-0.0150820500741036,
-0.00913228009318085));
#14495=CARTESIAN_POINT('Ctrl Pts',(0.000246621602187934,-0.0150948935015146,
-0.00910228463910051));
#14496=CARTESIAN_POINT('Ctrl Pts',(-8.54034130405478E-7,-0.0151077369289256,
-0.00910235340521342));
#14497=CARTESIAN_POINT('Ctrl Pts',(-0.000558194471297123,-0.015136661640685,
-0.00910250827353096));
#14498=CARTESIAN_POINT('Ctrl Pts',(-0.00111734149881382,-0.0151655863524443,
-0.00925859673664403));
#14499=CARTESIAN_POINT('Ctrl Pts',(-0.00159512763372221,-0.0151945110642037,
-0.00954869320728318));
#14500=CARTESIAN_POINT('Ctrl Pts',(-0.00180551810764494,-0.0152072479005631,
-0.00967643557877912));
#14501=CARTESIAN_POINT('Ctrl Pts',(-0.0020002885992337,-0.0152199847369226,
-0.00982947658612617));
#14502=CARTESIAN_POINT('Ctrl Pts',(-0.00217379374682141,-0.015232721573282,
-0.0100030617649711));
#14503=CARTESIAN_POINT('Ctrl Pts',(-0.00256774114811238,-0.0152616408512068,
-0.01039719087906));
#14504=CARTESIAN_POINT('Ctrl Pts',(-0.00285273819986065,-0.0152905601291315,
-0.0109028266790015));
#14505=CARTESIAN_POINT('Ctrl Pts',(-0.00298550494832231,-0.0153194794070563,
-0.0114456735459853));
#14506=CARTESIAN_POINT('Ctrl Pts',(-0.00304400398090827,-0.0153322216772503,
-0.0116848600661706));
#14507=CARTESIAN_POINT('Ctrl Pts',(-0.00307354494863363,-0.0153449639474444,
-0.0119308959084206));
#14508=CARTESIAN_POINT('Ctrl Pts',(-0.00307349994837537,-0.0153577062176384,
-0.0121764166129453));
#14509=CARTESIAN_POINT('Ctrl Pts',(-0.00307339781783225,-0.0153866254955631,
-0.0127336392571295));
#14510=CARTESIAN_POINT('Ctrl Pts',(-0.00291742600410256,-0.0154155447734879,
-0.0132927020720123));
#14511=CARTESIAN_POINT('Ctrl Pts',(-0.00262747630529442,-0.0154444640514126,
-0.0137704599826172));
#14512=CARTESIAN_POINT('Ctrl Pts',(-0.00249972009317517,-0.0154572063216067,
-0.0139809673265453));
#14513=CARTESIAN_POINT('Ctrl Pts',(-0.00234663993625058,-0.0154699485918007,
-0.0141758459158392));
#14514=CARTESIAN_POINT('Ctrl Pts',(-0.00217299712068187,-0.0154826908619947,
-0.0143494415096372));
#14515=CARTESIAN_POINT('Ctrl Pts',(-0.00177883122144032,-0.0155116155737541,
-0.0147435002163547));
#14516=CARTESIAN_POINT('Ctrl Pts',(-0.00127311414354502,-0.0155405402855134,
-0.0150285730660098));
#14517=CARTESIAN_POINT('Ctrl Pts',(-0.000730164233966559,-0.0155694649972728,
-0.0151613620273653));
#14518=CARTESIAN_POINT('Ctrl Pts',(-0.000491079253372756,-0.0155822018336322,
-0.0152198349098332));
#14519=CARTESIAN_POINT('Ctrl Pts',(-0.000245149159454215,-0.0155949386699917,
-0.0152493750433145));
#14520=CARTESIAN_POINT('Ctrl Pts',(2.72618638915599E-7,-0.0156076755063511,
-0.0152493532744675));
#14521=CARTESIAN_POINT('Ctrl Pts',(0.000555559208324033,-0.0156364936270589,
-0.0152493040206933));
#14522=CARTESIAN_POINT('Ctrl Pts',(0.00111284669964006,-0.0156653117477667,
-0.0150944325339671));
#14523=CARTESIAN_POINT('Ctrl Pts',(0.00158948612246453,-0.0156941298684745,
-0.0148064304316904));
#14524=CARTESIAN_POINT('Ctrl Pts',(0.00180191093289366,-0.0157069732958855,
-0.0146780759795623));
#14525=CARTESIAN_POINT('Ctrl Pts',(0.00199847381907867,-0.0157198167232965,
-0.0145239793332489));
#14526=CARTESIAN_POINT('Ctrl Pts',(0.00217338267989119,-0.0157326601507075,
-0.0143490559868944));
#14527=CARTESIAN_POINT('Ctrl Pts',(0.00257321058667491,-0.0157620192161878,
-0.0139491949673004));
#14528=CARTESIAN_POINT('Ctrl Pts',(0.00286061375982055,-0.0157913782816681,
-0.0134349608491815));
#14529=CARTESIAN_POINT('Ctrl Pts',(0.0029911228767067,-0.0158207373471483,
-0.0128826673968034));
#14530=CARTESIAN_POINT('Ctrl Pts',(0.00304581079399547,-0.0158330398297868,
-0.0126512369851707));
#14531=CARTESIAN_POINT('Ctrl Pts',(0.00307349860159295,-0.0158453423124253,
-0.0124134640517282));
#14532=CARTESIAN_POINT('Ctrl Pts',(0.00307349999994677,-0.0158576447950638,
-0.0121758713756698));
#14533=CARTESIAN_POINT('',(0.00307349958720421,-0.0168578266932082,-0.0121769697098861));
#14534=CARTESIAN_POINT('Ctrl Pts',(0.00307349910445136,-0.0158577676402129,
-0.0121735070264063));
#14535=CARTESIAN_POINT('Ctrl Pts',(0.0030730662635019,-0.015887135733148,
-0.0116065041433245));
#14536=CARTESIAN_POINT('Ctrl Pts',(0.00291142998921608,-0.0159165038260831,
-0.0110394863287188));
#14537=CARTESIAN_POINT('Ctrl Pts',(0.00261294882229721,-0.0159458719190182,
-0.0105575514908304));
#14538=CARTESIAN_POINT('Ctrl Pts',(0.00248795287356632,-0.0159581704927498,
-0.010355730039547));
#14539=CARTESIAN_POINT('Ctrl Pts',(0.00233958187208303,-0.0159704690664813,
-0.0101686574839441));
#14540=CARTESIAN_POINT('Ctrl Pts',(0.00217203976625694,-0.0159827676402129,
-0.0100013083907699));
#14541=CARTESIAN_POINT('Ctrl Pts',(0.00177933049551567,-0.0160115948051663,
-0.0096090515308265));
#14542=CARTESIAN_POINT('Ctrl Pts',(0.00127573698229395,-0.0160404219701197,
-0.00932468905152511));
#14543=CARTESIAN_POINT('Ctrl Pts',(0.000734901807145515,-0.016069249135073,
-0.00919150719673301));
#14544=CARTESIAN_POINT('Ctrl Pts',(0.000494016025655897,-0.0160820886367863,
-0.00913218854172314));
#14545=CARTESIAN_POINT('Ctrl Pts',(0.000246129473808355,-0.0160949281384996,
-0.00910225723428693));
#14546=CARTESIAN_POINT('Ctrl Pts',(-1.1965279448354E-6,-0.0161077676402129,
-0.00910235351946507));
#14547=CARTESIAN_POINT('Ctrl Pts',(-0.000558544714015742,-0.0161367014075452,
-0.00910257049774071));
#14548=CARTESIAN_POINT('Ctrl Pts',(-0.00111768053985367,-0.0161656351748775,
-0.00925872543230002));
#14549=CARTESIAN_POINT('Ctrl Pts',(-0.00159543770967884,-0.0161945689422098,
-0.00954888150054006));
#14550=CARTESIAN_POINT('Ctrl Pts',(-0.00180568457728475,-0.0162073018415442,
-0.00967657064539715));
#14551=CARTESIAN_POINT('Ctrl Pts',(-0.00200032768393728,-0.0162200347408785,
-0.00982952551388758));
#14552=CARTESIAN_POINT('Ctrl Pts',(-0.00217373222877299,-0.0162327676402129,
-0.0100030002202893));
#14553=CARTESIAN_POINT('Ctrl Pts',(-0.00256769613031811,-0.0162616959633114,
-0.010397123524371));
#14554=CARTESIAN_POINT('Ctrl Pts',(-0.0028527088982565,-0.0162906242864098,
-0.010902758378207));
#14555=CARTESIAN_POINT('Ctrl Pts',(-0.00298548896101624,-0.0163195526095083,
-0.0114456081813707));
#14556=CARTESIAN_POINT('Ctrl Pts',(-0.00304395754395783,-0.0163322909530765,
-0.01168464752268));
#14557=CARTESIAN_POINT('Ctrl Pts',(-0.00307350373554943,-0.0163450292966447,
-0.0119305284371561));
#14558=CARTESIAN_POINT('Ctrl Pts',(-0.00307349999964376,-0.0163577676402129,
-0.0121759000821285));
#14559=CARTESIAN_POINT('Ctrl Pts',(-0.00307349151553545,-0.0163866959633114,
-0.0127331303206558));
#14560=CARTESIAN_POINT('Ctrl Pts',(-0.00291760959876268,-0.0164156242864098,
-0.0132922253787799));
#14561=CARTESIAN_POINT('Ctrl Pts',(-0.00262773400439643,-0.0164445526095082,
-0.0137700352875036));
#14562=CARTESIAN_POINT('Ctrl Pts',(-0.00250008972648538,-0.0164572909530765,
-0.0139804348587788));
#14563=CARTESIAN_POINT('Ctrl Pts',(-0.00234715003467735,-0.0164700292966447,
-0.0141752289474491));
#14564=CARTESIAN_POINT('Ctrl Pts',(-0.00217366606222184,-0.0164827676402129,
-0.0143487725441342));
#14565=CARTESIAN_POINT('Ctrl Pts',(-0.00177961601418933,-0.0165117014075452,
-0.0147429580221444));
#14566=CARTESIAN_POINT('Ctrl Pts',(-0.00127397940839639,-0.0165406351748775,
-0.0150281879702471));
#14567=CARTESIAN_POINT('Ctrl Pts',(-0.000731063511943571,-0.0165695689422098,
-0.0151611419478947));
#14568=CARTESIAN_POINT('Ctrl Pts',(-0.00049214220670302,-0.0165823018415442,
-0.0152196510799426));
#14569=CARTESIAN_POINT('Ctrl Pts',(-0.000246375470689803,-0.0165950347408785,
-0.0152492650717026));
#14570=CARTESIAN_POINT('Ctrl Pts',(-1.10293681041439E-6,-0.0166077676402129,
-0.0152493530886616));
#14571=CARTESIAN_POINT('Ctrl Pts',(0.000554191784918156,-0.0166365948051663,
-0.0152495523582333));
#14572=CARTESIAN_POINT('Ctrl Pts',(0.00111155506214211,-0.0166654219701197,
-0.0150949259473566));
#14573=CARTESIAN_POINT('Ctrl Pts',(0.00158832691156067,-0.016694249135073,
-0.0148071305186285));
#14574=CARTESIAN_POINT('Ctrl Pts',(0.00180067914901998,-0.0167070886367863,
-0.0146789476083005));
#14575=CARTESIAN_POINT('Ctrl Pts',(0.00199720019475119,-0.0167199281384996,
-0.0145250469724957));
#14576=CARTESIAN_POINT('Ctrl Pts',(0.00217210598231125,-0.0167327676402129,
-0.0143503320405605));
#14577=CARTESIAN_POINT('Ctrl Pts',(0.00257217208601626,-0.016762135733148,
-0.0139507024853955));
#14578=CARTESIAN_POINT('Ctrl Pts',(0.00285987790424067,-0.0167915038260831,
-0.0134366328536536));
#14579=CARTESIAN_POINT('Ctrl Pts',(0.00299070999424267,-0.0168208719190182,
-0.012884412373958));
#14580=CARTESIAN_POINT('Ctrl Pts',(0.0030454989827174,-0.0168331704927497,
-0.0126531571712238));
#14581=CARTESIAN_POINT('Ctrl Pts',(0.00307332514268951,-0.0168454690664813,
-0.0124155516398577));
#14582=CARTESIAN_POINT('Ctrl Pts',(0.00307349917447235,-0.0168577676402129,
-0.012178105955595));
#14583=CARTESIAN_POINT('',(0.00307349973395781,-0.017857767640213,-0.0121771320990067));
#14584=CARTESIAN_POINT('Ctrl Pts',(0.00307349999993608,-0.0168578857462035,
-0.0121758334641773));
#14585=CARTESIAN_POINT('Ctrl Pts',(0.00307349634310224,-0.0168872451650051,
-0.011608834024638));
#14586=CARTESIAN_POINT('Ctrl Pts',(0.00291229126051317,-0.0169166045838068,
-0.0110416970556195));
#14587=CARTESIAN_POINT('Ctrl Pts',(0.00261417824885523,-0.0169459640026085,
-0.0105595382389228));
#14588=CARTESIAN_POINT('Ctrl Pts',(0.00248926148152478,-0.0169582663293905,
-0.010357501701213));
#14589=CARTESIAN_POINT('Ctrl Pts',(0.00234093052159938,-0.0169705686561726,
-0.0101702139657608));
#14590=CARTESIAN_POINT('Ctrl Pts',(0.00217339345729084,-0.0169828709829547,
-0.0100026613645675));
#14591=CARTESIAN_POINT('Ctrl Pts',(0.00178093414907792,-0.0170116894577097,
-0.0096101656608555));
#14592=CARTESIAN_POINT('Ctrl Pts',(0.00127752528436554,-0.0170405079324647,
-0.0093254911163739));
#14593=CARTESIAN_POINT('Ctrl Pts',(0.000736780138390888,-0.0170693264072197,
-0.00919197036699293));
#14594=CARTESIAN_POINT('Ctrl Pts',(0.000495791105552733,-0.0170821696780484,
-0.00913246537375042));
#14595=CARTESIAN_POINT('Ctrl Pts',(0.000247774567391759,-0.0170950129488772,
-0.00910237784625514));
#14596=CARTESIAN_POINT('Ctrl Pts',(3.04836335295681E-7,-0.0171078562197059,
-0.00910235330167525));
#14597=CARTESIAN_POINT('Ctrl Pts',(-0.000557035926712533,-0.017136781285948,
-0.00910229802342031));
#14598=CARTESIAN_POINT('Ctrl Pts',(-0.00111624201296547,-0.0171657063521901,
-0.00925817581220162));
#14599=CARTESIAN_POINT('Ctrl Pts',(-0.00159413762858014,-0.0171946314184321,
-0.00954809236304452));
#14600=CARTESIAN_POINT('Ctrl Pts',(-0.00180457113853043,-0.0172073680977738,
-0.0096757523695254));
#14601=CARTESIAN_POINT('Ctrl Pts',(-0.00199939495831796,-0.0172201047771154,
-0.00982871566688341));
#14602=CARTESIAN_POINT('Ctrl Pts',(-0.00217296233084268,-0.0172328414564571,
-0.0100022302836575));
#14603=CARTESIAN_POINT('Ctrl Pts',(-0.00256706069867207,-0.0172617610884542,
-0.0103962088654065));
#14604=CARTESIAN_POINT('Ctrl Pts',(-0.00285225122890694,-0.0172906807204512,
-0.0109017358769659));
#14605=CARTESIAN_POINT('Ctrl Pts',(-0.00298522556645655,-0.0173196003524483,
-0.0114445321755718));
#14606=CARTESIAN_POINT('Ctrl Pts',(-0.00304381462849378,-0.0173323424660349,
-0.0116836905470188));
#14607=CARTESIAN_POINT('Ctrl Pts',(-0.00307344965072599,-0.0173450845796216,
-0.0119297089794094));
#14608=CARTESIAN_POINT('Ctrl Pts',(-0.00307349993553538,-0.0173578266932083,
-0.0121752237915101));
#14609=CARTESIAN_POINT('Ctrl Pts',(-0.00307361406245576,-0.0173867463252053,
-0.0127324467331738));
#14610=CARTESIAN_POINT('Ctrl Pts',(-0.00291785907157083,-0.0174156659572024,
-0.0132915702771264));
#14611=CARTESIAN_POINT('Ctrl Pts',(-0.00262809456714721,-0.0174445855891994,
-0.0137694408103958));
#14612=CARTESIAN_POINT('Ctrl Pts',(-0.00250042308677956,-0.0174573277027861,
-0.0139799926118594));
#14613=CARTESIAN_POINT('Ctrl Pts',(-0.00234742282997037,-0.0174700698163728,
-0.0141749262395666));
#14614=CARTESIAN_POINT('Ctrl Pts',(-0.00217385252425702,-0.0174828119299594,
-0.0143485860020069));
#14615=CARTESIAN_POINT('Ctrl Pts',(-0.00177984154984009,-0.0175117369962015,
-0.0147428000464823));
#14616=CARTESIAN_POINT('Ctrl Pts',(-0.00127423643353935,-0.0175406620624436,
-0.0150280719926622));
#14617=CARTESIAN_POINT('Ctrl Pts',(-0.000731338562493786,-0.0175695871286856,
-0.015161074577687));
#14618=CARTESIAN_POINT('Ctrl Pts',(-0.000492282373619284,-0.0175823238080273,
-0.0152196400884069));
#14619=CARTESIAN_POINT('Ctrl Pts',(-0.000246370023034821,-0.0175950604873689,
-0.0152492769502351));
#14620=CARTESIAN_POINT('Ctrl Pts',(-9.54153753620061E-7,-0.0176077971667106,
-0.0152493531384518));
#14621=CARTESIAN_POINT('Ctrl Pts',(0.000554332734110935,-0.0176366156414656,
-0.015249525524687));
#14622=CARTESIAN_POINT('Ctrl Pts',(0.00111168225525367,-0.0176654341162206,
-0.0150948763166834));
#14623=CARTESIAN_POINT('Ctrl Pts',(0.00158843673613355,-0.0176942525909756,
-0.0148070642217173));
#14624=CARTESIAN_POINT('Ctrl Pts',(0.00180090762395152,-0.0177070958618043,
-0.0146787975901602));
#14625=CARTESIAN_POINT('Ctrl Pts',(0.00199752762317113,-0.0177199391326331,
-0.0145247836831463));
#14626=CARTESIAN_POINT('Ctrl Pts',(0.00217250307581148,-0.0177327824034618,
-0.0143499353079155));
#14627=CARTESIAN_POINT('Ctrl Pts',(0.0025724928963627,-0.0177621418222635,
-0.0139502359833711));
#14628=CARTESIAN_POINT('Ctrl Pts',(0.00286010416722769,-0.0177915012410651,
-0.0134361180366009));
#14629=CARTESIAN_POINT('Ctrl Pts',(0.00299083671501046,-0.0178208606598668,
-0.012883877293316));
#14630=CARTESIAN_POINT('Ctrl Pts',(0.00304561690445299,-0.0178331629866489,
-0.0126524746851047));
#14631=CARTESIAN_POINT('Ctrl Pts',(0.00307340087954239,-0.0178454653134309,
-0.0124147189475048));
#14632=CARTESIAN_POINT('Ctrl Pts',(0.00307349973395781,-0.017857767640213,
-0.0121771320990067));
#14633=CARTESIAN_POINT('',(0.00307349903227376,-0.0188577420250978,-0.0121736488040434));
#14634=CARTESIAN_POINT('Ctrl Pts',(0.00307349999999813,-0.0178578333594276,
-0.0121758566778537));
#14635=CARTESIAN_POINT('Ctrl Pts',(0.0030735006215337,-0.0178869007967827,
-0.0116125647073703));
#14636=CARTESIAN_POINT('Ctrl Pts',(0.00291433696992175,-0.0179159846530298,
-0.0110488283918617));
#14637=CARTESIAN_POINT('Ctrl Pts',(0.00261987653841084,-0.0179450851484625,
-0.0105687910060336));
#14638=CARTESIAN_POINT('Ctrl Pts',(0.00249371415197432,-0.0179575533362304,
-0.0103631176601649));
#14639=CARTESIAN_POINT('Ctrl Pts',(0.00234336486540254,-0.017970024578483,
-0.0101726346057528));
#14640=CARTESIAN_POINT('Ctrl Pts',(0.00217330443424238,-0.0179824988925469,
-0.0100025723369102));
#14641=CARTESIAN_POINT('Ctrl Pts',(0.00177902997917332,-0.018011419808167,
-0.00960829362128951));
#14642=CARTESIAN_POINT('Ctrl Pts',(0.00127275718761501,-0.0180403572352389,
-0.009322737625378));
#14643=CARTESIAN_POINT('Ctrl Pts',(0.000728564199173013,-0.0180693105259971,
-0.00918995368046224));
#14644=CARTESIAN_POINT('Ctrl Pts',(0.000490185945838011,-0.018081993223176,
-0.00913178901180201));
#14645=CARTESIAN_POINT('Ctrl Pts',(0.000244911249906314,-0.0180946789642627,
-0.00910235416870036));
#14646=CARTESIAN_POINT('Ctrl Pts',(1.10706451622527E-8,-0.0181073676948121,
-0.00910235328657803));
#14647=CARTESIAN_POINT('Ctrl Pts',(-0.000401979955621974,-0.0181281955922476,
-0.00910235183861967));
#14648=CARTESIAN_POINT('Ctrl Pts',(-0.000804358317651879,-0.0181490315443514,
-0.00918229815991824));
#14649=CARTESIAN_POINT('Ctrl Pts',(-0.00117616985844715,-0.0181698779590349,
-0.00933630636599481));
#14650=CARTESIAN_POINT('Ctrl Pts',(-0.00154798139924243,-0.0181907243737183,
-0.00949031457207138));
#14651=CARTESIAN_POINT('Ctrl Pts',(-0.00188889766670545,-0.0182115812509814,
-0.00971816659367328));
#14652=CARTESIAN_POINT('Ctrl Pts',(-0.00217328877794405,-0.018232438798651,
-0.0100025566805555));
#14653=CARTESIAN_POINT('Ctrl Pts',(-0.00231548433356335,-0.0182428675724858,
-0.0101447517239966));
#14654=CARTESIAN_POINT('Ctrl Pts',(-0.00244369725231803,-0.0182532965139223,
-0.0103009513223182));
#14655=CARTESIAN_POINT('Ctrl Pts',(-0.00255551954698984,-0.0182637381842315,
-0.0104683047235729));
#14656=CARTESIAN_POINT('Ctrl Pts',(-0.00266734184166164,-0.0182741798545408,
-0.0106356581248275));
#14657=CARTESIAN_POINT('Ctrl Pts',(-0.00276272283879781,-0.018284634253723,
-0.0108142141603233));
#14658=CARTESIAN_POINT('Ctrl Pts',(-0.00283954268404827,-0.0182950502136605,
-0.0109996732002329));
#14659=CARTESIAN_POINT('Ctrl Pts',(-0.00291636252929872,-0.0183054661735979,
-0.0111851322401425));
#14660=CARTESIAN_POINT('Ctrl Pts',(-0.00297487762643972,-0.0183158436942908,
-0.0113773322729812));
#14661=CARTESIAN_POINT('Ctrl Pts',(-0.00301444328935122,-0.0183263748869377,
-0.0115762418246218));
#14662=CARTESIAN_POINT('Ctrl Pts',(-0.00303422612080698,-0.0183316404832612,
-0.0116756966004421));
#14663=CARTESIAN_POINT('Ctrl Pts',(-0.00304907659667239,-0.0183369444975732,
-0.0117768871638611));
#14664=CARTESIAN_POINT('Ctrl Pts',(-0.00305870018960846,-0.0183420419650195,
-0.0118745969171828));
#14665=CARTESIAN_POINT('Ctrl Pts',(-0.0030635119860765,-0.0183445906987426,
-0.0119234517938437));
#14666=CARTESIAN_POINT('Ctrl Pts',(-0.00306716319515293,-0.0183470877957494,
-0.0119714145937676));
#14667=CARTESIAN_POINT('Ctrl Pts',(-0.00306979781767152,-0.0183498766894212,
-0.0120250434439775));
#14668=CARTESIAN_POINT('Ctrl Pts',(-0.0030724324401901,-0.018352665583093,
-0.0120786722941874));
#14669=CARTESIAN_POINT('Ctrl Pts',(-0.0030735,-0.0183557462734298,-0.0121380003223703));
#14670=CARTESIAN_POINT('Ctrl Pts',(-0.0030735,-0.0183577122040634,-0.0121758532865577));
#14671=CARTESIAN_POINT('Ctrl Pts',(-0.00307350000000001,-0.0183596781346969,
-0.0122137062507451));
#14672=CARTESIAN_POINT('Ctrl Pts',(-0.00307310376848221,-0.0183605293056272,
-0.0122300919653714));
#14673=CARTESIAN_POINT('Ctrl Pts',(-0.0030725419671156,-0.0183616976447121,
-0.0122525873097381));
#14674=CARTESIAN_POINT('Ctrl Pts',(-0.003071980165749,-0.0183628659837971,
-0.0122750826541048));
#14675=CARTESIAN_POINT('Ctrl Pts',(-0.00307096835910987,-0.0183643514910369,
-0.0123036761037775));
#14676=CARTESIAN_POINT('Ctrl Pts',(-0.00306955009680357,-0.0183658045381892,
-0.0123316238011403));
#14677=CARTESIAN_POINT('Ctrl Pts',(-0.00306671357219098,-0.0183687106324938,
-0.0123875191958658));
#14678=CARTESIAN_POINT('Ctrl Pts',(-0.00306256243770937,-0.0183714868864489,
-0.0124408581493612));
#14679=CARTESIAN_POINT('Ctrl Pts',(-0.00305674327724998,-0.0183743826836283,
-0.0124963572443917));
#14680=CARTESIAN_POINT('Ctrl Pts',(-0.00304510495633122,-0.0183801742779871,
-0.0126073554344527));
#14681=CARTESIAN_POINT('Ctrl Pts',(-0.00302633139541316,-0.018386444045243,
-0.0127269199041359));
#14682=CARTESIAN_POINT('Ctrl Pts',(-0.00299862041661768,-0.0183929964084466,
-0.0128501513267774));
#14683=CARTESIAN_POINT('Ctrl Pts',(-0.0029709094378222,-0.0183995487716502,
-0.0129733827494189));
#14684=CARTESIAN_POINT('Ctrl Pts',(-0.0029344247030508,-0.0184063837308014,
-0.0131003379592189));
#14685=CARTESIAN_POINT('Ctrl Pts',(-0.00288699201251265,-0.0184135533785181,
-0.0132302153542029));
#14686=CARTESIAN_POINT('Ctrl Pts',(-0.0028395593219745,-0.0184207230262348,
-0.0133600927491869));
#14687=CARTESIAN_POINT('Ctrl Pts',(-0.00278113531337715,-0.018428227362517,
-0.0134928631967346));
#14688=CARTESIAN_POINT('Ctrl Pts',(-0.00270984678779956,-0.018436053593843,
-0.0136260714207201));
#14689=CARTESIAN_POINT('Ctrl Pts',(-0.00256726973664439,-0.0184517060564951,
-0.0138924878686913));
#14690=CARTESIAN_POINT('Ctrl Pts',(-0.00237306306717248,-0.0184686460993229,
-0.0141605357837572));
#14691=CARTESIAN_POINT('Ctrl Pts',(-0.00211788429611001,-0.0184868837602526,
-0.0144031764239341));
#14692=CARTESIAN_POINT('Ctrl Pts',(-0.00186270552504755,-0.0185051214211823,
-0.0146458170641111));
#14693=CARTESIAN_POINT('Ctrl Pts',(-0.00154608949796055,-0.018524656700214,
-0.0148624700046778));
#14694=CARTESIAN_POINT('Ctrl Pts',(-0.00117424541782602,-0.0185454869076755,
-0.0150161965666414));
#14695=CARTESIAN_POINT('Ctrl Pts',(-0.000802401337691485,-0.018566317115137,
-0.0151699231286051));
#14696=CARTESIAN_POINT('Ctrl Pts',(-0.000374985873875508,-0.0185884422510285,
-0.0152597732637985));
#14697=CARTESIAN_POINT('Ctrl Pts',(7.73909019784573E-5,-0.0186118630361116,
-0.0152483787784444));
#14698=CARTESIAN_POINT('Ctrl Pts',(0.00052976767783242,-0.0186352838211947,
-0.0152369842930902));
#14699=CARTESIAN_POINT('Ctrl Pts',(0.00100698173546338,-0.0186600002554696,
-0.0151229073790469));
#14700=CARTESIAN_POINT('Ctrl Pts',(0.00145022863864532,-0.018686012145561,
-0.0148856944526881));
#14701=CARTESIAN_POINT('Ctrl Pts',(0.00189347554182726,-0.0187120240356524,
-0.0146484815263293));
#14702=CARTESIAN_POINT('Ctrl Pts',(0.00230162808382228,-0.0187393313815604,
-0.014286383187642));
#14703=CARTESIAN_POINT('Ctrl Pts',(0.00259715510412251,-0.0187679342360236,
-0.0138193822991193));
#14704=CARTESIAN_POINT('Ctrl Pts',(0.00287285221500992,-0.0187946178344663,
-0.0133837172434613));
#14705=CARTESIAN_POINT('Ctrl Pts',(0.00304908377064998,-0.0188224289167476,
-0.012855992906357));
#14706=CARTESIAN_POINT('Ctrl Pts',(0.00307111645156604,-0.0188513674685947,
-0.0122968739084389));
#14707=CARTESIAN_POINT('Ctrl Pts',(0.00307270096662869,-0.0188534486302775,
-0.0122566639822211));
#14708=CARTESIAN_POINT('Ctrl Pts',(0.0030735000947714,-0.0188555356232268,
-0.0122163109465063));
#14709=CARTESIAN_POINT('Ctrl Pts',(0.00307349999999157,-0.0188576284474371,
-0.012175846087576));
#14710=CARTESIAN_POINT('',(0.00307349999999759,-0.0198577587605502,-0.0121758571382905));
#14711=CARTESIAN_POINT('Ctrl Pts',(0.00307349881402483,-0.0188577676402129,
-0.0121731532517477));
#14712=CARTESIAN_POINT('Ctrl Pts',(0.00307300071011293,-0.018887132482759,
-0.0116061524943504));
#14713=CARTESIAN_POINT('Ctrl Pts',(0.00291130029165572,-0.0189164973253051,
-0.0110391550281488));
#14714=CARTESIAN_POINT('Ctrl Pts',(0.00261276553606138,-0.0189458621678513,
-0.0105572555899176));
#14715=CARTESIAN_POINT('Ctrl Pts',(0.00248770402422934,-0.0189581636219859,
-0.01035537935552));
#14716=CARTESIAN_POINT('Ctrl Pts',(0.00233925310066207,-0.0189704650761205,
-0.010168264828373));
#14717=CARTESIAN_POINT('Ctrl Pts',(0.0021716218292663,-0.0189827665302551,
-0.0100008910154706));
#14718=CARTESIAN_POINT('Ctrl Pts',(0.0017788404149206,-0.0190115904037082,
-0.00960871285915861));
#14719=CARTESIAN_POINT('Ctrl Pts',(0.00127519655609348,-0.0190404142771613,
-0.00932444800617673));
#14720=CARTESIAN_POINT('Ctrl Pts',(0.000734339809416652,-0.0190692381506144,
-0.0091913688596753));
#14721=CARTESIAN_POINT('Ctrl Pts',(0.00049336209149727,-0.019082080573842,
-0.00913207569337273));
#14722=CARTESIAN_POINT('Ctrl Pts',(0.000245384423439502,-0.0190949229970696,
-0.00910219102134657));
#14723=CARTESIAN_POINT('Ctrl Pts',(-2.02406328883577E-6,-0.0191077654202972,
-0.00910235395303485));
#14724=CARTESIAN_POINT('Ctrl Pts',(-0.00055936788590402,-0.0191366958961591,
-0.00910272099367752));
#14725=CARTESIAN_POINT('Ctrl Pts',(-0.00111845823087898,-0.019165626372021,
-0.009259024171689));
#14726=CARTESIAN_POINT('Ctrl Pts',(-0.00159613540464352,-0.0191945568478828,
-0.00954930535818452));
#14727=CARTESIAN_POINT('Ctrl Pts',(-0.00180641922172863,-0.0192072926687017,
-0.00967709341103036));
#14728=CARTESIAN_POINT('Ctrl Pts',(-0.00200108197151192,-0.0192200284895205,
-0.00983016017137237));
#14729=CARTESIAN_POINT('Ctrl Pts',(-0.00217448460178119,-0.0192327643103394,
-0.0100037531584294));
#14730=CARTESIAN_POINT('Ctrl Pts',(-0.00256830904193374,-0.0192616893473823,
-0.0103980099285603));
#14731=CARTESIAN_POINT('Ctrl Pts',(-0.00285314591010015,-0.0192906143844251,
-0.0109037395292233));
#14732=CARTESIAN_POINT('Ctrl Pts',(-0.00298573909953144,-0.019319539421468,
-0.0114466315921954));
#14733=CARTESIAN_POINT('Ctrl Pts',(-0.00304414539475079,-0.0193322806811059,
-0.011685771432169));
#14734=CARTESIAN_POINT('Ctrl Pts',(-0.00307360736477033,-0.0193450219407437,
-0.0119317475467586));
#14735=CARTESIAN_POINT('Ctrl Pts',(-0.00307349970435152,-0.0193577632003816,
-0.0121772013782274));
#14736=CARTESIAN_POINT('Ctrl Pts',(-0.00307325529511013,-0.0193866882374244,
-0.0127344273801568));
#14737=CARTESIAN_POINT('Ctrl Pts',(-0.00291713891682898,-0.0194156132744673,
-0.0132934530596749));
#14738=CARTESIAN_POINT('Ctrl Pts',(-0.0026270644627302,-0.0194445383115101,
-0.013771138389184));
#14739=CARTESIAN_POINT('Ctrl Pts',(-0.00249928886373934,-0.019457279571148,
-0.0139815551571714));
#14740=CARTESIAN_POINT('Ctrl Pts',(-0.0023462072838056,-0.0194700208307859,
-0.0141763452408011));
#14741=CARTESIAN_POINT('Ctrl Pts',(-0.00217257832192293,-0.0194827620904237,
-0.0143498601138497));
#14742=CARTESIAN_POINT('Ctrl Pts',(-0.0017783340608814,-0.0195116925662856,
-0.0147438453232469));
#14743=CARTESIAN_POINT('Ctrl Pts',(-0.00127255879685045,-0.0195406230421475,
-0.0150288213855679));
#14744=CARTESIAN_POINT('Ctrl Pts',(-0.000729580226654389,-0.0195695535180093,
-0.0151615047971793));
#14745=CARTESIAN_POINT('Ctrl Pts',(-0.000490549323342851,-0.0195822893388282,
-0.0152199149029787));
#14746=CARTESIAN_POINT('Ctrl Pts',(-0.000244682725290316,-0.019595025159647,
-0.0152494068678258));
#14747=CARTESIAN_POINT('Ctrl Pts',(6.72119984720121E-7,-0.0196077609804659,
-0.0152493532130677));
#14748=CARTESIAN_POINT('Ctrl Pts',(0.000555962360944095,-0.019636584853919,
-0.0152492317809294));
#14749=CARTESIAN_POINT('Ctrl Pts',(0.00111323264387907,-0.0196654087273722,
-0.0150942859026573));
#14750=CARTESIAN_POINT('Ctrl Pts',(0.00158983623043085,-0.0196942326008253,
-0.0148062188524841));
#14751=CARTESIAN_POINT('Ctrl Pts',(0.00180218607231614,-0.0197070750240529,
-0.0146778711138546));
#14752=CARTESIAN_POINT('Ctrl Pts',(0.00199867926914927,-0.0197199174472805,
-0.014523797397214));
#14753=CARTESIAN_POINT('Ctrl Pts',(0.00217352894764179,-0.0197327598705081,
-0.0143489096971842));
#14754=CARTESIAN_POINT('Ctrl Pts',(0.00257333147611902,-0.0197621247130542,
-0.0139490202305618));
#14755=CARTESIAN_POINT('Ctrl Pts',(0.00286070034265989,-0.0197914895556003,
-0.0134347647981465));
#14756=CARTESIAN_POINT('Ctrl Pts',(0.00299117167179052,-0.0198208543981464,
-0.0128824608720523));
#14757=CARTESIAN_POINT('Ctrl Pts',(0.00304582842905604,-0.019833155852281,
-0.012651090947131));
#14758=CARTESIAN_POINT('Ctrl Pts',(0.00307349970232731,-0.0198454573064156,
-0.012413383918551));
#14759=CARTESIAN_POINT('Ctrl Pts',(0.00307349999999759,-0.0198577587605502,
-0.0121758571382905));
#14760=CARTESIAN_POINT('',(0.00307349938939493,-0.0208578413935592,-0.0121772072451699));
#14761=CARTESIAN_POINT('Ctrl Pts',(0.00307349999548701,-0.0198577676402129,
-0.0121756867291843));
#14762=CARTESIAN_POINT('Ctrl Pts',(0.00307346926887639,-0.0198871331262766,
-0.0116086854885077));
#14763=CARTESIAN_POINT('Ctrl Pts',(0.00291223613639999,-0.0199164986123403,
-0.0110415547028757));
#14764=CARTESIAN_POINT('Ctrl Pts',(0.00261409846967682,-0.019945864098404,
-0.010559409213652));
#14765=CARTESIAN_POINT('Ctrl Pts',(0.00248920881946095,-0.019958165279007,
-0.0103574388213693));
#14766=CARTESIAN_POINT('Ctrl Pts',(0.00234091965474288,-0.0199704664596099,
-0.010170209557073));
#14767=CARTESIAN_POINT('Ctrl Pts',(0.00217343535246285,-0.0199827676402129,
-0.0100027032644324));
#14768=CARTESIAN_POINT('Ctrl Pts',(0.00178098080283119,-0.0200115921582588,
-0.00961019718628788));
#14769=CARTESIAN_POINT('Ctrl Pts',(0.00127757369359316,-0.0200404166763048,
-0.00932551220153036));
#14770=CARTESIAN_POINT('Ctrl Pts',(0.000736827631172451,-0.0200692411943507,
-0.00919198209430787));
#14771=CARTESIAN_POINT('Ctrl Pts',(0.000495909767823558,-0.0200820833429714,
-0.00913249060586174));
#14772=CARTESIAN_POINT('Ctrl Pts',(0.00024796804554989,-0.0200949254915922,
-0.0091023992270146));
#14773=CARTESIAN_POINT('Ctrl Pts',(5.7007540347468E-7,-0.0201077676402129,
-0.00910235333942713));
#14774=CARTESIAN_POINT('Ctrl Pts',(-0.000556774407145435,-0.0201366987614893,
-0.00910224996269499));
#14775=CARTESIAN_POINT('Ctrl Pts',(-0.00111599691584013,-0.0201656298827657,
-0.00925808148757206));
#14776=CARTESIAN_POINT('Ctrl Pts',(-0.00159391916450755,-0.0201945610040421,
-0.00954795984370019));
#14777=CARTESIAN_POINT('Ctrl Pts',(-0.00180430162541425,-0.0202072965494324,
-0.00967556495540167));
#14778=CARTESIAN_POINT('Ctrl Pts',(-0.0019990857039826,-0.0202200320948226,
-0.00982845974830203));
#14779=CARTESIAN_POINT('Ctrl Pts',(-0.00217262904748856,-0.0202327676402129,
-0.010001897152684));
#14780=CARTESIAN_POINT('Ctrl Pts',(-0.00256679037826628,-0.0202616933219348,
-0.0103958178686086));
#14781=CARTESIAN_POINT('Ctrl Pts',(-0.00285205908546481,-0.0202906190036567,
-0.0109013045649633));
#14782=CARTESIAN_POINT('Ctrl Pts',(-0.00298511565851904,-0.0203195446853786,
-0.011444083681242));
#14783=CARTESIAN_POINT('Ctrl Pts',(-0.00304372350086436,-0.0203322856703234,
-0.0116831632858417));
#14784=CARTESIAN_POINT('Ctrl Pts',(-0.00307339537122476,-0.0203450266552681,
-0.0119291032718217));
#14785=CARTESIAN_POINT('Ctrl Pts',(-0.00307349972222446,-0.0203577676402129,
-0.0121745465784101));
#14786=CARTESIAN_POINT('Ctrl Pts',(-0.00307373662885434,-0.0203866933219348,
-0.0127317731192086));
#14787=CARTESIAN_POINT('Ctrl Pts',(-0.00291810289228469,-0.0204156190036567,
-0.0132909338655017));
#14788=CARTESIAN_POINT('Ctrl Pts',(-0.00262844071992795,-0.0204445446853786,
-0.0137688698061914));
#14789=CARTESIAN_POINT('Ctrl Pts',(-0.00250085232244247,-0.0204572856703233,
-0.0139793877356718));
#14790=CARTESIAN_POINT('Ctrl Pts',(-0.00234794665639152,-0.0204700266552681,
-0.0141743021870652));
#14791=CARTESIAN_POINT('Ctrl Pts',(-0.00217447679040723,-0.0204827676402129,
-0.0143479612346077));
#14792=CARTESIAN_POINT('Ctrl Pts',(-0.00178057649523043,-0.0205116987614893,
-0.014742291106825));
#14793=CARTESIAN_POINT('Ctrl Pts',(-0.00127504987507543,-0.0205406298827657,
-0.0150277090280041));
#14794=CARTESIAN_POINT('Ctrl Pts',(-0.000732186943210237,-0.0205695610040421,
-0.0151608666081686));
#14795=CARTESIAN_POINT('Ctrl Pts',(-0.000493217445851103,-0.0205822965494324,
-0.0152194828778265));
#14796=CARTESIAN_POINT('Ctrl Pts',(-0.000247387599726067,-0.0205950320948226,
-0.0152491894961984));
#14797=CARTESIAN_POINT('Ctrl Pts',(-2.04334081728397E-6,-0.0206077676402129,
-0.0152493526073256));
#14798=CARTESIAN_POINT('Ctrl Pts',(0.000553247367328469,-0.0206365921582588,
-0.0152497217787654));
#14799=CARTESIAN_POINT('Ctrl Pts',(0.00111065478973551,-0.0206654166763048,
-0.0150952680060627));
#14800=CARTESIAN_POINT('Ctrl Pts',(0.00158751295250971,-0.0206942411943507,
-0.0148076216797899));
#14801=CARTESIAN_POINT('Ctrl Pts',(0.00179996692615825,-0.0207070833429714,
-0.0146794670002799));
#14802=CARTESIAN_POINT('Ctrl Pts',(0.00199658834590345,-0.0207199254915922,
-0.0145255745727847));
#14803=CARTESIAN_POINT('Ctrl Pts',(0.00217158672383872,-0.0207327676402129,
-0.0143508506085903));
#14804=CARTESIAN_POINT('Ctrl Pts',(0.00257174658650591,-0.0207621331262766,
-0.0139513182338244));
#14805=CARTESIAN_POINT('Ctrl Pts',(0.002859574810257,-0.0207914986123403,
-0.013437319424777));
#14806=CARTESIAN_POINT('Ctrl Pts',(0.00299053940595569,-0.020820864098404,
-0.0128851320127484));
#14807=CARTESIAN_POINT('Ctrl Pts',(0.00304540037916721,-0.020833165279007,
-0.0126538211103063));
#14808=CARTESIAN_POINT('Ctrl Pts',(0.0030732839097424,-0.0208454664596099,
-0.0124161495675305));
#14809=CARTESIAN_POINT('Ctrl Pts',(0.00307349874276012,-0.0208577676402129,
-0.0121786332599273));
#14810=CARTESIAN_POINT('',(0.00307349991751608,-0.0218577417662807,-0.0121753484333405));
#14811=CARTESIAN_POINT('Ctrl Pts',(0.00307349999999104,-0.0208579110364346,
-0.0121758607060226));
#14812=CARTESIAN_POINT('Ctrl Pts',(0.00307350136873632,-0.0208872481983145,
-0.0116088604069139));
#14813=CARTESIAN_POINT('Ctrl Pts',(0.002912300834902,-0.0209165870425929,
-0.0110417211748914));
#14814=CARTESIAN_POINT('Ctrl Pts',(0.00261419119460617,-0.020945931248704,
-0.0105595591771697));
#14815=CARTESIAN_POINT('Ctrl Pts',(0.002489269261174,-0.0209582278485684,
-0.0103575106660141));
#14816=CARTESIAN_POINT('Ctrl Pts',(0.00234093045349195,-0.0209705253899725,
-0.010170212365268));
#14817=CARTESIAN_POINT('Ctrl Pts',(0.0021733835198766,-0.0209828241436666,
-0.0100026514262771));
#14818=CARTESIAN_POINT('Ctrl Pts',(0.00178092303245176,-0.0210116326378917,
-0.00961015813278175));
#14819=CARTESIAN_POINT('Ctrl Pts',(0.00127751376905249,-0.0210404477837066,
-0.00932548613589601));
#14820=CARTESIAN_POINT('Ctrl Pts',(0.000736769023118917,-0.0210692591418753,
-0.00919196762243281));
#14821=CARTESIAN_POINT('Ctrl Pts',(0.000495761426462938,-0.0210821002397146,
-0.00913245899792775));
#14822=CARTESIAN_POINT('Ctrl Pts',(0.000247725386902452,-0.0210949405851584,
-0.00910237237716682));
#14823=CARTESIAN_POINT('Ctrl Pts',(2.36968295708491E-7,-0.0211077792539681,
-0.00910235329569328));
#14824=CARTESIAN_POINT('Ctrl Pts',(-0.00055708584513428,-0.021136690841274,
-0.00910231032584208));
#14825=CARTESIAN_POINT('Ctrl Pts',(-0.00111627223786569,-0.0211655939261682,
-0.00925819074347665));
#14826=CARTESIAN_POINT('Ctrl Pts',(-0.00159415131407735,-0.0211945272086743,
-0.00954810066543382));
#14827=CARTESIAN_POINT('Ctrl Pts',(-0.00180461465842751,-0.0212072697531848,
-0.00967578027053203));
#14828=CARTESIAN_POINT('Ctrl Pts',(-0.0019994633841539,-0.0212200181548879,
-0.00982877033427998));
#14829=CARTESIAN_POINT('Ctrl Pts',(-0.00217304838425305,-0.0212327757196597,
-0.0100023163143179));
#14830=CARTESIAN_POINT('Ctrl Pts',(-0.00256719098401647,-0.0212617430828706,
-0.0103963703150181));
#14831=CARTESIAN_POINT('Ctrl Pts',(-0.00285238515458049,-0.0212907576875417,
-0.0109019971240844));
#14832=CARTESIAN_POINT('Ctrl Pts',(-0.00298531443795843,-0.021319675288494,
-0.011444895041159));
#14833=CARTESIAN_POINT('Ctrl Pts',(-0.00304385815732449,-0.0213324109617171,
-0.0116839940755777));
#14834=CARTESIAN_POINT('Ctrl Pts',(-0.00307346370977526,-0.0213451278197905,
-0.0119299475821563));
#14835=CARTESIAN_POINT('Ctrl Pts',(-0.00307349996646892,-0.0213578135407414,
-0.0121753992870766));
#14836=CARTESIAN_POINT('Ctrl Pts',(-0.00307358227467943,-0.0213866120572328,
-0.0127326119988626));
#14837=CARTESIAN_POINT('Ctrl Pts',(-0.00291780077213178,-0.0214152501057386,
-0.0132917289026298));
#14838=CARTESIAN_POINT('Ctrl Pts',(-0.00262800217461437,-0.0214439139712749,
-0.0137695931713016));
#14839=CARTESIAN_POINT('Ctrl Pts',(-0.00250028916401618,-0.0214565460150266,
-0.0139801859241036));
#14840=CARTESIAN_POINT('Ctrl Pts',(-0.00234723536954019,-0.0214691830727747,
-0.0141751538149292));
#14841=CARTESIAN_POINT('Ctrl Pts',(-0.00217360204790616,-0.0214818410884174,
-0.0143488365785643));
#14842=CARTESIAN_POINT('Ctrl Pts',(-0.00177962843165187,-0.0215105620974404,
-0.0147429223786078));
#14843=CARTESIAN_POINT('Ctrl Pts',(-0.00127410374523453,-0.0215393910050567,
-0.0150281122649468));
#14844=CARTESIAN_POINT('Ctrl Pts',(-0.000731298271848334,-0.0215682772307582,
-0.0151610844480583));
#14845=CARTESIAN_POINT('Ctrl Pts',(-0.000492037458318172,-0.0215810098618757,
-0.0152196966660038));
#14846=CARTESIAN_POINT('Ctrl Pts',(-0.000245908898367081,-0.0215937536294333,
-0.0152493304427505));
#14847=CARTESIAN_POINT('Ctrl Pts',(-2.85679979158681E-7,-0.0216065042016624,
-0.0152493532732812));
#14848=CARTESIAN_POINT('Ctrl Pts',(0.000555014508283015,-0.021635330447022,
-0.0152494048881004));
#14849=CARTESIAN_POINT('Ctrl Pts',(0.00111234191860738,-0.0216641914719324,
-0.0150946272716086));
#14850=CARTESIAN_POINT('Ctrl Pts',(0.00158904050890284,-0.0216931009275372,
-0.0148066996353717));
#14851=CARTESIAN_POINT('Ctrl Pts',(0.00180156125657449,-0.021705989279307,
-0.0146783363513719));
#14852=CARTESIAN_POINT('Ctrl Pts',(0.00199821333105363,-0.0217188872568502,
-0.0145242100967846));
#14853=CARTESIAN_POINT('Ctrl Pts',(0.00217319805514847,-0.0217317960697658,
-0.0143492406112425));
#14854=CARTESIAN_POINT('Ctrl Pts',(0.00257305896431553,-0.0217612942427944,
-0.0139494145239813));
#14855=CARTESIAN_POINT('Ctrl Pts',(0.00286050574081673,-0.0217908489956305,
-0.0134352059308452));
#14856=CARTESIAN_POINT('Ctrl Pts',(0.00299106214730737,-0.0218204555171494,
-0.0128829243444759));
#14857=CARTESIAN_POINT('Ctrl Pts',(0.00304579179865083,-0.0218328666629811,
-0.0126514061870918));
#14858=CARTESIAN_POINT('Ctrl Pts',(0.00307350020926293,-0.021845286906188,
-0.0124135380719837));
#14859=CARTESIAN_POINT('Ctrl Pts',(0.00307349999999881,-0.0218577158923484,
-0.0121758505805963));
#14860=CARTESIAN_POINT('',(0.00307349949439479,-0.0228577072780383,-0.01217458316111));
#14861=CARTESIAN_POINT('Ctrl Pts',(0.00307349983503335,-0.0218577676402129,
-0.0121748462860847));
#14862=CARTESIAN_POINT('Ctrl Pts',(0.00307331406363246,-0.0218871263583065,
-0.0116078471782629));
#14863=CARTESIAN_POINT('Ctrl Pts',(0.00291192699341664,-0.0219164850764001,
-0.0110407622690103));
#14864=CARTESIAN_POINT('Ctrl Pts',(0.00261365940606214,-0.0219458437944937,
-0.0105586993795032));
#14865=CARTESIAN_POINT('Ctrl Pts',(0.00248867160359435,-0.0219581464442396,
-0.0103566929136141));
#14866=CARTESIAN_POINT('Ctrl Pts',(0.00234027201046346,-0.0219704490939856,
-0.0101694442405646));
#14867=CARTESIAN_POINT('Ctrl Pts',(0.00217267097699875,-0.0219827517437315,
-0.0100019390574066));
#14868=CARTESIAN_POINT('Ctrl Pts',(0.00178008169618916,-0.0220115695160087,
-0.00960957429671008));
#14869=CARTESIAN_POINT('Ctrl Pts',(0.00127657885878497,-0.022040387288286,
-0.00932506722177673));
#14870=CARTESIAN_POINT('Ctrl Pts',(0.000735789944503822,-0.0220692050605632,
-0.00919172604269481));
#14871=CARTESIAN_POINT('Ctrl Pts',(0.000494769436991987,-0.0220820486561255,
-0.00913229812580182));
#14872=CARTESIAN_POINT('Ctrl Pts',(0.000246730499174395,-0.0220948922516879,
-0.00910229288898429));
#14873=CARTESIAN_POINT('Ctrl Pts',(-7.5122358097326E-7,-0.0221077358472502,
-0.00910235337836497));
#14874=CARTESIAN_POINT('Ctrl Pts',(-0.000558091349644402,-0.0221366602101895,
-0.00910248960320891));
#14875=CARTESIAN_POINT('Ctrl Pts',(-0.00111724334613616,-0.0221655845731287,
-0.00925855919309804));
#14876=CARTESIAN_POINT('Ctrl Pts',(-0.00159503904782892,-0.022194508936068,
-0.00954863942280413));
#14877=CARTESIAN_POINT('Ctrl Pts',(-0.00180543905582782,-0.0222072459409683,
-0.00967637787343116));
#14878=CARTESIAN_POINT('Ctrl Pts',(-0.00200021915344352,-0.0222199829458685,
-0.0098294167504658));
#14879=CARTESIAN_POINT('Ctrl Pts',(-0.00217373341178053,-0.0222327199507688,
-0.0100030014037762));
#14880=CARTESIAN_POINT('Ctrl Pts',(-0.00256769153989136,-0.0222616388802927,
-0.0103971193612416));
#14881=CARTESIAN_POINT('Ctrl Pts',(-0.00285270257510404,-0.0222905578098167,
-0.0109027469575032));
#14882=CARTESIAN_POINT('Ctrl Pts',(-0.00298548448088764,-0.0223194767393406,
-0.0114455898653332));
#14883=CARTESIAN_POINT('Ctrl Pts',(-0.00304399166879977,-0.0223322191776562,
-0.0116847806784771));
#14884=CARTESIAN_POINT('Ctrl Pts',(-0.0030735395388613,-0.0223449616159718,
-0.0119308219663486));
#14885=CARTESIAN_POINT('Ctrl Pts',(-0.00307349996006712,-0.0223577040542874,
-0.0121763487332415));
#14886=CARTESIAN_POINT('Ctrl Pts',(-0.00307341013610005,-0.0223866229838114,
-0.0127335710710829));
#14887=CARTESIAN_POINT('Ctrl Pts',(-0.00291745083476184,-0.0224155419133353,
-0.0132926370849982));
#14888=CARTESIAN_POINT('Ctrl Pts',(-0.00262751193933117,-0.0224444608428593,
-0.013770401265978));
#14889=CARTESIAN_POINT('Ctrl Pts',(-0.00249975726268389,-0.0224572032811749,
-0.0139809166863533));
#14890=CARTESIAN_POINT('Ctrl Pts',(-0.00234667702880692,-0.0224699457194905,
-0.0141758031377059));
#14891=CARTESIAN_POINT('Ctrl Pts',(-0.00217303277351682,-0.0224826881578061,
-0.0143494058659133));
#14892=CARTESIAN_POINT('Ctrl Pts',(-0.00177887356019078,-0.0225116125207454,
-0.0147434708159295));
#14893=CARTESIAN_POINT('Ctrl Pts',(-0.00127316145523074,-0.0225405368836846,
-0.0150285519019311));
#14894=CARTESIAN_POINT('Ctrl Pts',(-0.000730214003843846,-0.0225694612466239,
-0.015161349854734));
#14895=CARTESIAN_POINT('Ctrl Pts',(-0.000491124058685119,-0.0225821982515242,
-0.0152198281755582));
#14896=CARTESIAN_POINT('Ctrl Pts',(-0.000245188176706377,-0.0225949352564245,
-0.0152493724155374));
#14897=CARTESIAN_POINT('Ctrl Pts',(2.39669782465268E-7,-0.0226076722613247,
-0.0152493532772134));
#14898=CARTESIAN_POINT('Ctrl Pts',(0.000555525927892844,-0.0226364900336019,
-0.0152493099763066));
#14899=CARTESIAN_POINT('Ctrl Pts',(0.00111281481403792,-0.0226653078058792,
-0.0150944446411238));
#14900=CARTESIAN_POINT('Ctrl Pts',(0.00158945717892497,-0.0226941255781564,
-0.0148064479201655));
#14901=CARTESIAN_POINT('Ctrl Pts',(0.00180188865015705,-0.0227069691737187,
-0.014678092634001));
#14902=CARTESIAN_POINT('Ctrl Pts',(0.00199845769115906,-0.0227198127692811,
-0.014523993699976));
#14903=CARTESIAN_POINT('Ctrl Pts',(0.00217337173187688,-0.0227326563648434,
-0.0143490669357602));
#14904=CARTESIAN_POINT('Ctrl Pts',(0.00257320151374196,-0.022762015082937,
-0.0139492080697039));
#14905=CARTESIAN_POINT('Ctrl Pts',(0.00286060724971039,-0.0227913738010306,
-0.0134349755781676));
#14906=CARTESIAN_POINT('Ctrl Pts',(0.00299111920455669,-0.0228207325191242,
-0.0128826829365673));
#14907=CARTESIAN_POINT('Ctrl Pts',(0.00304580970102223,-0.0228330351688702,
-0.0126512469826813));
#14908=CARTESIAN_POINT('Ctrl Pts',(0.00307349875478779,-0.0228453378186161,
-0.0124134680443367));
#14909=CARTESIAN_POINT('Ctrl Pts',(0.00307349999995779,-0.022857640468362,
-0.0121758693936782));
#14910=CARTESIAN_POINT('',(0.00307349962338454,-0.0238578241218712,-0.0121769184793798));
#14911=CARTESIAN_POINT('Ctrl Pts',(0.0030734990376214,-0.022857767640213,
-0.0121734210570659));
#14912=CARTESIAN_POINT('Ctrl Pts',(0.00307305033695564,-0.0228871357094251,
-0.0116064182027534));
#14913=CARTESIAN_POINT('Ctrl Pts',(0.00291139821148099,-0.0229165037786371,
-0.0110394049233265));
#14914=CARTESIAN_POINT('Ctrl Pts',(0.00261290357933612,-0.0229458718478492,
-0.0105574784427433));
#14915=CARTESIAN_POINT('Ctrl Pts',(0.00248790164963457,-0.0229581704453038,
-0.0103556599389589));
#14916=CARTESIAN_POINT('Ctrl Pts',(0.00233952495234875,-0.0229704690427584,
-0.0101685910649555));
#14917=CARTESIAN_POINT('Ctrl Pts',(0.0021719776110592,-0.022982767640213,
-0.010001246308951));
#14918=CARTESIAN_POINT('Ctrl Pts',(0.00177925715436449,-0.023011594781079,
-0.00960900069945493));
#14919=CARTESIAN_POINT('Ctrl Pts',(0.0012756555475673,-0.0230404219219451,
-0.00932465262100666));
#14920=CARTESIAN_POINT('Ctrl Pts',(0.000734816597786818,-0.0230692490628111,
-0.0091914862150307));
#14921=CARTESIAN_POINT('Ctrl Pts',(0.000493928481897427,-0.0230820885886117,
-0.00913217428002985));
#14922=CARTESIAN_POINT('Ctrl Pts',(0.000246040397300628,-0.0230949281144124,
-0.0091022500497725));
#14923=CARTESIAN_POINT('Ctrl Pts',(-1.28625627569396E-6,-0.023107767640213,
-0.00910235355570651));
#14924=CARTESIAN_POINT('Ctrl Pts',(-0.000558634401779208,-0.0231367013834657,
-0.0091025868052958));
#14925=CARTESIAN_POINT('Ctrl Pts',(-0.00111776564145458,-0.0231656351267184,
-0.00925875804508432));
#14926=CARTESIAN_POINT('Ctrl Pts',(-0.00159551432548366,-0.0231945688699711,
-0.00954892803311513));
#14927=CARTESIAN_POINT('Ctrl Pts',(-0.00180575803130939,-0.0232073017933851,
-0.00967662365142329));
#14928=CARTESIAN_POINT('Ctrl Pts',(-0.00200039715527956,-0.023220034716799,
-0.00982958467417083));
#14929=CARTESIAN_POINT('Ctrl Pts',(-0.0021737969912177,-0.023232767640213,
-0.0100030650108688));
#14930=CARTESIAN_POINT('Ctrl Pts',(-0.0025677491220947,-0.0232616959392744,
-0.0103972000337635));
#14931=CARTESIAN_POINT('Ctrl Pts',(-0.00285274681297765,-0.0232906242383358,
-0.0109028433512128));
#14932=CARTESIAN_POINT('Ctrl Pts',(-0.00298551070465185,-0.0233195525373972,
-0.011445697082442));
#14933=CARTESIAN_POINT('Ctrl Pts',(-0.00304397232568449,-0.0233322909050025,
-0.0116847388031318));
#14934=CARTESIAN_POINT('Ctrl Pts',(-0.00307351119625606,-0.0233450292726077,
-0.0119306212724117));
#14935=CARTESIAN_POINT('Ctrl Pts',(-0.00307349999679855,-0.0233577676402129,
-0.0121759935694385));
#14936=CARTESIAN_POINT('Ctrl Pts',(-0.00307347456329985,-0.0233866959392743,
-0.0127332237742619));
#14937=CARTESIAN_POINT('Ctrl Pts',(-0.00291757565825456,-0.0234156242383358,
-0.0132923140642119));
#14938=CARTESIAN_POINT('Ctrl Pts',(-0.00262768555746732,-0.0234445525373972,
-0.0137701151411722));
#14939=CARTESIAN_POINT('Ctrl Pts',(-0.00250003454483423,-0.0234572909050024,
-0.013980511395289));
#14940=CARTESIAN_POINT('Ctrl Pts',(-0.00234708845669796,-0.0234700292726077,
-0.0141753013142027));
#14941=CARTESIAN_POINT('Ctrl Pts',(-0.0021735986382546,-0.0234827676402129,
-0.0143488399891814));
#14942=CARTESIAN_POINT('Ctrl Pts',(-0.00177953638323401,-0.0235117013834656,
-0.0147430132162271));
#14943=CARTESIAN_POINT('Ctrl Pts',(-0.00127389095929958,-0.0235406351267183,
-0.0150282274685925));
#14944=CARTESIAN_POINT('Ctrl Pts',(-0.00073097096784502,-0.023569568869971,
-0.0151611646093798));
#14945=CARTESIAN_POINT('Ctrl Pts',(-0.000492047209839665,-0.023582301793385,
-0.0152196664913428));
#14946=CARTESIAN_POINT('Ctrl Pts',(-0.000246278880082321,-0.0235950347167989,
-0.0152492728653299));
#14947=CARTESIAN_POINT('Ctrl Pts',(-1.00569053437863E-6,-0.0236077676402129,
-0.0152493531220204));
#14948=CARTESIAN_POINT('Ctrl Pts',(0.00055428900149266,-0.0236365947810789,
-0.0152495348219213));
#14949=CARTESIAN_POINT('Ctrl Pts',(0.0011116473574554,-0.023665421921945,
-0.0150948907950721));
#14950=CARTESIAN_POINT('Ctrl Pts',(0.00158841008506312,-0.023694249062811,
-0.0148070803105281));
#14951=CARTESIAN_POINT('Ctrl Pts',(0.00180075883551153,-0.0237070885886116,
-0.0146788903468001));
#14952=CARTESIAN_POINT('Ctrl Pts',(0.00199727549648617,-0.0237199281144123,
-0.0145249830204326));
#14953=CARTESIAN_POINT('Ctrl Pts',(0.0021721761119366,-0.0237327676402129,
-0.0143502619852006));
#14954=CARTESIAN_POINT('Ctrl Pts',(0.00257222931168367,-0.023762135709425,
-0.0139506195423898));
#14955=CARTESIAN_POINT('Ctrl Pts',(0.00285991854711518,-0.023791503778637,
-0.0134365406511251));
#14956=CARTESIAN_POINT('Ctrl Pts',(0.00299073283294949,-0.0238208718478491,
-0.0128843159686508));
#14957=CARTESIAN_POINT('Ctrl Pts',(0.00304551451543502,-0.0238331704453037,
-0.0126530583730217));
#14958=CARTESIAN_POINT('Ctrl Pts',(0.00307333301785099,-0.0238454690427583,
-0.0124154512831565));
#14959=CARTESIAN_POINT('Ctrl Pts',(0.00307349924684273,-0.0238577676402129,
-0.0121780049503674));
#14960=CARTESIAN_POINT('',(0.00307349967665051,-0.0248577676402129,-0.012177263119607));
#14961=CARTESIAN_POINT('Ctrl Pts',(0.00307349999992634,-0.0238578806035296,
-0.0121758320083923));
#14962=CARTESIAN_POINT('Ctrl Pts',(0.00307349607452821,-0.0238872403822584,
-0.0116088324239896));
#14963=CARTESIAN_POINT('Ctrl Pts',(0.00291229064502768,-0.0239166001609873,
-0.0110416954096486));
#14964=CARTESIAN_POINT('Ctrl Pts',(0.00261417727345869,-0.0239459599397161,
-0.0105595366613475));
#14965=CARTESIAN_POINT('Ctrl Pts',(0.0024892633655894,-0.0239582621208491,
-0.0103575050210133));
#14966=CARTESIAN_POINT('Ctrl Pts',(0.00234093639568344,-0.0239705643019821,
-0.0101702214871738));
#14967=CARTESIAN_POINT('Ctrl Pts',(0.0021734041367439,-0.023982866483115,
-0.0100026720450634));
#14968=CARTESIAN_POINT('Ctrl Pts',(0.00178094653157099,-0.0240116853182242,
-0.00961017418694974));
#14969=CARTESIAN_POINT('Ctrl Pts',(0.00127753876572544,-0.0240405041533333,
-0.00932549710950571));
#14970=CARTESIAN_POINT('Ctrl Pts',(0.000736793995285274,-0.0240693229884425,
-0.00919197378857036));
#14971=CARTESIAN_POINT('Ctrl Pts',(0.000495810884073522,-0.0240821661131951,
-0.00913246907015739));
#14972=CARTESIAN_POINT('Ctrl Pts',(0.000247800461736436,-0.0240950092379478,
-0.00910238039836973));
#14973=CARTESIAN_POINT('Ctrl Pts',(3.36499649636908E-7,-0.0241078523627004,
-0.00910235330497879));
#14974=CARTESIAN_POINT('Ctrl Pts',(-0.00055700456237791,-0.0241367777897768,
-0.00910229228494521));
#14975=CARTESIAN_POINT('Ctrl Pts',(-0.00111621249341672,-0.0241657032168533,
-0.00925816447319608));
#14976=CARTESIAN_POINT('Ctrl Pts',(-0.00159411122558648,-0.0241946286439297,
-0.00954807634578493));
#14977=CARTESIAN_POINT('Ctrl Pts',(-0.00180454106139394,-0.0242073651767151,
-0.00967573123089108));
#14978=CARTESIAN_POINT('Ctrl Pts',(-0.00199936220140598,-0.0242201017095004,
-0.00982868836518448));
#14979=CARTESIAN_POINT('Ctrl Pts',(-0.00217292822667836,-0.0242328382422858,
-0.010002196190394));
#14980=CARTESIAN_POINT('Ctrl Pts',(-0.00256703298197344,-0.024261758234714,
-0.0103961687947023));
#14981=CARTESIAN_POINT('Ctrl Pts',(-0.00285223149793234,-0.0242906782271423,
-0.0109016916062154));
#14982=CARTESIAN_POINT('Ctrl Pts',(-0.00298521427273911,-0.0243195982195706,
-0.0114444860765776));
#14983=CARTESIAN_POINT('Ctrl Pts',(-0.00304380564996769,-0.0243323401870041,
-0.0116836379187375));
#14984=CARTESIAN_POINT('Ctrl Pts',(-0.00307344446317736,-0.0243450821544377,
-0.0119296499451585));
#14985=CARTESIAN_POINT('Ctrl Pts',(-0.00307349992158432,-0.0243578241218712,
-0.0121751590090976));
#14986=CARTESIAN_POINT('Ctrl Pts',(-0.00307362579356741,-0.0243867441142995,
-0.0127323822406914));
#14987=CARTESIAN_POINT('Ctrl Pts',(-0.00291788243124792,-0.0244156641067277,
-0.0132915093003472));
#14988=CARTESIAN_POINT('Ctrl Pts',(-0.00262812776063055,-0.0244445840991559,
-0.0137693860674581));
#14989=CARTESIAN_POINT('Ctrl Pts',(-0.00250046366853621,-0.0244573260665895,
-0.0139799355763797));
#14990=CARTESIAN_POINT('Ctrl Pts',(-0.00234747167256663,-0.0244700680340231,
-0.0141748681784755));
#14991=CARTESIAN_POINT('Ctrl Pts',(-0.0021739100261297,-0.0244828100014566,
-0.0143485284689756));
#14992=CARTESIAN_POINT('Ctrl Pts',(-0.00177990927440443,-0.0245117354285331,
-0.0147427531517122));
#14993=CARTESIAN_POINT('Ctrl Pts',(-0.00127431142674241,-0.0245406608556095,
-0.0150280385348234));
#14994=CARTESIAN_POINT('Ctrl Pts',(-0.000731416810373939,-0.024569586282686,
-0.0151610554069349));
#14995=CARTESIAN_POINT('Ctrl Pts',(-0.000492367787447086,-0.0245823228154714,
-0.0152196258041213));
#14996=CARTESIAN_POINT('Ctrl Pts',(-0.0002464621685526,-0.0245950593482567,
-0.0152492691029153));
#14997=CARTESIAN_POINT('Ctrl Pts',(-1.05205526183687E-6,-0.0246077958810421,
-0.0152493531064995));
#14998=CARTESIAN_POINT('Ctrl Pts',(0.000554235141673008,-0.0246366147161513,
-0.0152495431806337));
#14999=CARTESIAN_POINT('Ctrl Pts',(0.00111158984035125,-0.0246654335512604,
-0.0150949115582599));
#15000=CARTESIAN_POINT('Ctrl Pts',(0.0015883536267387,-0.0246942523863696,
-0.0148071143922688));
#15001=CARTESIAN_POINT('Ctrl Pts',(0.00180082358823867,-0.0247070955111222,
-0.0146788574765302));
#15002=CARTESIAN_POINT('Ctrl Pts',(0.00199744422213352,-0.0247199386358749,
-0.0145248539977468));
#15003=CARTESIAN_POINT('Ctrl Pts',(0.00217242210871539,-0.0247327817606275,
-0.0143500162131955));
#15004=CARTESIAN_POINT('Ctrl Pts',(0.00257242694643423,-0.0247621415393563,
-0.0139503316530336));
#15005=CARTESIAN_POINT('Ctrl Pts',(0.00286005738988455,-0.0247915013180852,
-0.0134362242481947));
#15006=CARTESIAN_POINT('Ctrl Pts',(0.00299081045101602,-0.024820861096814,
-0.0128839882285666));
#15007=CARTESIAN_POINT('Ctrl Pts',(0.00304559791575083,-0.024833163277947,
-0.0126525931760236));
#15008=CARTESIAN_POINT('Ctrl Pts',(0.00307339069671438,-0.0248454654590799,
-0.0124148442989605));
#15009=CARTESIAN_POINT('Ctrl Pts',(0.00307349967665051,-0.0248577676402129,
-0.012177263119607));
#15010=CARTESIAN_POINT('',(0.00307349906472614,-0.0258577432759482,-0.0121736790431998));
#15011=CARTESIAN_POINT('Ctrl Pts',(0.00307349999999773,-0.0248578401021784,
-0.0121758570261513));
#15012=CARTESIAN_POINT('Ctrl Pts',(0.00307350068537023,-0.0248869104153856,
-0.0116125624938714));
#15013=CARTESIAN_POINT('Ctrl Pts',(0.00291433569470665,-0.0249159966875591,
-0.0110488238096736));
#15014=CARTESIAN_POINT('Ctrl Pts',(0.00261987280316784,-0.0249450991055997,
-0.010568784916755));
#15015=CARTESIAN_POINT('Ctrl Pts',(0.00249371145037095,-0.0249575679107875,
-0.0103631143284876));
#15016=CARTESIAN_POINT('Ctrl Pts',(0.00234336379447851,-0.0249700396798027,
-0.0101726336832762));
#15017=CARTESIAN_POINT('Ctrl Pts',(0.00217330538285328,-0.0249825144273446,
-0.0100025732855318));
#15018=CARTESIAN_POINT('Ctrl Pts',(0.00177902926068591,-0.0250114368137107,
-0.00960829255859728));
#15019=CARTESIAN_POINT('Ctrl Pts',(0.00127275405917176,-0.0250403752106253,
-0.00932273579918919));
#15020=CARTESIAN_POINT('Ctrl Pts',(0.000728558695200731,-0.0250693290685143,
-0.00918995233748972));
#15021=CARTESIAN_POINT('Ctrl Pts',(0.000490182471258236,-0.0250820118507816,
-0.0091317886295688));
#15022=CARTESIAN_POINT('Ctrl Pts',(0.000244909984473728,-0.0250946975996085,
-0.00910235423995953));
#15023=CARTESIAN_POINT('Ctrl Pts',(1.19650119577734E-8,-0.0251073862688045,
-0.00910235328658139));
#15024=CARTESIAN_POINT('Ctrl Pts',(-0.000401979116139882,-0.0251282142520593,
-0.00910235172164627));
#15025=CARTESIAN_POINT('Ctrl Pts',(-0.000804358817299954,-0.0251490501039609,
-0.00918229846194574));
#15026=CARTESIAN_POINT('Ctrl Pts',(-0.00117616923873007,-0.0251698958673943,
-0.00933630610930164));
#15027=CARTESIAN_POINT('Ctrl Pts',(-0.00154797966016019,-0.0251907416308277,
-0.00949031375665754));
#15028=CARTESIAN_POINT('Ctrl Pts',(-0.00188889080179529,-0.025211597305793,
-0.00971815981154555));
#15029=CARTESIAN_POINT('Ctrl Pts',(-0.00217328846173606,-0.0252324545845573,
-0.0100025563643487));
#15030=CARTESIAN_POINT('Ctrl Pts',(-0.00231548729170644,-0.0252428832239394,
-0.0101447546407502));
#15031=CARTESIAN_POINT('Ctrl Pts',(-0.00244370560832201,-0.0252533122642713,
-0.0103009638674558));
#15032=CARTESIAN_POINT('Ctrl Pts',(-0.00255551936065739,-0.0252637523626038,
-0.0104683044447075));
#15033=CARTESIAN_POINT('Ctrl Pts',(-0.00266733311299277,-0.0252741924609363,
-0.0106356450219593));
#15034=CARTESIAN_POINT('Ctrl Pts',(-0.00276269865287568,-0.0252846436172694,
-0.0108141558086635));
#15035=CARTESIAN_POINT('Ctrl Pts',(-0.00283954259848281,-0.0252950624202936,
-0.0109996729936602));
#15036=CARTESIAN_POINT('Ctrl Pts',(-0.00291638654408995,-0.0253054812233178,
-0.0111851901786568));
#15037=CARTESIAN_POINT('Ctrl Pts',(-0.00297492629622829,-0.0253158676730331,
-0.011377576989722));
#15038=CARTESIAN_POINT('Ctrl Pts',(-0.00301444326754076,-0.0253263847576267,
-0.0115762417149734));
#15039=CARTESIAN_POINT('Ctrl Pts',(-0.00303420175319699,-0.0253316432999235,
-0.0116755740775992));
#15040=CARTESIAN_POINT('Ctrl Pts',(-0.0030490409528902,-0.0253369345009398,
-0.0117765252855877));
#15041=CARTESIAN_POINT('Ctrl Pts',(-0.00305870018412946,-0.0253420505311595,
-0.0118745968615537));
#15042=CARTESIAN_POINT('Ctrl Pts',(-0.00306352979974909,-0.0253446085462694,
-0.0119236326495368));
#15043=CARTESIAN_POINT('Ctrl Pts',(-0.00306718850569586,-0.02534712276868,
-0.0119719298103766));
#15044=CARTESIAN_POINT('Ctrl Pts',(-0.00306979781630011,-0.0253498845691424,
-0.012025043416062));
#15045=CARTESIAN_POINT('Ctrl Pts',(-0.00307240712690437,-0.0253526463696048,
-0.0120781570217473));
#15046=CARTESIAN_POINT('Ctrl Pts',(-0.0030735,-0.025355655748119,-0.012136115688322));
#15047=CARTESIAN_POINT('Ctrl Pts',(-0.0030735,-0.0253577193746031,-0.0121758532865577));
#15048=CARTESIAN_POINT('Ctrl Pts',(-0.00307350000000001,-0.0253597830010872,
-0.0122155908847934));
#15049=CARTESIAN_POINT('Ctrl Pts',(-0.00307300554522283,-0.0253609008755414,
-0.0122371133043084));
#15050=CARTESIAN_POINT('Ctrl Pts',(-0.00307224100675227,-0.025362287812272,
-0.0122638160424823));
#15051=CARTESIAN_POINT('Ctrl Pts',(-0.00307147646828171,-0.0253636747490026,
-0.0122905187806561));
#15052=CARTESIAN_POINT('Ctrl Pts',(-0.00307016498421063,-0.0253653307480096,
-0.0123223895170306));
#15053=CARTESIAN_POINT('Ctrl Pts',(-0.0030683501683386,-0.0253669591928204,
-0.0123537001151958));
#15054=CARTESIAN_POINT('Ctrl Pts',(-0.00306472053659454,-0.0253702160824419,
-0.0124163213115264));
#15055=CARTESIAN_POINT('Ctrl Pts',(-0.00305937780406044,-0.0253733627552782,
-0.012476730769819));
#15056=CARTESIAN_POINT('Ctrl Pts',(-0.00305198487235182,-0.0253766107825558,
-0.0125388830221662));
#15057=CARTESIAN_POINT('Ctrl Pts',(-0.00303719900893458,-0.0253831068371111,
-0.0126631875268605));
#15058=CARTESIAN_POINT('Ctrl Pts',(-0.00301376367080274,-0.0253900083094319,
-0.0127943819767643));
#15059=CARTESIAN_POINT('Ctrl Pts',(-0.0029800853608862,-0.0253971492765809,
-0.0129278462997116));
#15060=CARTESIAN_POINT('Ctrl Pts',(-0.00294640705096966,-0.0254042902437299,
-0.013061310622659));
#15061=CARTESIAN_POINT('Ctrl Pts',(-0.00290263545605546,-0.0254116707057071,
-0.0131971045166008));
#15062=CARTESIAN_POINT('Ctrl Pts',(-0.00284694205880417,-0.0254193348566784,
-0.0133340083555415));
#15063=CARTESIAN_POINT('Ctrl Pts',(-0.00279124866155287,-0.0254269990076497,
-0.0134709121944821));
#15064=CARTESIAN_POINT('Ctrl Pts',(-0.00272359546920565,-0.0254349468476151,
-0.0136088948852597));
#15065=CARTESIAN_POINT('Ctrl Pts',(-0.00264256792344005,-0.0254431675228483,
-0.0137453235857373));
#15066=CARTESIAN_POINT('Ctrl Pts',(-0.00248051283190884,-0.0254596088733148,
-0.0140181809866926));
#15067=CARTESIAN_POINT('Ctrl Pts',(-0.00226469144760116,-0.0254771415648527,
-0.014284636089567));
#15068=CARTESIAN_POINT('Ctrl Pts',(-0.00199062313410204,-0.0254957741134054,
-0.0145176094198858));
#15069=CARTESIAN_POINT('Ctrl Pts',(-0.00171655482060292,-0.025514406661958,
-0.0147505827502045));
#15070=CARTESIAN_POINT('Ctrl Pts',(-0.00138383681775807,-0.0255341390675254,
-0.0149495290333914));
#15071=CARTESIAN_POINT('Ctrl Pts',(-0.00100354630252485,-0.0255549690482522,
-0.0150809001138379));
#15072=CARTESIAN_POINT('Ctrl Pts',(-0.000623255787291618,-0.025575799028979,
-0.0152122711942845));
#15073=CARTESIAN_POINT('Ctrl Pts',(-0.000195143521376919,-0.0255977265848653,
-0.015275248483919));
#15074=CARTESIAN_POINT('Ctrl Pts',(0.000248294841224699,-0.0256207523273886,
-0.0152393075332902));
#15075=CARTESIAN_POINT('Ctrl Pts',(0.000691733203826318,-0.0256437780699119,
-0.0152033665826615));
#15076=CARTESIAN_POINT('Ctrl Pts',(0.00115034288718135,-0.0256679019990723,
-0.01506735112295));
#15077=CARTESIAN_POINT('Ctrl Pts',(0.00156948119630631,-0.0256931239508147,
-0.0148184147379611));
#15078=CARTESIAN_POINT('Ctrl Pts',(0.00198861950543127,-0.0257183459025571,
-0.0145694783529722));
#15079=CARTESIAN_POINT('Ctrl Pts',(0.00236737253616329,-0.0257446658768816,
-0.0142063008048711));
#15080=CARTESIAN_POINT('Ctrl Pts',(0.00263898767146668,-0.0257720839185305,
-0.013751336171215));
#15081=CARTESIAN_POINT('Ctrl Pts',(0.00291059991413796,-0.0257995016681841,
-0.0132963763828165));
#15082=CARTESIAN_POINT('Ctrl Pts',(0.00307350131380818,-0.025828017461774,
-0.0127485450022714));
#15083=CARTESIAN_POINT('Ctrl Pts',(0.00307349999999191,-0.0258576312843864,
-0.012175846235706));
#15084=CARTESIAN_POINT('',(0.00307349999999503,-0.0268577565897941,-0.0121758588150803));
#15085=CARTESIAN_POINT('Ctrl Pts',(0.0030734988612549,-0.0258577676402129,
-0.0121732075607849));
#15086=CARTESIAN_POINT('Ctrl Pts',(0.00307301077635369,-0.0258871323359906,
-0.0116062068522265));
#15087=CARTESIAN_POINT('Ctrl Pts',(0.00291132040796627,-0.0259164970317683,
-0.0110392065771651));
#15088=CARTESIAN_POINT('Ctrl Pts',(0.00261279421991182,-0.025945861727546,
-0.0105573018927509));
#15089=CARTESIAN_POINT('Ctrl Pts',(0.00248773509955849,-0.0259581632380008,
-0.0103554215273472));
#15090=CARTESIAN_POINT('Ctrl Pts',(0.00233928586059097,-0.0259704647484557,
-0.0101683027370409));
#15091=CARTESIAN_POINT('Ctrl Pts',(0.00217165560515604,-0.0259827662589106,
-0.010000924740009));
#15092=CARTESIAN_POINT('Ctrl Pts',(0.00177888037096302,-0.0260115899854944,
-0.00960874057365779));
#15093=CARTESIAN_POINT('Ctrl Pts',(0.00127524104593229,-0.0260404137120782,
-0.00932446792274665));
#15094=CARTESIAN_POINT('Ctrl Pts',(0.000734386477435069,-0.0260692374386621,
-0.00919138034284417));
#15095=CARTESIAN_POINT('Ctrl Pts',(0.000493407443421635,-0.0260820799183108,
-0.00913208285639934));
#15096=CARTESIAN_POINT('Ctrl Pts',(0.000245427868459588,-0.0260949223979595,
-0.00910219430558744));
#15097=CARTESIAN_POINT('Ctrl Pts',(-1.98291230682416E-6,-0.0261077648776082,
-0.00910235392621023));
#15098=CARTESIAN_POINT('Ctrl Pts',(-0.000559326620774171,-0.0261366952063965,
-0.00910271350451791));
#15099=CARTESIAN_POINT('Ctrl Pts',(-0.00111841896355447,-0.0261656255351847,
-0.00925900913306373));
#15100=CARTESIAN_POINT('Ctrl Pts',(-0.00159609997232856,-0.026194555863973,
-0.00954928382653372));
#15101=CARTESIAN_POINT('Ctrl Pts',(-0.00180638748166665,-0.0262072917414173,
-0.00967707023878891));
#15102=CARTESIAN_POINT('Ctrl Pts',(-0.00200105397037653,-0.0262200276188616,
-0.00983013604509866));
#15103=CARTESIAN_POINT('Ctrl Pts',(-0.00217446016899265,-0.0262327634963059,
-0.0100037286990944));
#15104=CARTESIAN_POINT('Ctrl Pts',(-0.00256828896208452,-0.026261688386436,
-0.0103979809574239));
#15105=CARTESIAN_POINT('Ctrl Pts',(-0.00285313149746629,-0.0262906132765661,
-0.0109037072449803));
#15106=CARTESIAN_POINT('Ctrl Pts',(-0.00298573082506832,-0.0263195381666962,
-0.011446597713911));
#15107=CARTESIAN_POINT('Ctrl Pts',(-0.00304414037961968,-0.0263322794827987,
-0.0116857391261178));
#15108=CARTESIAN_POINT('Ctrl Pts',(-0.00307360514234931,-0.0263450207989011,
-0.0119317172695922));
#15109=CARTESIAN_POINT('Ctrl Pts',(-0.00307349971650223,-0.0263577621150035,
-0.0121771733853063));
#15110=CARTESIAN_POINT('Ctrl Pts',(-0.00307326038243195,-0.0263866870051336,
-0.0127343992732539));
#15111=CARTESIAN_POINT('Ctrl Pts',(-0.00291714915791347,-0.0264156118952638,
-0.0132934262821599));
#15112=CARTESIAN_POINT('Ctrl Pts',(-0.00262707914936251,-0.0264445367853939,
-0.0137711142034569));
#15113=CARTESIAN_POINT('Ctrl Pts',(-0.00249930429337674,-0.0264572781014963,
-0.0139815341143424));
#15114=CARTESIAN_POINT('Ctrl Pts',(-0.00234622283697911,-0.0264700194175988,
-0.0141763272798705));
#15115=CARTESIAN_POINT('Ctrl Pts',(-0.00217259346875283,-0.0264827607337012,
-0.0143498449768671));
#15116=CARTESIAN_POINT('Ctrl Pts',(-0.00177835203641551,-0.0265116910624894,
-0.0147438328494178));
#15117=CARTESIAN_POINT('Ctrl Pts',(-0.00127257886971661,-0.0265406213912777,
-0.0150288124134629));
#15118=CARTESIAN_POINT('Ctrl Pts',(-0.000729601329433494,-0.0265695517200659,
-0.0151614996403798));
#15119=CARTESIAN_POINT('Ctrl Pts',(-0.000490568601576626,-0.0265822875975102,
-0.0152199119824173));
#15120=CARTESIAN_POINT('Ctrl Pts',(-0.000244699846216731,-0.0265950234749545,
-0.0152494056872691));
#15121=CARTESIAN_POINT('Ctrl Pts',(6.57285128261936E-7,-0.0266077593523988,
-0.0152493532162761));
#15122=CARTESIAN_POINT('Ctrl Pts',(0.000555947401589652,-0.0266365830789827,
-0.0152492344643828));
#15123=CARTESIAN_POINT('Ctrl Pts',(0.00111321833243329,-0.0266654068055665,
-0.0150942913426623));
#15124=CARTESIAN_POINT('Ctrl Pts',(0.00158982325464466,-0.0266942305321503,
-0.0148062266952191));
#15125=CARTESIAN_POINT('Ctrl Pts',(0.0018021757065795,-0.0267070730117991,
-0.0146778788092668));
#15126=CARTESIAN_POINT('Ctrl Pts',(0.00199867134309933,-0.0267199154914478,
-0.0145238043854205));
#15127=CARTESIAN_POINT('Ctrl Pts',(0.00217352311052001,-0.0267327579710965,
-0.0143489155355596));
#15128=CARTESIAN_POINT('Ctrl Pts',(0.00257332666068658,-0.0267621226668742,
-0.0139490271953364));
#15129=CARTESIAN_POINT('Ctrl Pts',(0.00286069689813898,-0.0267914873626519,
-0.0134347726021502));
#15130=CARTESIAN_POINT('Ctrl Pts',(0.00299116973179934,-0.0268208520584295,
-0.012882469084264));
#15131=CARTESIAN_POINT('Ctrl Pts',(0.00304582764276496,-0.0268331535688844,
-0.0126510971146384));
#15132=CARTESIAN_POINT('Ctrl Pts',(0.00307349957273473,-0.0268454550793392,
-0.0124133878459035));
#15133=CARTESIAN_POINT('Ctrl Pts',(0.00307349999999503,-0.0268577565897941,
-0.0121758588150803));
#15134=CARTESIAN_POINT('',(-0.0013261977441873,-0.0271787743898721,-0.00940320080322876));
#15135=CARTESIAN_POINT('Ctrl Pts',(0.00307490613955397,-0.0268602076302924,
-0.012175775310944));
#15136=CARTESIAN_POINT('Ctrl Pts',(0.00307491292342961,-0.0268611376005165,
-0.012158051380771));
#15137=CARTESIAN_POINT('Ctrl Pts',(0.00307476249686456,-0.0268620613829282,
-0.0121403314445906));
#15138=CARTESIAN_POINT('Ctrl Pts',(0.00307445305337281,-0.0268629793711641,
-0.0121226174982785));
#15139=CARTESIAN_POINT('Ctrl Pts',(0.00306573943659914,-0.0268888289944517,
-0.0116238106277867));
#15140=CARTESIAN_POINT('Ctrl Pts',(0.00293065178342736,-0.0269100842487583,
-0.0111276312005785));
#15141=CARTESIAN_POINT('Ctrl Pts',(0.00268958940748811,-0.0269355342842967,
-0.0106913744809503));
#15142=CARTESIAN_POINT('Ctrl Pts',(0.00243996627138719,-0.0269618881176572,
-0.0102396251356849));
#15143=CARTESIAN_POINT('Ctrl Pts',(0.00207616383323794,-0.0269930635228418,
-0.0098502833634627));
#15144=CARTESIAN_POINT('Ctrl Pts',(0.00163926437820477,-0.0270202698942173,
-0.00957464222116215));
#15145=CARTESIAN_POINT('Ctrl Pts',(0.00163155978799815,-0.0270207496703764,
-0.00956978137269679));
#15146=CARTESIAN_POINT('Ctrl Pts',(0.00162383366347141,-0.0270212278936503,
-0.00956495627789788));
#15147=CARTESIAN_POINT('Ctrl Pts',(0.00161608611459192,-0.0270217046142949,
-0.0095601673085752));
#15148=CARTESIAN_POINT('Ctrl Pts',(0.00118449817741507,-0.0270482609978461,
-0.00929339114190244));
#15149=CARTESIAN_POINT('Ctrl Pts',(0.000684240449115547,-0.0270701544205097,
-0.00913816439777956));
#15150=CARTESIAN_POINT('Ctrl Pts',(0.000178117810484161,-0.0270960725546501,
-0.00910966736202029));
#15151=CARTESIAN_POINT('Ctrl Pts',(-0.000337090369108963,-0.0271224559520518,
-0.00908065876845681));
#15152=CARTESIAN_POINT('Ctrl Pts',(-0.000860189467237764,-0.027152024494513,
-0.00918030222031895));
#15153=CARTESIAN_POINT('Ctrl Pts',(-0.00132619774419796,-0.0271787743898752,
-0.00940320080323842));
#15154=CARTESIAN_POINT('',(-0.00290082504980717,-0.0271763869731017,-0.0131997112254818));
#15155=CARTESIAN_POINT('Origin',(0.,-0.0271787743898824,-0.0121758532865681));
#15156=CARTESIAN_POINT('',(0.0030735,-0.0266247798641645,-0.0121758532205251));
#15157=CARTESIAN_POINT('Ctrl Pts',(-0.00289961087048566,-0.0271763232091976,
-0.0131992324493061));
#15158=CARTESIAN_POINT('Ctrl Pts',(-0.00308763169612782,-0.0271471980364023,
-0.0126662862034661));
#15159=CARTESIAN_POINT('Ctrl Pts',(-0.00312155308971536,-0.0271224964632597,
-0.0120796370457119));
#15160=CARTESIAN_POINT('Ctrl Pts',(-0.00300304924290092,-0.0270927645607504,
-0.011527470947428));
#15161=CARTESIAN_POINT('Ctrl Pts',(-0.00293451349166028,-0.0270755693529233,
-0.0112081301043012));
#15162=CARTESIAN_POINT('Ctrl Pts',(-0.00281529683471947,-0.0270568702133368,
-0.0109001188883222));
#15163=CARTESIAN_POINT('Ctrl Pts',(-0.00265107719335906,-0.0270388739894333,
-0.0106192115375074));
#15164=CARTESIAN_POINT('Ctrl Pts',(-0.00259301567986319,-0.0270325112426364,
-0.0105198939053088));
#15165=CARTESIAN_POINT('Ctrl Pts',(-0.0025295230107784,-0.0270264147659866,
-0.0104236706696188));
#15166=CARTESIAN_POINT('Ctrl Pts',(-0.00246051730748276,-0.0270204974975181,
-0.0103314076212616));
#15167=CARTESIAN_POINT('Ctrl Pts',(-0.00219969424658502,-0.0269981318088809,
-0.0099826780303586));
#15168=CARTESIAN_POINT('Ctrl Pts',(-0.00185877014511459,-0.0269783263552642,
-0.00969034090217038));
#15169=CARTESIAN_POINT('Ctrl Pts',(-0.00147503608472361,-0.02695637990696,
-0.00948099890407491));
#15170=CARTESIAN_POINT('Ctrl Pts',(-0.00117664367801609,-0.0269393143029282,
-0.00931821412918935));
#15171=CARTESIAN_POINT('Ctrl Pts',(-0.000851985381520887,-0.0269210215646513,
-0.00920449927642397));
#15172=CARTESIAN_POINT('Ctrl Pts',(-0.000518818664669812,-0.0269020068478604,
-0.00914659649850862));
#15173=CARTESIAN_POINT('Ctrl Pts',(-0.000275393555156683,-0.026888113924939,
-0.00910429038165403));
#15174=CARTESIAN_POINT('Ctrl Pts',(-2.59212939084465E-5,-0.0268748219903249,
-0.00908976765259022));
#15175=CARTESIAN_POINT('Ctrl Pts',(0.000221735837015603,-0.0268620018707547,
-0.00910749573534982));
#15176=CARTESIAN_POINT('Ctrl Pts',(0.000525307879835055,-0.0268462872823129,
-0.00912922638481073));
#15177=CARTESIAN_POINT('Ctrl Pts',(0.000826058247928513,-0.0268312816080388,
-0.00919954037695764));
#15178=CARTESIAN_POINT('Ctrl Pts',(0.00110976365222905,-0.0268167469419083,
-0.00931015671458052));
#15179=CARTESIAN_POINT('Ctrl Pts',(0.0014265401172301,-0.0268005179942499,
-0.00943366741219987));
#15180=CARTESIAN_POINT('Ctrl Pts',(0.00172191944737471,-0.0267832082732035,
-0.00960988343338538));
#15181=CARTESIAN_POINT('Ctrl Pts',(0.00198065347741659,-0.0267648525352007,
-0.00982725230390036));
#15182=CARTESIAN_POINT('Ctrl Pts',(0.00227095652361926,-0.0267442571513749,
-0.0100711430872269));
#15183=CARTESIAN_POINT('Ctrl Pts',(0.0025193142480031,-0.0267226761994269,
-0.0103697063505273));
#15184=CARTESIAN_POINT('Ctrl Pts',(0.00270111735108537,-0.0267025569396926,
-0.0107044215657649));
#15185=CARTESIAN_POINT('Ctrl Pts',(0.0027889247782419,-0.0266928397214294,
-0.01086608262315));
#15186=CARTESIAN_POINT('Ctrl Pts',(0.00286131189634785,-0.0266834634729189,
-0.0110361616317958));
#15187=CARTESIAN_POINT('Ctrl Pts',(0.0029187151677258,-0.0266747039152927,
-0.0112112645346353));
#15188=CARTESIAN_POINT('Ctrl Pts',(0.00302065102293573,-0.0266591488262456,
-0.0115222096031344));
#15189=CARTESIAN_POINT('Ctrl Pts',(0.00307230929529488,-0.0266437720605787,
-0.0118493837213127));
#15190=CARTESIAN_POINT('Ctrl Pts',(0.00307224986630574,-0.0266269429077654,
-0.0121759396378161));
#15191=CARTESIAN_POINT('',(0.00307349935664723,-0.0256248537561334,-0.0121772619237424));
#15192=CARTESIAN_POINT('Ctrl Pts',(0.0030735,-0.0266247798641645,-0.0121758532205251));
#15193=CARTESIAN_POINT('Ctrl Pts',(0.00307350001218174,-0.0265954233398465,
-0.0127428512174199));
#15194=CARTESIAN_POINT('Ctrl Pts',(0.00291229937933948,-0.0265660668155286,
-0.0133099880167539));
#15195=CARTESIAN_POINT('Ctrl Pts',(0.00261419079830434,-0.0265367102912106,
-0.0137921480369242));
#15196=CARTESIAN_POINT('Ctrl Pts',(0.00248924640825892,-0.0265244062742915,
-0.0139942327585893));
#15197=CARTESIAN_POINT('Ctrl Pts',(0.00234087672716486,-0.0265121022573725,
-0.0141815619079462));
#15198=CARTESIAN_POINT('Ctrl Pts',(0.00217329292152179,-0.0264997982404535,
-0.01434914574899));
#15199=CARTESIAN_POINT('Ctrl Pts',(0.00178081767495824,-0.0264709826752771,
-0.0147416210784607));
#15200=CARTESIAN_POINT('Ctrl Pts',(0.00127739859003859,-0.0264421671101007,
-0.0150262717538645));
#15201=CARTESIAN_POINT('Ctrl Pts',(0.000736650025021551,-0.0264133515449242,
-0.0151597683306965));
#15202=CARTESIAN_POINT('Ctrl Pts',(0.000495602930727057,-0.0264005065579828,
-0.0152192765088507));
#15203=CARTESIAN_POINT('Ctrl Pts',(0.000247526363821311,-0.0263876615710414,
-0.0152493532903629));
#15204=CARTESIAN_POINT('Ctrl Pts',(-4.72438689886815E-11,-0.0263748165841,
-0.0152493532865581));
#15205=CARTESIAN_POINT('Ctrl Pts',(-0.000557337869483213,-0.0263458944298224,
-0.0152493532779911));
#15206=CARTESIAN_POINT('Ctrl Pts',(-0.00111652614259104,-0.0263169722755447,
-0.0150934215947984));
#15207=CARTESIAN_POINT('Ctrl Pts',(-0.00159439172129221,-0.0262880501212671,
-0.0148034600472959));
#15208=CARTESIAN_POINT('Ctrl Pts',(-0.00180486158453935,-0.0262753117234269,
-0.0146757501431516));
#15209=CARTESIAN_POINT('Ctrl Pts',(-0.00199971203677584,-0.0262625733255867,
-0.0145227266810762));
#15210=CARTESIAN_POINT('Ctrl Pts',(-0.00217329298833469,-0.0262498349277465,
-0.0143491456821771));
#15211=CARTESIAN_POINT('Ctrl Pts',(-0.00256732938986629,-0.0262209182038713,
-0.0139551091731811));
#15212=CARTESIAN_POINT('Ctrl Pts',(-0.0028524424777176,-0.0261920014799961,
-0.0134495414786068));
#15213=CARTESIAN_POINT('Ctrl Pts',(-0.00298533501378733,-0.0261630847561209,
-0.0129067274928723));
#15214=CARTESIAN_POINT('Ctrl Pts',(-0.00304390180239396,-0.0261503409278783,
-0.0126675050888499));
#15215=CARTESIAN_POINT('Ctrl Pts',(-0.00307350006319907,-0.0261375970996357,
-0.0124214237788402));
#15216=CARTESIAN_POINT('Ctrl Pts',(-0.0030734999999999,-0.0261248532713931,
-0.0121758524955754));
#15217=CARTESIAN_POINT('Ctrl Pts',(-0.00307349985659614,-0.0260959365475179,
-0.0116186324158105));
#15218=CARTESIAN_POINT('Ctrl Pts',(-0.00291763174738019,-0.0260670198236426,
-0.0110595431121297));
#15219=CARTESIAN_POINT('Ctrl Pts',(-0.00262777159708766,-0.0260381030997674,
-0.0105817332523262));
#15220=CARTESIAN_POINT('Ctrl Pts',(-0.00250002794308169,-0.0260253592715248,
-0.0103711586792096));
#15221=CARTESIAN_POINT('Ctrl Pts',(-0.0023469469085358,-0.0260126154432822,
-0.0101762146797365));
#15222=CARTESIAN_POINT('Ctrl Pts',(-0.00217329186971606,-0.0259998716150396,
-0.0100025597723208));
#15223=CARTESIAN_POINT('Ctrl Pts',(-0.00177918126745261,-0.025970949460762,
-0.00960844946827901));
#15224=CARTESIAN_POINT('Ctrl Pts',(-0.00127350533089006,-0.0259420273064843,
-0.00932330853013815));
#15225=CARTESIAN_POINT('Ctrl Pts',(-0.000730575770667611,-0.0259131051522067,
-0.00919044522511768));
#15226=CARTESIAN_POINT('Ctrl Pts',(-0.000491449297897936,-0.0259003667543665,
-0.00913192725921977));
#15227=CARTESIAN_POINT('Ctrl Pts',(-0.000245470875214288,-0.0258876283565263,
-0.00910235316398429));
#15228=CARTESIAN_POINT('Ctrl Pts',(1.53472154182256E-9,-0.0258748899586861,
-0.00910235328655848));
#15229=CARTESIAN_POINT('Ctrl Pts',(0.000555285355831455,-0.0258460743935097,
-0.00910235356383391));
#15230=CARTESIAN_POINT('Ctrl Pts',(0.00111258429007166,-0.0258172588283333,
-0.00925717441826294));
#15231=CARTESIAN_POINT('Ctrl Pts',(0.00158924789974853,-0.0257884432631569,
-0.00954513221370661));
#15232=CARTESIAN_POINT('Ctrl Pts',(0.00180172812716241,-0.0257755982762155,
-0.0096734938855845));
#15233=CARTESIAN_POINT('Ctrl Pts',(0.00199834217675505,-0.0257627532892741,
-0.00982760986230361));
#15234=CARTESIAN_POINT('Ctrl Pts',(0.00217329404013981,-0.0257499083023327,
-0.010002561942745));
#15235=CARTESIAN_POINT('Ctrl Pts',(0.00257313709327206,-0.0257205517770763,
-0.0104024054919486));
#15236=CARTESIAN_POINT('Ctrl Pts',(0.00286056100861589,-0.02569119525182,
-0.0109166263961833));
#15237=CARTESIAN_POINT('Ctrl Pts',(0.00299109311605828,-0.0256618387265637,
-0.011468913245912));
#15238=CARTESIAN_POINT('Ctrl Pts',(0.00304580226648514,-0.0256495346997022,
-0.0117003899678665));
#15239=CARTESIAN_POINT('Ctrl Pts',(0.00307350017616934,-0.0256372306728407,
-0.0119382130388463));
#15240=CARTESIAN_POINT('Ctrl Pts',(0.00307349999999916,-0.0256249266459792,
-0.0121758555650184));
#15241=CARTESIAN_POINT('',(0.00307349987269237,-0.024624748008777,-0.0121752386980468));
#15242=CARTESIAN_POINT('Ctrl Pts',(0.00307349871570724,-0.0256247811395518,
-0.0121786630100232));
#15243=CARTESIAN_POINT('Ctrl Pts',(0.00307298037501563,-0.0255954138959754,
-0.0127456652327553));
#15244=CARTESIAN_POINT('Ctrl Pts',(0.00291125891857178,-0.0255660466523991,
-0.0133126581730836));
#15245=CARTESIAN_POINT('Ctrl Pts',(0.00261270561721589,-0.0255366794088227,
-0.0137945477011307));
#15246=CARTESIAN_POINT('Ctrl Pts',(0.00248766720975212,-0.0255243799857324,
-0.0139963699515859));
#15247=CARTESIAN_POINT('Ctrl Pts',(0.00233925141307591,-0.0255120805626421,
-0.0141834369067124));
#15248=CARTESIAN_POINT('Ctrl Pts',(0.00217166421594283,-0.0254997811395518,
-0.0143507732352444));
#15249=CARTESIAN_POINT('Ctrl Pts',(0.00177888813102166,-0.025470954837001,
-0.0147429613564746));
#15250=CARTESIAN_POINT('Ctrl Pts',(0.00127524673881237,-0.0254421285344501,
-0.0150272366276994));
#15251=CARTESIAN_POINT('Ctrl Pts',(0.000734389712799084,-0.0254133022318993,
-0.0151603254341472));
#15252=CARTESIAN_POINT('Ctrl Pts',(0.000493470811168384,-0.0254004618677835,
-0.0152196084008585));
#15253=CARTESIAN_POINT('Ctrl Pts',(0.000245554842806924,-0.0253876215036676,
-0.015249497186873));
#15254=CARTESIAN_POINT('Ctrl Pts',(-1.79457787336804E-6,-0.0253747811395518,
-0.0152493527626424));
#15255=CARTESIAN_POINT('Ctrl Pts',(-0.000559141493980125,-0.0253458482343444,
-0.0152490273347543));
#15256=CARTESIAN_POINT('Ctrl Pts',(-0.00111824595371007,-0.025316915329137,
-0.0150927642575334));
#15257=CARTESIAN_POINT('Ctrl Pts',(-0.00159594612820109,-0.0252879824239296,
-0.0148025162276071));
#15258=CARTESIAN_POINT('Ctrl Pts',(-0.00180618841211308,-0.0252752486624703,
-0.0146747741584783));
#15259=CARTESIAN_POINT('Ctrl Pts',(-0.00200081903578972,-0.0252625149010111,
-0.0145217645205726));
#15260=CARTESIAN_POINT('Ctrl Pts',(-0.00217420255139949,-0.0252497811395518,
-0.0143482357380357));
#15261=CARTESIAN_POINT('Ctrl Pts',(-0.00256808028828137,-0.0252208536770538,
-0.013954027996261));
#15262=CARTESIAN_POINT('Ctrl Pts',(-0.00285298337185679,-0.0251919262145559,
-0.013448332571431));
#15263=CARTESIAN_POINT('Ctrl Pts',(-0.00298564623897108,-0.0251629987520579,
-0.0129054550859788));
#15264=CARTESIAN_POINT('Ctrl Pts',(-0.00304406890047807,-0.0251502595478892,
-0.0126663802923892));
#15265=CARTESIAN_POINT('Ctrl Pts',(-0.00307356213274085,-0.0251375203437205,
-0.0124204688459204));
#15266=CARTESIAN_POINT('Ctrl Pts',(-0.00307349990116896,-0.0251247811395518,
-0.0121750738544722));
#15267=CARTESIAN_POINT('Ctrl Pts',(-0.00307335858924413,-0.0250958536770538,
-0.0116178448220857));
#15268=CARTESIAN_POINT('Ctrl Pts',(-0.0029173440407025,-0.0250669262145559,
-0.0110587878836229));
#15269=CARTESIAN_POINT('Ctrl Pts',(-0.00262735552814881,-0.0250379987520579,
-0.0105810475997405));
#15270=CARTESIAN_POINT('Ctrl Pts',(-0.00249964910148719,-0.0250252595478892,
-0.0103706582157277));
#15271=CARTESIAN_POINT('Ctrl Pts',(-0.00234664610208603,-0.0250125203437205,
-0.0101758833232711));
#15272=CARTESIAN_POINT('Ctrl Pts',(-0.00217310045002427,-0.0249997811395518,
-0.0100023683696322));
#15273=CARTESIAN_POINT('Ctrl Pts',(-0.00177894867776568,-0.0249708482343444,
-0.00960828631872732));
#15274=CARTESIAN_POINT('Ctrl Pts',(-0.00127323899679475,-0.024941915329137,
-0.00932318820737745));
#15275=CARTESIAN_POINT('Ctrl Pts',(-0.000730289593933061,-0.0249129824239296,
-0.00919037520775847));
#15276=CARTESIAN_POINT('Ctrl Pts',(-0.000491330245367016,-0.0249002486624703,
-0.00913192241694081));
#15277=CARTESIAN_POINT('Ctrl Pts',(-0.000245531643034035,-0.0248875149010111,
-0.00910237210790608));
#15278=CARTESIAN_POINT('Ctrl Pts',(-2.35713786740483E-7,-0.0248747811395518,
-0.00910235329559681));
#15279=CARTESIAN_POINT('Ctrl Pts',(0.000555057762818296,-0.024845954837001,
-0.00910231070886231));
#15280=CARTESIAN_POINT('Ctrl Pts',(0.00111237636565889,-0.0248171285344501,
-0.00925709369733194));
#15281=CARTESIAN_POINT('Ctrl Pts',(0.00158906643107183,-0.0247883022318993,
-0.00954502259500065));
#15282=CARTESIAN_POINT('Ctrl Pts',(0.00180140285540206,-0.0247754618677835,
-0.00967327740253341));
#15283=CARTESIAN_POINT('Ctrl Pts',(0.00199789782178222,-0.0247626215036676,
-0.00982725041082163));
#15284=CARTESIAN_POINT('Ctrl Pts',(0.00217276704534377,-0.0247497811395518,
-0.0100020350750537));
#15285=CARTESIAN_POINT('Ctrl Pts',(0.00257271108400271,-0.0247204138959755,
-0.010401785717762));
#15286=CARTESIAN_POINT('Ctrl Pts',(0.00286026047587044,-0.0246910466523991,
-0.0109159421159849));
#15287=CARTESIAN_POINT('Ctrl Pts',(0.00299092486810477,-0.0246616794088228,
-0.0114682017597792));
#15288=CARTESIAN_POINT('Ctrl Pts',(0.00304564899087614,-0.0246493799857324,
-0.0116994960246657));
#15289=CARTESIAN_POINT('Ctrl Pts',(0.0030734030999119,-0.0246370805626421,
-0.0119371336788303));
#15290=CARTESIAN_POINT('Ctrl Pts',(0.00307349974546122,-0.0246247811395518,
-0.0121746024269245));
#15291=CARTESIAN_POINT('Ctrl Pts',(0.00307349999992352,-0.0246247148780022,
-0.0121758749691691));
#15292=CARTESIAN_POINT('Ctrl Pts',(0.00307349599990712,-0.024595352466092,
-0.0127428754284441));
#15293=CARTESIAN_POINT('Ctrl Pts',(0.00291229002300707,-0.0245659900541818,
-0.0133100131564192));
#15294=CARTESIAN_POINT('Ctrl Pts',(0.00261417579362664,-0.0245366276422716,
-0.0137921723051978));
#15295=CARTESIAN_POINT('Ctrl Pts',(0.00248927970630659,-0.024524326148413,
-0.0139941747096894));
#15296=CARTESIAN_POINT('Ctrl Pts',(0.0023409773439075,-0.0245120246545545,
-0.0141814332731449));
#15297=CARTESIAN_POINT('Ctrl Pts',(0.00217347456253716,-0.0244997231606959,
-0.0143489640927537));
#15298=CARTESIAN_POINT('Ctrl Pts',(0.00178102831398537,-0.0244709016982887,
-0.0147414760327609));
#15299=CARTESIAN_POINT('Ctrl Pts',(0.00127762796176171,-0.0244420802358815,
-0.0150261697812338));
#15300=CARTESIAN_POINT('Ctrl Pts',(0.000736885823996938,-0.0244132587734743,
-0.0151597101082559));
#15301=CARTESIAN_POINT('Ctrl Pts',(0.000495938637509918,-0.0244004163301127,
-0.0152192138233012));
#15302=CARTESIAN_POINT('Ctrl Pts',(0.000247965232569662,-0.0243875738867512,
-0.0152493100806458));
#15303=CARTESIAN_POINT('Ctrl Pts',(5.36111760505852E-7,-0.0243747314433896,
-0.015249353239801));
#15304=CARTESIAN_POINT('Ctrl Pts',(-0.000556806754329106,-0.0243458033844476,
-0.0152494504573282));
#15305=CARTESIAN_POINT('Ctrl Pts',(-0.00111602625065947,-0.0243168753255056,
-0.015093613618999));
#15306=CARTESIAN_POINT('Ctrl Pts',(-0.00159394459477676,-0.0242879472665637,
-0.0148037313048044));
#15307=CARTESIAN_POINT('Ctrl Pts',(-0.00180435258788129,-0.0242752114197369,
-0.0146761079216115));
#15308=CARTESIAN_POINT('Ctrl Pts',(-0.0019991579586532,-0.0242624755729101,
-0.0145231885374881));
#15309=CARTESIAN_POINT('Ctrl Pts',(-0.00217271631721875,-0.0242497397260833,
-0.0143497222004743));
#15310=CARTESIAN_POINT('Ctrl Pts',(-0.0025668607214936,-0.0242208171043095,
-0.0139557867736294));
#15311=CARTESIAN_POINT('Ctrl Pts',(-0.0028521088439021,-0.0241918944825356,
-0.0134502901086501));
#15312=CARTESIAN_POINT('Ctrl Pts',(-0.00298514405465798,-0.0241629718607618,
-0.012907507045477));
#15313=CARTESIAN_POINT('Ctrl Pts',(-0.00304375006260632,-0.0241502305767668,
-0.0126683947959168));
#15314=CARTESIAN_POINT('Ctrl Pts',(-0.00307341243721463,-0.0241374892927719,
-0.0124224215391223));
#15315=CARTESIAN_POINT('Ctrl Pts',(-0.00307349980533095,-0.024124748008777,
-0.0121769471926725));
#15316=CARTESIAN_POINT('Ctrl Pts',(-0.00307369813031801,-0.0240958253870032,
-0.0116197222159447));
#15317=CARTESIAN_POINT('Ctrl Pts',(-0.00291802652412777,-0.0240669027652293,
-0.011060573504202));
#15318=CARTESIAN_POINT('Ctrl Pts',(-0.00262833255001533,-0.0240379801434555,
-0.010582658302719));
#15319=CARTESIAN_POINT('Ctrl Pts',(-0.00250071364932767,-0.0240252388594605,
-0.0103721222954651));
#15320=CARTESIAN_POINT('Ctrl Pts',(-0.002347772072134,-0.0240124975754656,
-0.010177195475843));
#15321=CARTESIAN_POINT('Ctrl Pts',(-0.00217426319369506,-0.0239997562914707,
-0.0100035315298786));
#15322=CARTESIAN_POINT('Ctrl Pts',(-0.00178032526213027,-0.0239708282325287,
-0.00960924152998886));
#15323=CARTESIAN_POINT('Ctrl Pts',(-0.00127477209842849,-0.0239419001735867,
-0.00932387362135798));
#15324=CARTESIAN_POINT('Ctrl Pts',(-0.000731897509323036,-0.0239129721146448,
-0.00919076898526161));
#15325=CARTESIAN_POINT('Ctrl Pts',(-0.000492891925613767,-0.023900236267818,
-0.00913216843205273));
#15326=CARTESIAN_POINT('Ctrl Pts',(-0.000247027045862867,-0.0238875004209912,
-0.00910248559522246));
#15327=CARTESIAN_POINT('Ctrl Pts',(-1.65170043229059E-6,-0.0238747645741644,
-0.00910235373037045));
#15328=CARTESIAN_POINT('Ctrl Pts',(0.000553637350242043,-0.0238459431117572,
-0.00910205531771469));
#15329=CARTESIAN_POINT('Ctrl Pts',(0.00111102372754518,-0.02381712164935,
-0.00925657921020503));
#15330=CARTESIAN_POINT('Ctrl Pts',(0.00158784448799195,-0.0237883001869428,
-0.00954428490782393));
#15331=CARTESIAN_POINT('Ctrl Pts',(0.00180030919651852,-0.0237754577435812,
-0.00967248257088029));
#15332=CARTESIAN_POINT('Ctrl Pts',(0.00199693407333457,-0.0237626153002197,
-0.00982642253680694));
#15333=CARTESIAN_POINT('Ctrl Pts',(0.00217192712459075,-0.0237497728568581,
-0.0100011958846975));
#15334=CARTESIAN_POINT('Ctrl Pts',(0.00257202373453882,-0.0237204104449479,
-0.0104007901742898));
#15335=CARTESIAN_POINT('Ctrl Pts',(0.00285977136180032,-0.0236910480330377,
-0.0109148331126464));
#15336=CARTESIAN_POINT('Ctrl Pts',(0.00299064981277481,-0.0236616856211274,
-0.0114670402312678));
#15337=CARTESIAN_POINT('Ctrl Pts',(0.00304548183630884,-0.0236493841272689,
-0.0116983894984578));
#15338=CARTESIAN_POINT('Ctrl Pts',(0.00307332843671528,-0.0236370826334104,
-0.0119360968598615));
#15339=CARTESIAN_POINT('Ctrl Pts',(0.00307349920581301,-0.0236247811395518,
-0.0121736437918623));
#15340=CARTESIAN_POINT('Origin',(0.,-0.0271787743898721,-0.0121758532865581));
#15341=CARTESIAN_POINT('',(0.00251751029526666,-0.0221787894580564,-0.01217507662023));
#15342=CARTESIAN_POINT('',(0.00251749942082674,-0.0211788370573946,-0.0121771378810096));
#15343=CARTESIAN_POINT('Ctrl Pts',(0.0025174999999979,-0.0221787227179838,
-0.0121758500317772));
#15344=CARTESIAN_POINT('Ctrl Pts',(0.0025175006270217,-0.0221481735656116,
-0.0126608388780163));
#15345=CARTESIAN_POINT('Ctrl Pts',(0.00237306104723493,-0.0221176054100055,
-0.0131460858681194));
#15346=CARTESIAN_POINT('Ctrl Pts',(0.00210809405127732,-0.0220870179095754,
-0.0135519876262827));
#15347=CARTESIAN_POINT('Ctrl Pts',(0.00201298331277554,-0.0220760384298695,
-0.013697687341972));
#15348=CARTESIAN_POINT('Ctrl Pts',(0.00190281903971488,-0.0220650564576341,
-0.0138333157348486));
#15349=CARTESIAN_POINT('Ctrl Pts',(0.00178014970375261,-0.0220540719770704,
-0.0139559862260403));
#15350=CARTESIAN_POINT('Ctrl Pts',(0.00144068346397155,-0.0220236743207722,
-0.0142954556627196));
#15351=CARTESIAN_POINT('Ctrl Pts',(0.000999662972082794,-0.0219932574554404,
-0.0145361579274445));
#15352=CARTESIAN_POINT('Ctrl Pts',(0.000528152341818232,-0.0219628223855097,
-0.0146373287290177));
#15353=CARTESIAN_POINT('Ctrl Pts',(0.000354602569433263,-0.0219516200941509,
-0.0146745668493443));
#15354=CARTESIAN_POINT('Ctrl Pts',(0.000177184431567649,-0.0219404153364902,
-0.014693352730372));
#15355=CARTESIAN_POINT('Ctrl Pts',(7.90266785490307E-9,-0.021929208162614,
-0.0146933532865457));
#15356=CARTESIAN_POINT('Ctrl Pts',(-0.000329262373811186,-0.0219083804081497,
-0.0146933543201559));
#15357=CARTESIAN_POINT('Ctrl Pts',(-0.0006588475998666,-0.0218875443086468,
-0.0146278711993561));
#15358=CARTESIAN_POINT('Ctrl Pts',(-0.000963400065171092,-0.0218666966492722,
-0.0145017222778017));
#15359=CARTESIAN_POINT('Ctrl Pts',(-0.00126795253047558,-0.0218458489898976,
-0.0143755733562472));
#15360=CARTESIAN_POINT('Ctrl Pts',(-0.00154720597461104,-0.0218249897706513,
-0.0141889292240289));
#15361=CARTESIAN_POINT('Ctrl Pts',(-0.00178013852765,-0.021804132065188,
-0.013955997402178));
#15362=CARTESIAN_POINT('Ctrl Pts',(-0.00189660480416948,-0.0217937032124563,
-0.0138395314912525));
#15363=CARTESIAN_POINT('Ctrl Pts',(-0.00200161407899827,-0.0217832747381703,
-0.0137116060554127));
#15364=CARTESIAN_POINT('Ctrl Pts',(-0.00209322310255972,-0.0217728298716174,
-0.0135745038122114));
#15365=CARTESIAN_POINT('Ctrl Pts',(-0.00218483212612116,-0.0217623850050645,
-0.0134374015690101));
#15366=CARTESIAN_POINT('Ctrl Pts',(-0.00226298661049305,-0.0217519237462447,
-0.0132910645112378));
#15367=CARTESIAN_POINT('Ctrl Pts',(-0.00232586596705365,-0.0217415144103612,
-0.0131392606527857));
#15368=CARTESIAN_POINT('Ctrl Pts',(-0.00238874532361424,-0.0217311050744777,
-0.0129874567943336));
#15369=CARTESIAN_POINT('Ctrl Pts',(-0.00243663034191228,-0.0217207476615306,
-0.0128303642853091));
#15370=CARTESIAN_POINT('Ctrl Pts',(-0.00246912675070183,-0.0217101856814195,
-0.0126669941410679));
#15371=CARTESIAN_POINT('Ctrl Pts',(-0.0024853749550966,-0.021704904691364,
-0.0125853090689473));
#15372=CARTESIAN_POINT('Ctrl Pts',(-0.00249755937086223,-0.0216995725595175,
-0.0125019905764725));
#15373=CARTESIAN_POINT('Ctrl Pts',(-0.00250537750098589,-0.0216945163415666,
-0.0124226119288662));
#15374=CARTESIAN_POINT('Ctrl Pts',(-0.00250928656604771,-0.0216919882325911,
-0.012382922605063));
#15375=CARTESIAN_POINT('Ctrl Pts',(-0.00251226369782038,-0.0216895291020895,
-0.0123442417324174));
#15376=CARTESIAN_POINT('Ctrl Pts',(-0.00251446754887909,-0.0216866804277945,
-0.0122993814033331));
#15377=CARTESIAN_POINT('Ctrl Pts',(-0.0025166713999378,-0.0216838317534995,
-0.0122545210742488));
#15378=CARTESIAN_POINT('Ctrl Pts',(-0.0025175,-0.0216805935354111,-0.0122034465123688));
#15379=CARTESIAN_POINT('Ctrl Pts',(-0.0025175,-0.0216788436847921,-0.012175853286558));
#15380=CARTESIAN_POINT('Ctrl Pts',(-0.0025175,-0.0216770938341731,-0.0121482600607472));
#15381=CARTESIAN_POINT('Ctrl Pts',(-0.00251732341511713,-0.0216768323510236,
-0.0121441379809924));
#15382=CARTESIAN_POINT('Ctrl Pts',(-0.00251714088833399,-0.0216761473547436,
-0.012133332723566));
#15383=CARTESIAN_POINT('Ctrl Pts',(-0.00251695836155086,-0.0216754623584636,
-0.0121225274661396));
#15384=CARTESIAN_POINT('Ctrl Pts',(-0.00251656012884372,-0.0216743538490531,
-0.0121050456834368));
#15385=CARTESIAN_POINT('Ctrl Pts',(-0.00251597543186803,-0.021673288642944,
-0.0120882526231104));
#15386=CARTESIAN_POINT('Ctrl Pts',(-0.00251480603791666,-0.0216711582307259,
-0.0120546665024575));
#15387=CARTESIAN_POINT('Ctrl Pts',(-0.00251312737169555,-0.0216692010317134,
-0.0120238206193739));
#15388=CARTESIAN_POINT('Ctrl Pts',(-0.00251066671451669,-0.0216670840740922,
-0.0119904917516649));
#15389=CARTESIAN_POINT('Ctrl Pts',(-0.00250574540015897,-0.0216628501588498,
-0.0119238340162468));
#15390=CARTESIAN_POINT('Ctrl Pts',(-0.0024973438866829,-0.0216579772091725,
-0.0118472847469798));
#15391=CARTESIAN_POINT('Ctrl Pts',(-0.00248382492313489,-0.0216527263553775,
-0.01176546322672));
#15392=CARTESIAN_POINT('Ctrl Pts',(-0.00247030595958689,-0.0216474755015825,
-0.0116836417064601));
#15393=CARTESIAN_POINT('Ctrl Pts',(-0.00245181307897284,-0.0216418467436696,
-0.0115965131745003));
#15394=CARTESIAN_POINT('Ctrl Pts',(-0.00242619291886598,-0.0216357705286481,
-0.0115039945436332));
#15395=CARTESIAN_POINT('Ctrl Pts',(-0.00240057275875913,-0.0216296943136265,
-0.0114114759127662));
#15396=CARTESIAN_POINT('Ctrl Pts',(-0.00236778366178648,-0.0216231706414963,
-0.0113135845938267));
#15397=CARTESIAN_POINT('Ctrl Pts',(-0.0023256664652384,-0.0216162165939039,
-0.0112119644223909));
#15398=CARTESIAN_POINT('Ctrl Pts',(-0.00224143207214223,-0.0216023084987191,
-0.0110087240795193));
#15399=CARTESIAN_POINT('Ctrl Pts',(-0.00211996024600938,-0.0215866789016856,
-0.0107905612374037));
#15400=CARTESIAN_POINT('Ctrl Pts',(-0.00194563811812038,-0.0215693144003712,
-0.0105782617983118));
#15401=CARTESIAN_POINT('Ctrl Pts',(-0.00177131599023139,-0.0215519498990567,
-0.0103659623592199));
#15402=CARTESIAN_POINT('Ctrl Pts',(-0.00154366358191858,-0.0215328504934613,
-0.0101600234254014));
#15403=CARTESIAN_POINT('Ctrl Pts',(-0.00125814306546542,-0.0215120197747794,
-0.00999528403133567));
#15404=CARTESIAN_POINT('Ctrl Pts',(-0.000972622549012248,-0.0214911890560976,
-0.00983054463726996));
#15405=CARTESIAN_POINT('Ctrl Pts',(-0.000628743563775202,-0.0214686270243295,
-0.00970799681970146));
#15406=CARTESIAN_POINT('Ctrl Pts',(-0.000246101333787693,-0.0214443327171287,
-0.00967041113326301));
#15407=CARTESIAN_POINT('Ctrl Pts',(0.000136540896199817,-0.0214200384099279,
-0.00963282544682456));
#15408=CARTESIAN_POINT('Ctrl Pts',(0.000557976207619178,-0.0213940118272944,
-0.00968195163694664));
#15409=CARTESIAN_POINT('Ctrl Pts',(0.000963897772287331,-0.0213662532274188,
-0.00985019051337289));
#15410=CARTESIAN_POINT('Ctrl Pts',(0.00136981933695548,-0.0213384946275433,
-0.0100184293897991));
#15411=CARTESIAN_POINT('Ctrl Pts',(0.00175889506188566,-0.0213090040104255,
-0.0103082271150057));
#15412=CARTESIAN_POINT('Ctrl Pts',(0.00204652746439145,-0.02127778130565,
-0.010709725192737));
#15413=CARTESIAN_POINT('Ctrl Pts',(0.00229998122120466,-0.0212502687175191,
-0.0110635142487257));
#15414=CARTESIAN_POINT('Ctrl Pts',(0.00247306168481993,-0.0212214112240566,
-0.0115047157964407));
#15415=CARTESIAN_POINT('Ctrl Pts',(0.00250998397883032,-0.0211912088413219,
-0.0119814653342176));
#15416=CARTESIAN_POINT('Ctrl Pts',(0.00251496274895857,-0.021187136214607,
-0.012045752411198));
#15417=CARTESIAN_POINT('Ctrl Pts',(0.00251750023443854,-0.0211830391336996,
-0.012110615346057));
#15418=CARTESIAN_POINT('Ctrl Pts',(0.00251749999998375,-0.0211789175986389,
-0.0121758623327987));
#15419=CARTESIAN_POINT('',(0.00251749999999825,-0.02017876552198,-0.0121758562566413));
#15420=CARTESIAN_POINT('Ctrl Pts',(0.00251749897019639,-0.0211787743898821,
-0.0121781303592641));
#15421=CARTESIAN_POINT('Ctrl Pts',(0.00251705740623119,-0.0211479067710791,
-0.0126663171548534));
#15422=CARTESIAN_POINT('Ctrl Pts',(0.0023703289589053,-0.0211170391522761,
-0.0131543526657776));
#15423=CARTESIAN_POINT('Ctrl Pts',(0.00210170356769341,-0.0210861715334731,
-0.0135617278709072));
#15424=CARTESIAN_POINT('Ctrl Pts',(0.00200772487514791,-0.0210753724856095,
-0.0137042482372092));
#15425=CARTESIAN_POINT('Ctrl Pts',(0.00189928032167646,-0.0210645734377458,
-0.0138370435243574));
#15426=CARTESIAN_POINT('Ctrl Pts',(0.00177874396527104,-0.0210537743898821,
-0.0139573908685394));
#15427=CARTESIAN_POINT('Ctrl Pts',(0.00144055410491447,-0.0210234754112344,
-0.0142950504157245));
#15428=CARTESIAN_POINT('Ctrl Pts',(0.00100184213234116,-0.0209931764325866,
-0.0145346681905484));
#15429=CARTESIAN_POINT('Ctrl Pts',(0.000533254187855318,-0.0209628774539389,
-0.0146362285061404));
#15430=CARTESIAN_POINT('Ctrl Pts',(0.000357447550137102,-0.02095150976592,
-0.0146743322982246));
#15431=CARTESIAN_POINT('Ctrl Pts',(0.000177703303467145,-0.020940142077901,
-0.0146934719846099));
#15432=CARTESIAN_POINT('Ctrl Pts',(-1.67369790539226E-6,-0.0209287743898821,
-0.0146933527301996));
#15433=CARTESIAN_POINT('Ctrl Pts',(-0.000481546144216977,-0.0208983633549288,
-0.0146930336987455));
#15434=CARTESIAN_POINT('Ctrl Pts',(-0.000962865230832859,-0.0208679523199756,
-0.0145511889640779));
#15435=CARTESIAN_POINT('Ctrl Pts',(-0.00136692716455534,-0.0208375412850222,
-0.0142899290602239));
#15436=CARTESIAN_POINT('Ctrl Pts',(-0.00151647723157411,-0.0208262856533089,
-0.0141932324083747));
#15437=CARTESIAN_POINT('Ctrl Pts',(-0.00165558709770307,-0.0208150300215955,
-0.0140806851966216));
#15438=CARTESIAN_POINT('Ctrl Pts',(-0.00178111121517929,-0.0208037743898821,
-0.0139550241859274));
#15439=CARTESIAN_POINT('Ctrl Pts',(-0.00212019485783324,-0.0207733690727329,
-0.0136155707477957));
#15440=CARTESIAN_POINT('Ctrl Pts',(-0.00236026563099572,-0.0207429637555837,
-0.0131750429536424));
#15441=CARTESIAN_POINT('Ctrl Pts',(-0.00246132456596799,-0.0207125584384344,
-0.0127047083054078));
#15442=CARTESIAN_POINT('Ctrl Pts',(-0.00249875420312637,-0.0207012970889169,
-0.0125305084166867));
#15443=CARTESIAN_POINT('Ctrl Pts',(-0.00251757532001169,-0.0206900357393996,
-0.0123524778336015));
#15444=CARTESIAN_POINT('Ctrl Pts',(-0.0025174997724744,-0.0206787743898821,
-0.0121747829635494));
#15445=CARTESIAN_POINT('Ctrl Pts',(-0.00251729579631439,-0.0206483690727328,
-0.0116950119670646));
#15446=CARTESIAN_POINT('Ctrl Pts',(-0.00237562415070273,-0.0206179637555834,
-0.0112137432307141));
#15447=CARTESIAN_POINT('Ctrl Pts',(-0.00211455196730226,-0.0205875584384341,
-0.0108096628797779));
#15448=CARTESIAN_POINT('Ctrl Pts',(-0.00201785752757362,-0.0205762970889167,
-0.0106600018832282));
#15449=CARTESIAN_POINT('Ctrl Pts',(-0.00190529247357263,-0.0205650357393995,
-0.0105207865527399));
#15450=CARTESIAN_POINT('Ctrl Pts',(-0.00177959773126699,-0.0205537743898821,
-0.0103951685404929));
#15451=CARTESIAN_POINT('Ctrl Pts',(-0.00144016175196195,-0.0205233633549287,
-0.0100559397690798));
#15452=CARTESIAN_POINT('Ctrl Pts',(-0.000999596726135764,-0.0204929523199754,
-0.00981574134499383));
#15453=CARTESIAN_POINT('Ctrl Pts',(-0.00052918611128424,-0.020462541285022,
-0.00971459988440222));
#15454=CARTESIAN_POINT('Ctrl Pts',(-0.000355079289766713,-0.0204512856533087,
-0.0096771657413976));
#15455=CARTESIAN_POINT('Ctrl Pts',(-0.000177141891441104,-0.0204400300215954,
-0.00965832038682323));
#15456=CARTESIAN_POINT('Ctrl Pts',(4.66948050388447E-7,-0.0204287743898821,
-0.00965835332986306));
#15457=CARTESIAN_POINT('Ctrl Pts',(0.000478571293721941,-0.0203984754112344,
-0.009658442009067));
#15458=CARTESIAN_POINT('Ctrl Pts',(0.000958339118330285,-0.0203681764325867,
-0.00979905048057223));
#15459=CARTESIAN_POINT('Ctrl Pts',(0.00136155392147097,-0.0203378774539389,
-0.0100583129282822));
#15460=CARTESIAN_POINT('Ctrl Pts',(0.00151283361112674,-0.02032650976592,
-0.0101555840163561));
#15461=CARTESIAN_POINT('Ctrl Pts',(0.00165348256099827,-0.020315142077901,
-0.0102690365665635));
#15462=CARTESIAN_POINT('Ctrl Pts',(0.00178025817466354,-0.0203037743898821,
-0.0103958288256184));
#15463=CARTESIAN_POINT('Ctrl Pts',(0.00212450243168519,-0.0202729067710791,
-0.0107401182812365));
#15464=CARTESIAN_POINT('Ctrl Pts',(0.00236662192217892,-0.0202420391522763,
-0.0111881073528289));
#15465=CARTESIAN_POINT('Ctrl Pts',(0.00246545726791875,-0.0202111715334733,
-0.0116666119782703));
#15466=CARTESIAN_POINT('Ctrl Pts',(0.00250003485020926,-0.0202003724856096,
-0.0118340169985972));
#15467=CARTESIAN_POINT('Ctrl Pts',(0.00251749074081832,-0.0201895734377458,
-0.0120049244588735));
#15468=CARTESIAN_POINT('Ctrl Pts',(0.00251749999630341,-0.0201787743898821,
-0.0121757168596234));
#15469=CARTESIAN_POINT('',(0.00251749967158866,-0.019178682372853,-0.0121750998261193));
#15470=CARTESIAN_POINT('Ctrl Pts',(0.00251749999999825,-0.02017876552198,
-0.0121758562566413));
#15471=CARTESIAN_POINT('Ctrl Pts',(0.00251749942404778,-0.0201478985796235,
-0.0126640430232735));
#15472=CARTESIAN_POINT('Ctrl Pts',(0.00237121201732249,-0.0201170316372671,
-0.0131522106873684));
#15473=CARTESIAN_POINT('Ctrl Pts',(0.00210295494144678,-0.0200861646949107,
-0.0135598282734146));
#15474=CARTESIAN_POINT('Ctrl Pts',(0.00200910037981308,-0.0200753653400964,
-0.013702440615429));
#15475=CARTESIAN_POINT('Ctrl Pts',(0.00190076972724618,-0.0200645659852821,
-0.0138353399771734));
#15476=CARTESIAN_POINT('Ctrl Pts',(0.00178033495272378,-0.0200537666304678,
-0.0139558009560445));
#15477=CARTESIAN_POINT('Ctrl Pts',(0.00144244726229051,-0.0200234683294094,
-0.0142937621645035));
#15478=CARTESIAN_POINT('Ctrl Pts',(0.00100395002775284,-0.019993170028351,
-0.0145337717268215));
#15479=CARTESIAN_POINT('Ctrl Pts',(0.000535453448710425,-0.0199628717272925,
-0.0146357508157784));
#15480=CARTESIAN_POINT('Ctrl Pts',(0.000359672394884014,-0.0199515037311802,
-0.0146740136175298));
#15481=CARTESIAN_POINT('Ctrl Pts',(0.000179936394819805,-0.0199401357350679,
-0.0146933139879726));
#15482=CARTESIAN_POINT('Ctrl Pts',(5.50671286675763E-7,-0.0199287677389556,
-0.0146933532263319));
#15483=CARTESIAN_POINT('Ctrl Pts',(-0.000479321396759237,-0.0198983573824538,
-0.0146934581922805));
#15484=CARTESIAN_POINT('Ctrl Pts',(-0.000960765252524083,-0.0198679470259521,
-0.0145520390541735));
#15485=CARTESIAN_POINT('Ctrl Pts',(-0.00136505768018742,-0.0198375366694503,
-0.0142911366670443));
#15486=CARTESIAN_POINT('Ctrl Pts',(-0.00151470050263993,-0.0198262807287813,
-0.0141945675331126));
#15487=CARTESIAN_POINT('Ctrl Pts',(-0.0016539161141768,-0.0198150247881123,
-0.0140821370557623));
#15488=CARTESIAN_POINT('Ctrl Pts',(-0.00177955610029437,-0.0198037688474433,
-0.0139565796372097));
#15489=CARTESIAN_POINT('Ctrl Pts',(-0.00211893586369603,-0.0197733642079718,
-0.0136174229059933));
#15490=CARTESIAN_POINT('Ctrl Pts',(-0.00235939135465183,-0.0197429595685003,
-0.0131771054644321));
#15491=CARTESIAN_POINT('Ctrl Pts',(-0.00246086132166213,-0.0197125549290287,
-0.0127068596947561));
#15492=CARTESIAN_POINT('Ctrl Pts',(-0.0024984450606929,-0.0197012932713295,
-0.0125326840760133));
#15493=CARTESIAN_POINT('Ctrl Pts',(-0.00251742180734246,-0.0196900316136303,
-0.0123546611207697));
#15494=CARTESIAN_POINT('Ctrl Pts',(-0.00251749975779415,-0.019678769955931,
-0.012176957599188));
#15495=CARTESIAN_POINT('Ctrl Pts',(-0.0025177102113032,-0.0196483653164596,
-0.0116971870671051));
#15496=CARTESIAN_POINT('Ctrl Pts',(-0.00237645460119475,-0.0196179606769882,
-0.011215796495468));
#15497=CARTESIAN_POINT('Ctrl Pts',(-0.00211573195307296,-0.0195875560375168,
-0.0108114909619734));
#15498=CARTESIAN_POINT('Ctrl Pts',(-0.00201916217725421,-0.0195762943798175,
-0.010661739127934));
#15499=CARTESIAN_POINT('Ctrl Pts',(-0.00190671120570611,-0.0195650327221181,
-0.0105224202649405));
#15500=CARTESIAN_POINT('Ctrl Pts',(-0.00178111766245729,-0.0195537710644188,
-0.0103966888415214));
#15501=CARTESIAN_POINT('Ctrl Pts',(-0.00144197181674905,-0.0195233607079171,
-0.0100571706718406));
#15502=CARTESIAN_POINT('Ctrl Pts',(-0.00100161251329237,-0.0194929503514154,
-0.0098165961994737));
#15503=CARTESIAN_POINT('Ctrl Pts',(-0.000531288854696852,-0.0194625399949137,
-0.0097150529283667));
#15504=CARTESIAN_POINT('Ctrl Pts',(-0.000357205555275701,-0.0194512840542446,
-0.00967746819847854));
#15505=CARTESIAN_POINT('Ctrl Pts',(-0.000179275420660757,-0.0194400281135756,
-0.00965847080633757));
#15506=CARTESIAN_POINT('Ctrl Pts',(-1.65795391985757E-6,-0.0194287721729066,
-0.00965835383249881));
#15507=CARTESIAN_POINT('Ctrl Pts',(0.000476445799358355,-0.0193984738718482,
-0.00965803896689255));
#15508=CARTESIAN_POINT('Ctrl Pts',(0.000956331742318686,-0.0193681755707899,
-0.00979824216117706));
#15509=CARTESIAN_POINT('Ctrl Pts',(0.00135976503294221,-0.0193378772697315,
-0.0100571637611232));
#15510=CARTESIAN_POINT('Ctrl Pts',(0.00151113418300043,-0.0193265092736191,
-0.0101543117740077));
#15511=CARTESIAN_POINT('Ctrl Pts',(0.00165188522462424,-0.0193151412775067,
-0.0102676518033066));
#15512=CARTESIAN_POINT('Ctrl Pts',(0.00177877270373225,-0.0193037732813944,
-0.0103943443984363));
#15513=CARTESIAN_POINT('Ctrl Pts',(0.00212330382994413,-0.019272906339038,
-0.0107383463660817));
#15514=CARTESIAN_POINT('Ctrl Pts',(0.00236579690432436,-0.0192420393966816,
-0.0111861330421385));
#15515=CARTESIAN_POINT('Ctrl Pts',(0.0024650314678091,-0.0192111724543252,
-0.0116645548289906));
#15516=CARTESIAN_POINT('Ctrl Pts',(0.00249975046422119,-0.0192003730995108,
-0.0118319392938171));
#15517=CARTESIAN_POINT('Ctrl Pts',(0.00251734898190401,-0.0191895737446965,
-0.0120028408387453));
#15518=CARTESIAN_POINT('Ctrl Pts',(0.00251749902856922,-0.0191787743898821,
-0.0121736416914285));
#15519=CARTESIAN_POINT('',(0.00251749999999651,-0.0181788400336509,-0.0121758574807786));
#15520=CARTESIAN_POINT('Ctrl Pts',(0.0025174999999847,-0.0191786353788967,
-0.0121758445091258));
#15521=CARTESIAN_POINT('Ctrl Pts',(0.00251750170207121,-0.0191478104553933,
-0.0126640285958876));
#15522=CARTESIAN_POINT('Ctrl Pts',(0.0023712181033913,-0.019116981663674,
-0.0131521946266093));
#15523=CARTESIAN_POINT('Ctrl Pts',(0.00200907496145789,-0.0190753508046254,
-0.0137024816231192));
#15524=CARTESIAN_POINT('Ctrl Pts',(0.00190069671332285,-0.0190645563654964,
-0.0138354304943692));
#15525=CARTESIAN_POINT('Ctrl Pts',(0.00144229472143091,-0.0190234846160053,
-0.0142938656603467));
#15526=CARTESIAN_POINT('Ctrl Pts',(0.00100378140055006,-0.0189931985744862,
-0.0145338433849123));
#15527=CARTESIAN_POINT('Ctrl Pts',(0.000359425373225544,-0.0189515497284823,
-0.0146740542590721));
#15528=CARTESIAN_POINT('Ctrl Pts',(0.00017961579626026,-0.0189401837567628,
-0.0146933418902656));
#15529=CARTESIAN_POINT('Ctrl Pts',(-0.000479704801724841,-0.0188984297906503,
-0.0146933837415642));
#15530=CARTESIAN_POINT('Ctrl Pts',(-0.00096112004307815,-0.0188680494431272,
-0.014551894086947));
#15531=CARTESIAN_POINT('Ctrl Pts',(-0.00151506125314685,-0.0188263618747039,
-0.0141943035839131));
#15532=CARTESIAN_POINT('Ctrl Pts',(-0.00165431580166961,-0.018815090775692,
-0.0140817973026295));
#15533=CARTESIAN_POINT('Ctrl Pts',(-0.00211926443661562,-0.018773357645065,
-0.0136169330664543));
#15534=CARTESIAN_POINT('Ctrl Pts',(-0.00235961099893533,-0.0187428433006891,
-0.0131765788736037));
#15535=CARTESIAN_POINT('Ctrl Pts',(-0.00249854058101726,-0.0187011966212453,
-0.0125320589461935));
#15536=CARTESIAN_POINT('Ctrl Pts',(-0.00251747899192606,-0.0186899535052533,
-0.0123539416161887));
#15537=CARTESIAN_POINT('Ctrl Pts',(-0.00251755664288924,-0.0186484623083203,
-0.0116962330356729));
#15538=CARTESIAN_POINT('Ctrl Pts',(-0.00237606299894619,-0.0186183855843164,
-0.0112147502638011));
#15539=CARTESIAN_POINT('Ctrl Pts',(-0.00201845434901466,-0.0185771189445961,
-0.0106608047389055));
#15540=CARTESIAN_POINT('Ctrl Pts',(-0.00190598884271828,-0.0185659656408752,
-0.0105215951671963));
#15541=CARTESIAN_POINT('Ctrl Pts',(-0.00144124441175641,-0.0185246278682585,
-0.0100567188361891));
#15542=CARTESIAN_POINT('Ctrl Pts',(-0.0010009741369636,-0.0184943299457318,
-0.00981635764190458));
#15543=CARTESIAN_POINT('Ctrl Pts',(-0.000356395749972991,-0.0184527046799012,
-0.00967733079535345));
#15544=CARTESIAN_POINT('Ctrl Pts',(-0.000178150455788198,-0.0184414340252707,
-0.0096583696678918));
#15545=CARTESIAN_POINT('Ctrl Pts',(0.000477888567463474,-0.0183998548353155,
-0.00965830930438933));
#15546=CARTESIAN_POINT('Ctrl Pts',(0.000957709402945352,-0.0183695109173314,
-0.00979879367698402));
#15547=CARTESIAN_POINT('Ctrl Pts',(0.00151241638113353,-0.0183276938099204,
-0.0101552602800974));
#15548=CARTESIAN_POINT('Ctrl Pts',(0.00165318713052002,-0.0183162711544142,
-0.0102687684694766));
#15549=CARTESIAN_POINT('Ctrl Pts',(0.0021243490727292,-0.018273819192397,
-0.0107398907053701));
#15550=CARTESIAN_POINT('Ctrl Pts',(0.00236651757367148,-0.018242731147569,
-0.0111878560810346));
#15551=CARTESIAN_POINT('Ctrl Pts',(0.00250002625799525,-0.0182006750806357,
-0.0118338865874667));
#15552=CARTESIAN_POINT('Ctrl Pts',(0.0025175002847659,-0.0181897612054126,
-0.0120049301415805));
#15553=CARTESIAN_POINT('Ctrl Pts',(0.00251749999999651,-0.0181788400336509,
-0.0121758574807786));
#15554=CARTESIAN_POINT('',(0.0025174996618868,-0.0171788333650338,-0.012176768974368));
#15555=CARTESIAN_POINT('Ctrl Pts',(0.00251749978208517,-0.0181787743898821,
-0.0121769007602343));
#15556=CARTESIAN_POINT('Ctrl Pts',(0.00251729665938466,-0.0181479131488603,
-0.0126650861589615));
#15557=CARTESIAN_POINT('Ctrl Pts',(0.00237080747747283,-0.0181170519078386,
-0.0131531919847914));
#15558=CARTESIAN_POINT('Ctrl Pts',(0.00210238256047418,-0.0180861906668169,
-0.0135606976169483));
#15559=CARTESIAN_POINT('Ctrl Pts',(0.00200844187027922,-0.0180753901557679,
-0.0137033123964226));
#15560=CARTESIAN_POINT('Ctrl Pts',(0.00190002070867247,-0.018064589644719,
-0.0138362025487504));
#15561=CARTESIAN_POINT('Ctrl Pts',(0.0017794943310653,-0.0180537891336701,
-0.0139566413637044));
#15562=CARTESIAN_POINT('Ctrl Pts',(0.00144144917271534,-0.0180234965077712,
-0.0142944409315743));
#15563=CARTESIAN_POINT('Ctrl Pts',(0.00100284143968462,-0.0179932038818723,
-0.0145342429641631));
#15564=CARTESIAN_POINT('Ctrl Pts',(0.000534299314744759,-0.0179629112559734,
-0.014636001756115));
#15565=CARTESIAN_POINT('Ctrl Pts',(0.000358450758299624,-0.0179515421298016,
-0.0146741928508275));
#15566=CARTESIAN_POINT('Ctrl Pts',(0.000178653920795057,-0.0179401730036298,
-0.0146934089138742));
#15567=CARTESIAN_POINT('Ctrl Pts',(-7.82159575315025E-7,-0.017928803877458,
-0.0146933531650539));
#15568=CARTESIAN_POINT('Ctrl Pts',(-0.000480651474567896,-0.0178983992075785,
-0.0146932040749257));
#15569=CARTESIAN_POINT('Ctrl Pts',(-0.000962018237753669,-0.017867994537699,
-0.0145515316086698));
#15570=CARTESIAN_POINT('Ctrl Pts',(-0.0013661713923947,-0.0178375898678195,
-0.0142904175387392));
#15571=CARTESIAN_POINT('Ctrl Pts',(-0.0015158058168978,-0.0178263327856283,
-0.0141937421741279));
#15572=CARTESIAN_POINT('Ctrl Pts',(-0.00165499872077991,-0.0178150757034371,
-0.014081201916579));
#15573=CARTESIAN_POINT('Ctrl Pts',(-0.00178060053003004,-0.0178038186212459,
-0.0139555352813135));
#15574=CARTESIAN_POINT('Ctrl Pts',(-0.00211977937025927,-0.0177734196635815,
-0.0136161813829952));
#15575=CARTESIAN_POINT('Ctrl Pts',(-0.00235997606698392,-0.017743020705917,
-0.0131757254849616));
#15576=CARTESIAN_POINT('Ctrl Pts',(-0.00246117097680353,-0.0177126217482525,
-0.0127054226143519));
#15577=CARTESIAN_POINT('Ctrl Pts',(-0.002498663626283,-0.0177013589538463,
-0.0125311757010596));
#15578=CARTESIAN_POINT('Ctrl Pts',(-0.00251753643997218,-0.0176900961594401,
-0.0123530901387271));
#15579=CARTESIAN_POINT('Ctrl Pts',(-0.00251749994694553,-0.0176788333650338,
-0.0121753364410923));
#15580=CARTESIAN_POINT('Ctrl Pts',(-0.0025174014500777,-0.0176484344073693,
-0.0116955685491982));
#15581=CARTESIAN_POINT('Ctrl Pts',(-0.00237583737863047,-0.0176180354497047,
-0.011214271138594));
#15582=CARTESIAN_POINT('Ctrl Pts',(-0.00211485669286262,-0.0175876364920402,
-0.0108101346410626));
#15583=CARTESIAN_POINT('Ctrl Pts',(-0.00201816351541162,-0.017576373697634,
-0.0106604023267525));
#15584=CARTESIAN_POINT('Ctrl Pts',(-0.00190558679701245,-0.0175651109032279,
-0.0105211191169428));
#15585=CARTESIAN_POINT('Ctrl Pts',(-0.00177986963867943,-0.0175538481088218,
-0.0103954403234208));
#15586=CARTESIAN_POINT('Ctrl Pts',(-0.00144048772692144,-0.0175234434389423,
-0.0100561619800467));
#15587=CARTESIAN_POINT('Ctrl Pts',(-0.00099996244018008,-0.0174930387690628,
-0.00981589679331808));
#15588=CARTESIAN_POINT('Ctrl Pts',(-0.000529570110150823,-0.0174626340991833,
-0.00971468247809419));
#15589=CARTESIAN_POINT('Ctrl Pts',(-0.000355411168703594,-0.0174513770169921,
-0.00967720869956213));
#15590=CARTESIAN_POINT('Ctrl Pts',(-0.00017741619453138,-0.0174401199348009,
-0.00965833554778184));
#15591=CARTESIAN_POINT('Ctrl Pts',(2.51531350274394E-7,-0.0174288628526097,
-0.00965835329912374));
#15592=CARTESIAN_POINT('Ctrl Pts',(0.000478352504853852,-0.0173985702267108,
-0.00965840106769734));
#15593=CARTESIAN_POINT('Ctrl Pts',(0.000958129698327566,-0.0173682776008119,
-0.00979896659453205));
#15594=CARTESIAN_POINT('Ctrl Pts',(0.00136136532735725,-0.0173379849749131,
-0.0100581916763216));
#15595=CARTESIAN_POINT('Ctrl Pts',(0.00151270370121509,-0.0173266158487412,
-0.0101554814481495));
#15596=CARTESIAN_POINT('Ctrl Pts',(0.00165340570642434,-0.0173152467225694,
-0.0102689643764695));
#15597=CARTESIAN_POINT('Ctrl Pts',(0.00178022537647008,-0.0173038775963976,
-0.010395796023723));
#15598=CARTESIAN_POINT('Ctrl Pts',(0.0021244745601289,-0.017273016355376,
-0.0107400777192469));
#15599=CARTESIAN_POINT('Ctrl Pts',(0.00236660208174994,-0.0172421551143543,
-0.0111880604961051));
#15600=CARTESIAN_POINT('Ctrl Pts',(0.00246544689552489,-0.0172112938733326,
-0.0116665617636101));
#15601=CARTESIAN_POINT('Ctrl Pts',(0.00250003962310081,-0.0172004933622836,
-0.0118340228914061));
#15602=CARTESIAN_POINT('Ctrl Pts',(0.00251749906459384,-0.0171896928512346,
-0.0120049892050111));
#15603=CARTESIAN_POINT('Ctrl Pts',(0.00251749999996227,-0.0171788923401855,
-0.0121758395037901));
#15604=CARTESIAN_POINT('',(0.00251749963321368,-0.0161787130482344,-0.0121748985097519));
#15605=CARTESIAN_POINT('Ctrl Pts',(0.00251749932381133,-0.0171787743898821,
-0.012177698444946));
#15606=CARTESIAN_POINT('Ctrl Pts',(0.00251714151439738,-0.0171479040308582,
-0.0126658868647471));
#15607=CARTESIAN_POINT('Ctrl Pts',(0.00237049591654825,-0.0171170336718345,
-0.0131539488348971));
#15608=CARTESIAN_POINT('Ctrl Pts',(0.00210193894734248,-0.0170861633128106,
-0.0135613708474879));
#15609=CARTESIAN_POINT('Ctrl Pts',(0.00200801637077188,-0.0170753670051678,
-0.0137038587720697));
#15610=CARTESIAN_POINT('Ctrl Pts',(0.00189963613076377,-0.0170645706975249,
-0.0138366307209233));
#15611=CARTESIAN_POINT('Ctrl Pts',(0.00177916928923548,-0.0170537743898821,
-0.0139569661101157));
#15612=CARTESIAN_POINT('Ctrl Pts',(0.00144105763519167,-0.0170234726289297,
-0.0142947088197582));
#15613=CARTESIAN_POINT('Ctrl Pts',(0.00100239963061137,-0.0169931708679771,
-0.0145344318790767));
#15614=CARTESIAN_POINT('Ctrl Pts',(0.000533832953673381,-0.0169628691070247,
-0.0146361029949358));
#15615=CARTESIAN_POINT('Ctrl Pts',(0.000358093460758483,-0.0169515042013105,
-0.0146742355195573));
#15616=CARTESIAN_POINT('Ctrl Pts',(0.000178414513428729,-0.0169401392955963,
-0.0146934174733652));
#15617=CARTESIAN_POINT('Ctrl Pts',(-9.03414161335177E-7,-0.0169287743898821,
-0.0146933531244613));
#15618=CARTESIAN_POINT('Ctrl Pts',(-0.000480779152462688,-0.016898360573519,
-0.0146931809192714));
#15619=CARTESIAN_POINT('Ctrl Pts',(-0.000962144144701767,-0.016867946757156,
-0.0145514816527625));
#15620=CARTESIAN_POINT('Ctrl Pts',(-0.00136628727402242,-0.016837532940793,
-0.0142903426657805));
#15621=CARTESIAN_POINT('Ctrl Pts',(-0.00151581675369036,-0.0168262800904893,
-0.01419372348804));
#15622=CARTESIAN_POINT('Ctrl Pts',(-0.00165491782093178,-0.0168150272401857,
-0.0140812611991804));
#15623=CARTESIAN_POINT('Ctrl Pts',(-0.00178044714873814,-0.0168037743898821,
-0.0139556887285443));
#15624=CARTESIAN_POINT('Ctrl Pts',(-0.00211965965503896,-0.016773366296242,
-0.0136163596392294));
#15625=CARTESIAN_POINT('Ctrl Pts',(-0.00235989530171396,-0.0167429582026018,
-0.0131759184826837));
#15626=CARTESIAN_POINT('Ctrl Pts',(-0.00246112875058267,-0.0167125501089617,
-0.0127056188224845));
#15627=CARTESIAN_POINT('Ctrl Pts',(-0.00249861035631251,-0.0167012915359351,
-0.012531490738976));
#15628=CARTESIAN_POINT('Ctrl Pts',(-0.00251749729511135,-0.0166900329629087,
-0.0123535276339294));
#15629=CARTESIAN_POINT('Ctrl Pts',(-0.0025174999997082,-0.0166787743898821,
-0.0121758916167497));
#15630=CARTESIAN_POINT('Ctrl Pts',(-0.0025175073045091,-0.0166483662962419,
-0.011696117436527));
#15631=CARTESIAN_POINT('Ctrl Pts',(-0.00237604584935783,-0.0166179582026016,
-0.0112147838942784));
#15632=CARTESIAN_POINT('Ctrl Pts',(-0.0021151489841834,-0.0165875501089614,
-0.0108105873693435));
#15633=CARTESIAN_POINT('Ctrl Pts',(-0.00201855212271358,-0.0165762915359349,
-0.0106609339202703));
#15634=CARTESIAN_POINT('Ctrl Pts',(-0.00190609068656835,-0.0165650329629086,
-0.0105217122176387));
#15635=CARTESIAN_POINT('Ctrl Pts',(-0.00178050134567524,-0.0165537743898821,
-0.0103960720617867));
#15636=CARTESIAN_POINT('Ctrl Pts',(-0.00144123533548841,-0.0165233605735191,
-0.010056668780489));
#15637=CARTESIAN_POINT('Ctrl Pts',(-0.00100078923118645,-0.0164929467571562,
-0.00981624624970903));
#15638=CARTESIAN_POINT('Ctrl Pts',(-0.000530427177695476,-0.0164625329407932,
-0.00971486704946492));
#15639=CARTESIAN_POINT('Ctrl Pts',(-0.000356397265983295,-0.0164512800904895,
-0.00967735761787496));
#15640=CARTESIAN_POINT('Ctrl Pts',(-0.000178529965730701,-0.0164400272401858,
-0.00965842259834124));
#15641=CARTESIAN_POINT('Ctrl Pts',(-9.80074539332744E-7,-0.0164287743898821,
-0.0096583534773319));
#15642=CARTESIAN_POINT('Ctrl Pts',(0.000477127623938968,-0.0163984726289296,
-0.00965816734775183));
#15643=CARTESIAN_POINT('Ctrl Pts',(0.000956978853136251,-0.0163681708679771,
-0.00979850192424106));
#15644=CARTESIAN_POINT('Ctrl Pts',(0.00136034396970021,-0.0163378691070246,
-0.010057535431726));
#15645=CARTESIAN_POINT('Ctrl Pts',(0.00151162912191674,-0.0163265042013105,
-0.0101546879171538));
#15646=CARTESIAN_POINT('Ctrl Pts',(0.00165229984926619,-0.0163151392955962,
-0.0102680171781157));
#15647=CARTESIAN_POINT('Ctrl Pts',(0.00177911505175044,-0.0163037743898821,
-0.0103946862863487));
#15648=CARTESIAN_POINT('Ctrl Pts',(0.00212358168691954,-0.0162729040308583,
-0.0107387560874303));
#15649=CARTESIAN_POINT('Ctrl Pts',(0.00236598895617194,-0.0162420336718344,
-0.0111865914635291));
#15650=CARTESIAN_POINT('Ctrl Pts',(0.00246513082529533,-0.0162111633128106,
-0.0116650340776605));
#15651=CARTESIAN_POINT('Ctrl Pts',(0.00249980376572062,-0.0162003670051677,
-0.0118323600762862));
#15652=CARTESIAN_POINT('Ctrl Pts',(0.00251736893054138,-0.0161895706975249,
-0.0120031970670941));
#15653=CARTESIAN_POINT('Ctrl Pts',(0.00251749926645723,-0.0161787743898821,
-0.0121739314678082));
#15654=CARTESIAN_POINT('',(0.00251755538663573,-0.015178857044612,-0.0121751343114423));
#15655=CARTESIAN_POINT('Ctrl Pts',(0.00251749999997012,-0.0161786517065868,
-0.0121758655516955));
#15656=CARTESIAN_POINT('Ctrl Pts',(0.00251749762155505,-0.0161477908369676,
-0.0126640508647007));
#15657=CARTESIAN_POINT('Ctrl Pts',(0.00237120923608777,-0.0161169299673483,
-0.0131522167799313));
#15658=CARTESIAN_POINT('Ctrl Pts',(0.00210295203127188,-0.0160860690977291,
-0.0135598326954257));
#15659=CARTESIAN_POINT('Ctrl Pts',(0.0020090673912971,-0.0160752684124856,
-0.0137024900883574));
#15660=CARTESIAN_POINT('Ctrl Pts',(0.00190069746994918,-0.0160644677272422,
-0.0138354282650385));
#15661=CARTESIAN_POINT('Ctrl Pts',(0.00178021660930023,-0.0160536670419987,
-0.0139559193173478));
#15662=CARTESIAN_POINT('Ctrl Pts',(0.00144230871570574,-0.0160233747882719,
-0.0142938557950883));
#15663=CARTESIAN_POINT('Ctrl Pts',(0.00100379856888952,-0.0159930825345452,
-0.0145338356963433));
#15664=CARTESIAN_POINT('Ctrl Pts',(0.000535298010146728,-0.0159627902808184,
-0.0146357846454242));
#15665=CARTESIAN_POINT('Ctrl Pts',(0.000359460187621698,-0.0159514209796825,
-0.0146740481669517));
#15666=CARTESIAN_POINT('Ctrl Pts',(0.000179666165241272,-0.0159400516785465,
-0.014693337223714));
#15667=CARTESIAN_POINT('Ctrl Pts',(2.25215308823281E-7,-0.0159286823774106,
-0.0146933532764842));
#15668=CARTESIAN_POINT('Ctrl Pts',(-0.000479643856273245,-0.0158982780801603,
-0.0146933962055256));
#15669=CARTESIAN_POINT('Ctrl Pts',(-0.000961067062991505,-0.0158678737829099,
-0.0145519165176877));
#15670=CARTESIAN_POINT('Ctrl Pts',(-0.00136532456468596,-0.0158374694856596,
-0.0142909644143869));
#15671=CARTESIAN_POINT('Ctrl Pts',(-0.00151500178961346,-0.0158262122280472,
-0.014194346326912));
#15672=CARTESIAN_POINT('Ctrl Pts',(-0.00165424327245194,-0.0158149549704349,
-0.014081858293453));
#15673=CARTESIAN_POINT('Ctrl Pts',(-0.00177989809173394,-0.0158036977128225,
-0.0139562378048692));
#15674=CARTESIAN_POINT('Ctrl Pts',(-0.00211921063967702,-0.0157732991273554,
-0.0136170179619792));
#15675=CARTESIAN_POINT('Ctrl Pts',(-0.00235958108989582,-0.0157429005418882,
-0.0131766571301363));
#15676=CARTESIAN_POINT('Ctrl Pts',(-0.0024609616650532,-0.0157125019564211,
-0.0127063944566275));
#15677=CARTESIAN_POINT('Ctrl Pts',(-0.00249852414691729,-0.0157012389870255,
-0.0125321575959901));
#15678=CARTESIAN_POINT('Ctrl Pts',(-0.00251746728692474,-0.01568997601763,
-0.0123540745231461));
#15679=CARTESIAN_POINT('Ctrl Pts',(-0.00251749995748017,-0.0156787130482344,
-0.0121763159823111));
#15680=CARTESIAN_POINT('Ctrl Pts',(-0.00251758813481925,-0.0156483144627673,
-0.0116965483467703));
#15681=CARTESIAN_POINT('Ctrl Pts',(-0.00237621148852556,-0.0156179158773003,
-0.0112151960937125));
#15682=CARTESIAN_POINT('Ctrl Pts',(-0.00211538828755822,-0.0155875172918331,
-0.0108109581833133));
#15683=CARTESIAN_POINT('Ctrl Pts',(-0.00201875077350902,-0.0155762543224375,
-0.0106611841348371));
#15684=CARTESIAN_POINT('Ctrl Pts',(-0.00190622477840748,-0.0155649913530419,
-0.0105218535800564));
#15685=CARTESIAN_POINT('Ctrl Pts',(-0.00178055241147931,-0.0155537283836464,
-0.0103961231497185));
#15686=CARTESIAN_POINT('Ctrl Pts',(-0.00144130084592552,-0.0155233240863961,
-0.0100567148424469));
#15687=CARTESIAN_POINT('Ctrl Pts',(-0.00100086800023652,-0.0154929197891457,
-0.00981628074575207));
#15688=CARTESIAN_POINT('Ctrl Pts',(-0.000530514760432268,-0.0154625154918954,
-0.00971488592818791));
#15689=CARTESIAN_POINT('Ctrl Pts',(-0.000356365443784941,-0.015451258234283,
-0.00967734427503011));
#15690=CARTESIAN_POINT('Ctrl Pts',(-0.000178372744225681,-0.0154400009766707,
-0.00965840279886414));
#15691=CARTESIAN_POINT('Ctrl Pts',(-7.00176193161934E-7,-0.0154287437190583,
-0.00965835338392586));
#15692=CARTESIAN_POINT('Ctrl Pts',(0.000477400503071805,-0.0153984514653315,
-0.00965822041283291));
#15693=CARTESIAN_POINT('Ctrl Pts',(0.000957230582051071,-0.0153681592116047,
-0.009798604400552));
#15694=CARTESIAN_POINT('Ctrl Pts',(0.00136056406704873,-0.0153378669578779,
-0.0100576767902633));
#15695=CARTESIAN_POINT('Ctrl Pts',(0.00151194335663502,-0.015326497656742,
-0.0101549119461942));
#15696=CARTESIAN_POINT('Ctrl Pts',(0.00165269182272679,-0.0153151283556061,
-0.0102683451667279));
#15697=CARTESIAN_POINT('Ctrl Pts',(0.00177956216610836,-0.0153037590544702,
-0.0103951329977548));
#15698=CARTESIAN_POINT('Ctrl Pts',(0.0021239394571007,-0.0152728981848508,
-0.0107392863169314));
#15699=CARTESIAN_POINT('Ctrl Pts',(0.00236623382097467,-0.0152420373152316,
-0.0111871787171439));
#15700=CARTESIAN_POINT('Ctrl Pts',(0.00246525692736654,-0.0152111764456122,
-0.0116656430043496));
#15701=CARTESIAN_POINT('Ctrl Pts',(0.00249991302802582,-0.0152003757603689,
-0.0118330959060355));
#15702=CARTESIAN_POINT('Ctrl Pts',(0.0025174361894798,-0.0151895750751254,
-0.0120040605760843));
#15703=CARTESIAN_POINT('Ctrl Pts',(0.00251749982538233,-0.0151787743898821,
-0.012174915629931));
#15704=CARTESIAN_POINT('',(0.00251749939328164,-0.0141788271636735,-0.0121772344157477));
#15705=CARTESIAN_POINT('Ctrl Pts',(0.00251749999999728,-0.0151787156439641,
-0.0121758495859091));
#15706=CARTESIAN_POINT('Ctrl Pts',(0.00251750071291988,-0.0151481640251222,
-0.0126608409072188));
#15707=CARTESIAN_POINT('Ctrl Pts',(0.00237305979471814,-0.0151175938090383,
-0.0131460901801096));
#15708=CARTESIAN_POINT('Ctrl Pts',(0.00210809033725665,-0.0150870046971682,
-0.0135519933157576));
#15709=CARTESIAN_POINT('Ctrl Pts',(0.00201298073055038,-0.015076024871692,
-0.0136976904385964));
#15710=CARTESIAN_POINT('Ctrl Pts',(0.00190281808401211,-0.0150650426116467,
-0.0138333165509995));
#15711=CARTESIAN_POINT('Ctrl Pts',(0.00178015071638259,-0.0150540579032255,
-0.0139559852134002));
#15712=CARTESIAN_POINT('Ctrl Pts',(0.00144068287806857,-0.0150236589854504,
-0.0142954566348445));
#15713=CARTESIAN_POINT('Ctrl Pts',(0.000999660018196464,-0.0149932413169844,
-0.0145361596170759));
#15714=CARTESIAN_POINT('Ctrl Pts',(0.000528147072577002,-0.014962805775685,
-0.0146373298596191));
#15715=CARTESIAN_POINT('Ctrl Pts',(0.000354599300466907,-0.0149516034949533,
-0.0146745671621372));
#15716=CARTESIAN_POINT('Ctrl Pts',(0.000177183293706389,-0.0149403987929458,
-0.0146933526631847));
#15717=CARTESIAN_POINT('Ctrl Pts',(8.8573912000701E-9,-0.014929191713435,
-0.0146933532865425));
#15718=CARTESIAN_POINT('Ctrl Pts',(-0.000329261486051471,-0.0149083638841147,
-0.0146933544450236));
#15719=CARTESIAN_POINT('Ctrl Pts',(-0.000658847952640571,-0.0148875278432613,
-0.0146278709517489));
#15720=CARTESIAN_POINT('Ctrl Pts',(-0.000963399403632745,-0.0148666807812065,
-0.0145017225518179));
#15721=CARTESIAN_POINT('Ctrl Pts',(-0.00126795085462492,-0.0148458337191516,
-0.0143755741518868));
#15722=CARTESIAN_POINT('Ctrl Pts',(-0.00154719964135841,-0.0148249756358953,
-0.0141889354689233));
#15723=CARTESIAN_POINT('Ctrl Pts',(-0.00178013819010309,-0.0148041179574223,
-0.0139559977397238));
#15724=CARTESIAN_POINT('Ctrl Pts',(-0.00189660746447543,-0.0147936891181858,
-0.013839528875124));
#15725=CARTESIAN_POINT('Ctrl Pts',(-0.00200162166373276,-0.0147832603801451,
-0.0137115946618794));
#15726=CARTESIAN_POINT('Ctrl Pts',(-0.00209322290365292,-0.0147728170861969,
-0.0135745041098957));
#15727=CARTESIAN_POINT('Ctrl Pts',(-0.00218482414357308,-0.0147623737922487,
-0.0134374135579119));
#15728=CARTESIAN_POINT('Ctrl Pts',(-0.00226296456431943,-0.0147519159423931,
-0.0132911176945691));
#15729=CARTESIAN_POINT('Ctrl Pts',(-0.002325865875714,-0.0147415032420826,
-0.0131392608732986));
#15730=CARTESIAN_POINT('Ctrl Pts',(-0.00238876718710857,-0.0147310905417721,
-0.0129874040520281));
#15731=CARTESIAN_POINT('Ctrl Pts',(-0.00243667461938459,-0.0147207229910068,
-0.0128301416474611));
#15732=CARTESIAN_POINT('Ctrl Pts',(-0.00246912672741954,-0.0147101764250794,
-0.0126669942581156));
#15733=CARTESIAN_POINT('Ctrl Pts',(-0.00248535278143701,-0.0147049031421157,
-0.0125854205634429));
#15734=CARTESIAN_POINT('Ctrl Pts',(-0.00249752695350485,-0.0146995851053614,
-0.0125023196953955));
#15735=CARTESIAN_POINT('Ctrl Pts',(-0.00250537749513714,-0.0146945081517445,
-0.0124226119882493));
#15736=CARTESIAN_POINT('Ctrl Pts',(-0.00250930276595329,-0.014691969674936,
-0.0123827581346762));
#15737=CARTESIAN_POINT('Ctrl Pts',(-0.00251228671057559,-0.0146894914689118,
-0.0123437732872266));
#15738=CARTESIAN_POINT('Ctrl Pts',(-0.00251446754741514,-0.0146866727988687,
-0.0122993814331324));
#15739=CARTESIAN_POINT('Ctrl Pts',(-0.00251664838425469,-0.0146838541288256,
-0.0122549895790381));
#15740=CARTESIAN_POINT('Ctrl Pts',(-0.0025175,-0.0146806949947635,-0.0122051596879933));
#15741=CARTESIAN_POINT('Ctrl Pts',(-0.0025175,-0.0146788366351873,-0.0121758532865581));
#15742=CARTESIAN_POINT('Ctrl Pts',(-0.0025175,-0.0146769782756111,-0.0121465468851228));
#15743=CARTESIAN_POINT('Ctrl Pts',(-0.00251725426100465,-0.0146764206905208,
-0.0121377557191278));
#15744=CARTESIAN_POINT('Ctrl Pts',(-0.00251694772361996,-0.0146754929894721,
-0.0121231237259275));
#15745=CARTESIAN_POINT('Ctrl Pts',(-0.00251664118623527,-0.0146745652884234,
-0.0121084917327271));
#15746=CARTESIAN_POINT('Ctrl Pts',(-0.00251604607189495,-0.0146732674714164,
-0.0120880271427794));
#15747=CARTESIAN_POINT('Ctrl Pts',(-0.00251519594101278,-0.0146720075132562,
-0.012068170287376));
#15748=CARTESIAN_POINT('Ctrl Pts',(-0.00251349567924844,-0.0146694875969357,
-0.0120284565765692));
#15749=CARTESIAN_POINT('Ctrl Pts',(-0.00251102772241131,-0.0146671191160024,
-0.0119911552048106));
#15750=CARTESIAN_POINT('Ctrl Pts',(-0.00250750307707114,-0.0146646110693223,
-0.0119517225914742));
#15751=CARTESIAN_POINT('Ctrl Pts',(-0.00250045378639079,-0.0146595949759621,
-0.0118728573648014));
#15752=CARTESIAN_POINT('Ctrl Pts',(-0.00248880263071647,-0.0146540206196144,
-0.0117855188015991));
#15753=CARTESIAN_POINT('Ctrl Pts',(-0.00247095694289093,-0.0146481162154468,
-0.0116940047248926));
#15754=CARTESIAN_POINT('Ctrl Pts',(-0.0024531112550654,-0.0146422118112792,
-0.0116024906481861));
#15755=CARTESIAN_POINT('Ctrl Pts',(-0.00242921266780654,-0.0146359773592916,
-0.0115067594572136));
#15756=CARTESIAN_POINT('Ctrl Pts',(-0.0023972519619071,-0.0146293520735607,
-0.0114070950143213));
#15757=CARTESIAN_POINT('Ctrl Pts',(-0.00236529125600766,-0.0146227267878298,
-0.0113074305714289));
#15758=CARTESIAN_POINT('Ctrl Pts',(-0.00232522920184558,-0.0146157106683554,
-0.0112038539433981));
#15759=CARTESIAN_POINT('Ctrl Pts',(-0.0022751852637213,-0.0146083186436641,
-0.01109819922994));
#15760=CARTESIAN_POINT('Ctrl Pts',(-0.00217509738747274,-0.0145935345942814,
-0.0108868898030238));
#15761=CARTESIAN_POINT('Ctrl Pts',(-0.00203504218911522,-0.0145772469240307,
-0.0106673103909374));
#15762=CARTESIAN_POINT('Ctrl Pts',(-0.00184324713000241,-0.0145594439198393,
-0.0104611386549829));
#15763=CARTESIAN_POINT('Ctrl Pts',(-0.0016514520708896,-0.014541640915648,
-0.0102549669190285));
#15764=CARTESIAN_POINT('Ctrl Pts',(-0.00140748406223656,-0.0145223225775161,
-0.0100626956686912));
#15765=CARTESIAN_POINT('Ctrl Pts',(-0.00111175942872558,-0.0145014920439725,
-0.00991713745169976));
#15766=CARTESIAN_POINT('Ctrl Pts',(-0.000816034795214608,-0.014480661510429,
-0.00977157923470835));
#15767=CARTESIAN_POINT('Ctrl Pts',(-0.000468174670655183,-0.014458318781474,
-0.00967362327560147));
#15768=CARTESIAN_POINT('Ctrl Pts',(-9.0880954173227E-5,-0.0144344630160636,
-0.00965999420819767));
#15769=CARTESIAN_POINT('Ctrl Pts',(0.000286412762308729,-0.0144106072506532,
-0.00964636514079386));
#15770=CARTESIAN_POINT('Ctrl Pts',(0.000693089871217907,-0.0143852384487876,
-0.00971851511006437));
#15771=CARTESIAN_POINT('Ctrl Pts',(0.00107766354684713,-0.0143583568361125,
-0.00990067251796038));
#15772=CARTESIAN_POINT('Ctrl Pts',(0.00146223722247635,-0.0143314752234374,
-0.0100828299258564));
#15773=CARTESIAN_POINT('Ctrl Pts',(0.00182358312527259,-0.014303080799953,
-0.0103768885650704));
#15774=CARTESIAN_POINT('Ctrl Pts',(0.00208795759600706,-0.0142731735041193,
-0.0107693543255644));
#15775=CARTESIAN_POINT('Ctrl Pts',(0.00233330315158756,-0.0142454188495498,
-0.0111335715277292));
#15776=CARTESIAN_POINT('Ctrl Pts',(0.00249357887136464,-0.0142163612692967,
-0.0115834060038655));
#15777=CARTESIAN_POINT('Ctrl Pts',(0.00251499973632202,-0.0141860007797548,
-0.012063681203132));
#15778=CARTESIAN_POINT('Ctrl Pts',(0.00251666095110628,-0.0141836462859384,
-0.012100927143626));
#15779=CARTESIAN_POINT('Ctrl Pts',(0.0025175001312269,-0.0141812839561704,
-0.0121383331360715));
#15780=CARTESIAN_POINT('Ctrl Pts',(0.00251749999998461,-0.0141789137904583,
-0.0121758620904934));
#15781=CARTESIAN_POINT('',(0.0025175,-0.0131787743898721,-0.012175853286558));
#15782=CARTESIAN_POINT('Ctrl Pts',(0.00251749902367291,-0.0141787743898821,
-0.0121780704482395));
#15783=CARTESIAN_POINT('Ctrl Pts',(0.00251706907769517,-0.0141479071685421,
-0.012666257028528));
#15784=CARTESIAN_POINT('Ctrl Pts',(0.00237035237263466,-0.0141170399472022,
-0.013154295843589));
#15785=CARTESIAN_POINT('Ctrl Pts',(0.00210173688987106,-0.0140861727258623,
-0.0135616773359075));
#15786=CARTESIAN_POINT('Ctrl Pts',(0.00200775699488553,-0.0140753732805355,
-0.0137042069826473));
#15787=CARTESIAN_POINT('Ctrl Pts',(0.00189930957625436,-0.0140645738352088,
-0.0138370109335702));
#15788=CARTESIAN_POINT('Ctrl Pts',(0.00177876899422965,-0.0140537743898821,
-0.0139573658784775));
#15789=CARTESIAN_POINT('Ctrl Pts',(0.00144058422971941,-0.0140234758148021,
-0.0142950298254853));
#15790=CARTESIAN_POINT('Ctrl Pts',(0.00100187609621577,-0.0139931772397221,
-0.0145346536854798));
#15791=CARTESIAN_POINT('Ctrl Pts',(0.000533290013078261,-0.013962878664642,
-0.0146362207412183));
#15792=CARTESIAN_POINT('Ctrl Pts',(0.00035747549060425,-0.0139515105730554,
-0.0146743289225031));
#15793=CARTESIAN_POINT('Ctrl Pts',(0.00017772270395627,-0.0139401424814687,
-0.0146934712260336));
#15794=CARTESIAN_POINT('Ctrl Pts',(-1.66287135762318E-6,-0.0139287743898821,
-0.0146933527373741));
#15795=CARTESIAN_POINT('Ctrl Pts',(-0.000481534852372283,-0.0138983637583667,
-0.0146930357699276));
#15796=CARTESIAN_POINT('Ctrl Pts',(-0.000962854182385809,-0.0138679531268514,
-0.0145511933676515));
#15797=CARTESIAN_POINT('Ctrl Pts',(-0.00136691705462027,-0.013837542495336,
-0.0142899355971099));
#15798=CARTESIAN_POINT('Ctrl Pts',(-0.00151647481342291,-0.0138262864601847,
-0.0141932349860988));
#15799=CARTESIAN_POINT('Ctrl Pts',(-0.00165559143238043,-0.0138150304250334,
-0.014080682226469));
#15800=CARTESIAN_POINT('Ctrl Pts',(-0.00178112090832962,-0.0138037743898821,
-0.0139550144821531));
#15801=CARTESIAN_POINT('Ctrl Pts',(-0.00212020238086612,-0.0137733694754573,
-0.0136155595177253));
#15802=CARTESIAN_POINT('Ctrl Pts',(-0.00236027068215153,-0.0137429645610325,
-0.0131750308481881));
#15803=CARTESIAN_POINT('Ctrl Pts',(-0.00246132719935155,-0.0137125596466076,
-0.0127046960493263));
#15804=CARTESIAN_POINT('Ctrl Pts',(-0.00249875777531793,-0.0137012978943658,
-0.0125304875677141));
#15805=CARTESIAN_POINT('Ctrl Pts',(-0.00251757800760962,-0.013690036142124,
-0.0123524481141251));
#15806=CARTESIAN_POINT('Ctrl Pts',(-0.00251749975591821,-0.0136787743898821,
-0.0121747447056049));
#15807=CARTESIAN_POINT('Ctrl Pts',(-0.00251728848897417,-0.0136483694754573,
-0.0116949741678561));
#15808=CARTESIAN_POINT('Ctrl Pts',(-0.00237560978566041,-0.0136179645610324,
-0.0112137079417602));
#15809=CARTESIAN_POINT('Ctrl Pts',(-0.00211453184685873,-0.0135875596466076,
-0.0108096317384115));
#15810=CARTESIAN_POINT('Ctrl Pts',(-0.00201783053661956,-0.0135762978943657,
-0.0106599649435852));
#15811=CARTESIAN_POINT('Ctrl Pts',(-0.00190525722781884,-0.013565036142124,
-0.0105207450621084));
#15812=CARTESIAN_POINT('Ctrl Pts',(-0.00177955331071196,-0.0135537743898821,
-0.0103951241481617));
#15813=CARTESIAN_POINT('Ctrl Pts',(-0.00144010919747922,-0.0135233637583667,
-0.010055904172209));
#15814=CARTESIAN_POINT('Ctrl Pts',(-0.000999538623246463,-0.0134929531268514,
-0.00981571681272789));
#15815=CARTESIAN_POINT('Ctrl Pts',(-0.00052912589697104,-0.013462542495336,
-0.00971458693868865));
#15816=CARTESIAN_POINT('Ctrl Pts',(-0.000355009743549373,-0.0134512864601847,
-0.00967715524587891));
#15817=CARTESIAN_POINT('Ctrl Pts',(-0.000177063097394015,-0.0134400304250334,
-0.00965831424067397));
#15818=CARTESIAN_POINT('Ctrl Pts',(5.54290495030118E-7,-0.0134287743898821,
-0.00965835334757854));
#15819=CARTESIAN_POINT('Ctrl Pts',(0.000478658142352042,-0.0133984758148021,
-0.00965845861408386));
#15820=CARTESIAN_POINT('Ctrl Pts',(0.000958420702075833,-0.013368177239722,
-0.00979908345595051));
#15821=CARTESIAN_POINT('Ctrl Pts',(0.0013616263130965,-0.0133378786646419,
-0.0100583594770079));
#15822=CARTESIAN_POINT('Ctrl Pts',(0.00151290993954471,-0.0133265105730553,
-0.0101556404067483));
#15823=CARTESIAN_POINT('Ctrl Pts',(0.00165356124644845,-0.0133151424814687,
-0.010269103995322));
#15824=CARTESIAN_POINT('Ctrl Pts',(0.00178033728213873,-0.0133037743898821,
-0.0103959079469965));
#15825=CARTESIAN_POINT('Ctrl Pts',(0.00212456603191952,-0.0132729071685422,
-0.0107402124956799));
#15826=CARTESIAN_POINT('Ctrl Pts',(0.00236666557989477,-0.0132420399472021,
-0.0111882120610907));
#15827=CARTESIAN_POINT('Ctrl Pts',(0.0024654797540446,-0.0132111727258622,
-0.0116667208554597));
#15828=CARTESIAN_POINT('Ctrl Pts',(0.00250005164697466,-0.0132003732805357,
-0.0118341356514375));
#15829=CARTESIAN_POINT('Ctrl Pts',(0.00251750000000004,-0.0131895738352092,
-0.0120050524791417));
#15830=CARTESIAN_POINT('Ctrl Pts',(0.0025175,-0.0131787743898827,-0.0121758532865587));
#15831=CARTESIAN_POINT('',(0.00178084802570376,-0.013178793072307,-0.0139565263307246));
#15832=CARTESIAN_POINT('Origin',(0.,-0.0131787743898824,-0.012175853286568));
#15833=CARTESIAN_POINT('',(0.00251749951162147,-0.0133037004643823,-0.0121747621479011));
#15834=CARTESIAN_POINT('Ctrl Pts',(0.00178027729478665,-0.0131787974308209,
-0.0139558586246588));
#15835=CARTESIAN_POINT('Ctrl Pts',(0.00213502811265273,-0.0132107157510099,
-0.013601053606474));
#15836=CARTESIAN_POINT('Ctrl Pts',(0.00237986623540055,-0.0132435981229686,
-0.013138028295549));
#15837=CARTESIAN_POINT('Ctrl Pts',(0.00247338372893183,-0.0132748262662687,
-0.0126450858296061));
#15838=CARTESIAN_POINT('Ctrl Pts',(0.00250270547493553,-0.0132846176288409,
-0.0124905272199275));
#15839=CARTESIAN_POINT('Ctrl Pts',(0.00251750034288861,-0.0132942463656009,
-0.0123332009389632));
#15840=CARTESIAN_POINT('Ctrl Pts',(0.00251749999999402,-0.0133036317703176,
-0.0121758478005721));
#15841=CARTESIAN_POINT('',(0.0025174998365065,-0.0143038157113684,-0.0121764859784127));
#15842=CARTESIAN_POINT('Ctrl Pts',(0.00251749898605663,-0.0133037743898821,
-0.0121735938167424));
#15843=CARTESIAN_POINT('Ctrl Pts',(0.00251706083443314,-0.0133346442943258,
-0.0116854057204819));
#15844=CARTESIAN_POINT('Ctrl Pts',(0.00237033506334122,-0.0133655141987695,
-0.0111973681052421));
#15845=CARTESIAN_POINT('Ctrl Pts',(0.00210171129165819,-0.0133963841032132,
-0.0107899904158106));
#15846=CARTESIAN_POINT('Ctrl Pts',(0.00200776001313763,-0.0134071808654362,
-0.010647509895479));
#15847=CARTESIAN_POINT('Ctrl Pts',(0.00189935103424433,-0.0134179776276591,
-0.0105147488285564));
#15848=CARTESIAN_POINT('Ctrl Pts',(0.00177885628403369,-0.0134287743898821,
-0.0103944278542837));
#15849=CARTESIAN_POINT('Ctrl Pts',(0.0014406856893849,-0.0134590756892734,
-0.0100567449648021));
#15850=CARTESIAN_POINT('Ctrl Pts',(0.0010019861077406,-0.0134893769886648,
-0.00981709907992996));
#15851=CARTESIAN_POINT('Ctrl Pts',(0.000533402069157638,-0.0135196782880561,
-0.00971551012296925));
#15852=CARTESIAN_POINT('Ctrl Pts',(0.000357646249941188,-0.0135310436553314,
-0.00967740628484457));
#15853=CARTESIAN_POINT('Ctrl Pts',(0.000177953861841114,-0.0135424090226068,
-0.00965825579838605));
#15854=CARTESIAN_POINT('Ctrl Pts',(-1.37385441371961E-6,-0.0135537743898821,
-0.00965835366142921));
#15855=CARTESIAN_POINT('Ctrl Pts',(-0.00048124901856916,-0.0135841877448327,
-0.00965861553976505));
#15856=CARTESIAN_POINT('Ctrl Pts',(-0.000962587104117076,-0.0136146010997832,
-0.00980040445547009));
#15857=CARTESIAN_POINT('Ctrl Pts',(-0.0013666812162148,-0.0136450144547338,
-0.0100616185069639));
#15858=CARTESIAN_POINT('Ctrl Pts',(-0.00151620095888938,-0.0136562677664499,
-0.0101582708871721));
#15859=CARTESIAN_POINT('Ctrl Pts',(-0.00165528817767921,-0.013667521078166,
-0.0102707661943849));
#15860=CARTESIAN_POINT('Ctrl Pts',(-0.00178079954929275,-0.0136787743898821,
-0.0103963704360538));
#15861=CARTESIAN_POINT('Ctrl Pts',(-0.00211994448965385,-0.0137091820229257,
-0.0107357663210824));
#15862=CARTESIAN_POINT('Ctrl Pts',(-0.00236009283512154,-0.0137395896559693,
-0.011176254544861));
#15863=CARTESIAN_POINT('Ctrl Pts',(-0.00246123332061233,-0.0137699972890129,
-0.0116465737843028));
#15864=CARTESIAN_POINT('Ctrl Pts',(-0.00249868260596648,-0.0137812563226359,
-0.0118207188788209));
#15865=CARTESIAN_POINT('Ctrl Pts',(-0.00251753440491855,-0.013792515356259,
-0.0119986957463653));
#15866=CARTESIAN_POINT('Ctrl Pts',(-0.00251749995265597,-0.0138037743898821,
-0.0121763415253998));
#15867=CARTESIAN_POINT('Ctrl Pts',(-0.00251740690632599,-0.0138341820229257,
-0.0126561151757386));
#15868=CARTESIAN_POINT('Ctrl Pts',(-0.00237584506952176,-0.0138645896559693,
-0.0131374187103319));
#15869=CARTESIAN_POINT('Ctrl Pts',(-0.00211486410742613,-0.0138949972890129,
-0.013541560450309));
#15870=CARTESIAN_POINT('Ctrl Pts',(-0.00201823069228971,-0.0139062563226359,
-0.0136912020035456));
#15871=CARTESIAN_POINT('Ctrl Pts',(-0.00190573312061065,-0.013917515356259,
-0.0138304073426009));
#15872=CARTESIAN_POINT('Ctrl Pts',(-0.00178010919676054,-0.0139287743898821,
-0.0139560267324921));
#15873=CARTESIAN_POINT('Ctrl Pts',(-0.00144076879560054,-0.0139591877448326,
-0.0142953548863397));
#15874=CARTESIAN_POINT('Ctrl Pts',(-0.00100027024108851,-0.0139896010997831,
-0.0145356802908132));
#15875=CARTESIAN_POINT('Ctrl Pts',(-0.000529886334566621,-0.0140200144547337,
-0.0146369560317598));
#15876=CARTESIAN_POINT('Ctrl Pts',(-0.000355838560653692,-0.0140312677664498,
-0.0146744292892815));
#15877=CARTESIAN_POINT('Ctrl Pts',(-0.000177957055843198,-0.0140425210781659,
-0.0146933252281468));
#15878=CARTESIAN_POINT('Ctrl Pts',(-3.97376790599182E-7,-0.0140537743898821,
-0.014693353255196));
#15879=CARTESIAN_POINT('Ctrl Pts',(0.000477709791170785,-0.0140840756892734,
-0.0146934287224032));
#15880=CARTESIAN_POINT('Ctrl Pts',(0.000957528083984738,-0.0141143769886648,
-0.0145529833977446));
#15881=CARTESIAN_POINT('Ctrl Pts',(0.00136083300869463,-0.0141446782880562,
-0.0142938570099843));
#15882=CARTESIAN_POINT('Ctrl Pts',(0.00151210403288667,-0.0141560436553315,
-0.0141966642615945));
#15883=CARTESIAN_POINT('Ctrl Pts',(0.00165275572478575,-0.0141674090226068,
-0.0140832954048709));
#15884=CARTESIAN_POINT('Ctrl Pts',(0.00177954712227563,-0.0141787743898821,
-0.0139565886092831));
#15885=CARTESIAN_POINT('Ctrl Pts',(0.00212393003837453,-0.0142096442943259,
-0.0136124354836143));
#15886=CARTESIAN_POINT('Ctrl Pts',(0.0023662286154867,-0.0142405141987698,
-0.013164541615454));
#15887=CARTESIAN_POINT('Ctrl Pts',(0.00246525451638777,-0.0142713841032136,
-0.0126860752181033));
#15888=CARTESIAN_POINT('Ctrl Pts',(0.00249988886739057,-0.0142821808654364,
-0.0125187313919113));
#15889=CARTESIAN_POINT('Ctrl Pts',(0.00251741265685568,-0.0142929776276592,
-0.0123478803200529));
#15890=CARTESIAN_POINT('Ctrl Pts',(0.00251749967307457,-0.0143037743898821,
-0.0121771362789318));
#15891=CARTESIAN_POINT('',(0.00251749973816877,-0.0153038253093176,-0.0121766683770049));
#15892=CARTESIAN_POINT('Ctrl Pts',(0.00251749999993842,-0.0143038570328546,
-0.0121758356778936));
#15893=CARTESIAN_POINT('Ctrl Pts',(0.0025174965853186,-0.0143347205377646,
-0.0116876495701149));
#15894=CARTESIAN_POINT('Ctrl Pts',(0.002371206713351,-0.0143655840426746,
-0.011199483304505));
#15895=CARTESIAN_POINT('Ctrl Pts',(0.00210294789098424,-0.0143964475475845,
-0.0107918675865579));
#15896=CARTESIAN_POINT('Ctrl Pts',(0.00200907910578422,-0.014407247265884,
-0.0106492352140807));
#15897=CARTESIAN_POINT('Ctrl Pts',(0.0019007301047126,-0.0144180469841836,
-0.0105163187080229));
#15898=CARTESIAN_POINT('Ctrl Pts',(0.00178027394343148,-0.014428846702483,
-0.0103958445965965));
#15899=CARTESIAN_POINT('Ctrl Pts',(0.00144237569619611,-0.0144591415902266,
-0.0100578959964145));
#15900=CARTESIAN_POINT('Ctrl Pts',(0.0010038716150532,-0.0144894364779702,
-0.00981790169375985));
#15901=CARTESIAN_POINT('Ctrl Pts',(0.000535372809709038,-0.0145197313657138,
-0.0097159382057831));
#15902=CARTESIAN_POINT('Ctrl Pts',(0.000359565867310013,-0.0145310997011797,
-0.00967767580499775));
#15903=CARTESIAN_POINT('Ctrl Pts',(0.000179803488936402,-0.0145424680366456,
-0.00965838130553472));
#15904=CARTESIAN_POINT('Ctrl Pts',(3.92733717786047E-7,-0.0145538363721115,
-0.00965835331719161));
#15905=CARTESIAN_POINT('Ctrl Pts',(-0.000479477977530979,-0.0145842433074097,
-0.00965827845665108));
#15906=CARTESIAN_POINT('Ctrl Pts',(-0.000960911889368447,-0.0146146502427079,
-0.0097997270328723));
#15907=CARTESIAN_POINT('Ctrl Pts',(-0.00136518740714128,-0.014645057178006,
-0.0100606536285157));
#15908=CARTESIAN_POINT('Ctrl Pts',(-0.00151484542360727,-0.0146563134659173,
-0.0101572455689882));
#15909=CARTESIAN_POINT('Ctrl Pts',(-0.00165407229727665,-0.0146675697538286,
-0.0102697027086086));
#15910=CARTESIAN_POINT('Ctrl Pts',(-0.00177971848881848,-0.0146788260417399,
-0.010395289232513));
#15911=CARTESIAN_POINT('Ctrl Pts',(-0.00211906638382967,-0.0147092272625128,
-0.0107344759759053));
#15912=CARTESIAN_POINT('Ctrl Pts',(-0.00235948150774078,-0.0147396284832857,
-0.0111748140816622));
#15913=CARTESIAN_POINT('Ctrl Pts',(-0.00246090901105393,-0.0147700297040585,
-0.0116450679351084));
#15914=CARTESIAN_POINT('Ctrl Pts',(-0.00249848239660917,-0.0147812917064951,
-0.0118192714673577));
#15915=CARTESIAN_POINT('Ctrl Pts',(-0.00251744317698114,-0.0147925537089318,
-0.0119973217499119));
#15916=CARTESIAN_POINT('Ctrl Pts',(-0.00251749987191038,-0.0148038157113684,
-0.0121750502104685));
#15917=CARTESIAN_POINT('Ctrl Pts',(-0.0025176529170789,-0.0148342169321413,
-0.0126548194342313));
#15918=CARTESIAN_POINT('Ctrl Pts',(-0.00237634045289419,-0.0148646181529143,
-0.0131361920566667));
#15919=CARTESIAN_POINT('Ctrl Pts',(-0.0021155705531048,-0.0148950193736872,
-0.0135404658633856));
#15920=CARTESIAN_POINT('Ctrl Pts',(-0.00201896945709177,-0.0149062813761238,
-0.013690227369027));
#15921=CARTESIAN_POINT('Ctrl Pts',(-0.00190648390638609,-0.0149175433785602,
-0.0138295510692772));
#15922=CARTESIAN_POINT('Ctrl Pts',(-0.00178085411735329,-0.0149288053809968,
-0.0139552815269505));
#15923=CARTESIAN_POINT('Ctrl Pts',(-0.00144165894418808,-0.014959212316295,
-0.0142947485012323));
#15924=CARTESIAN_POINT('Ctrl Pts',(-0.00100126530635152,-0.0149896192515932,
-0.0145352575277486));
#15925=CARTESIAN_POINT('Ctrl Pts',(-0.000530927814105084,-0.0150200261868913,
-0.0146367315659961));
#15926=CARTESIAN_POINT('Ctrl Pts',(-0.000356814435815436,-0.0150312824748026,
-0.0146742960551113));
#15927=CARTESIAN_POINT('Ctrl Pts',(-0.000178855863209009,-0.0150425387627139,
-0.0146932673716284));
#15928=CARTESIAN_POINT('Ctrl Pts',(-1.21341844005783E-6,-0.0150537950506252,
-0.0146933529941282));
#15929=CARTESIAN_POINT('Ctrl Pts',(0.000476888951114326,-0.0150840899383688,
-0.0146935834363522));
#15930=CARTESIAN_POINT('Ctrl Pts',(0.000956749001387523,-0.0151143848261125,
-0.0145532963079935));
#15931=CARTESIAN_POINT('Ctrl Pts',(0.00136013598984903,-0.0151446797138561,
-0.0142943046877277));
#15932=CARTESIAN_POINT('Ctrl Pts',(0.00151150933858718,-0.015156048049322,
-0.0141971165533154));
#15933=CARTESIAN_POINT('Ctrl Pts',(0.0016522587497757,-0.0151674163847878,
-0.0140837337046568));
#15934=CARTESIAN_POINT('Ctrl Pts',(0.00177913794469099,-0.0151787847202537,
-0.0139569974199063));
#15935=CARTESIAN_POINT('Ctrl Pts',(0.0021235979289153,-0.0152096482251635,
-0.0136129254175978));
#15936=CARTESIAN_POINT('Ctrl Pts',(0.00236599908946475,-0.0152405117300734,
-0.0131650898075971));
#15937=CARTESIAN_POINT('Ctrl Pts',(0.00246513583155777,-0.0152713752349833,
-0.0126866483354475));
#15938=CARTESIAN_POINT('Ctrl Pts',(0.00249982563399178,-0.0152821749532829,
-0.012519232705332));
#15939=CARTESIAN_POINT('Ctrl Pts',(0.00251738929573821,-0.0152929746715825,
-0.0123483024723817));
#15940=CARTESIAN_POINT('Ctrl Pts',(0.00251749947634573,-0.0153037743898821,
-0.0121774770473163));
#15941=CARTESIAN_POINT('',(0.00251749964728232,-0.0163037152489246,-0.0121749072438898));
#15942=CARTESIAN_POINT('Ctrl Pts',(0.00251749999999181,-0.0153038762287532,
-0.0121758597066935));
#15943=CARTESIAN_POINT('Ctrl Pts',(0.00251750124987346,-0.015334773828238,
-0.0116857490092181));
#15944=CARTESIAN_POINT('Ctrl Pts',(0.00237009877551313,-0.0153656931543452,
-0.0111958220961543));
#15945=CARTESIAN_POINT('Ctrl Pts',(0.00209985358181042,-0.0153966188415361,
-0.0107871772318362));
#15946=CARTESIAN_POINT('Ctrl Pts',(0.00200668698258001,-0.0154072804228392,
-0.0106462975670405));
#15947=CARTESIAN_POINT('Ctrl Pts',(0.0018993619470655,-0.0154179427601664,
-0.0105149344514446));
#15948=CARTESIAN_POINT('Ctrl Pts',(0.00178015521674487,-0.0154286052239324,
-0.0103957258601372));
#15949=CARTESIAN_POINT('Ctrl Pts',(0.0014437994054449,-0.0154586906196211,
-0.010059364797844));
#15950=CARTESIAN_POINT('Ctrl Pts',(0.00100771648424144,-0.0154887770219555,
-0.0098200625804111));
#15951=CARTESIAN_POINT('Ctrl Pts',(0.000541997348581827,-0.0155189068606704,
-0.00971738930998039));
#15952=CARTESIAN_POINT('Ctrl Pts',(0.000363889698180644,-0.015530429588361,
-0.00967812338003418));
#15953=CARTESIAN_POINT('Ctrl Pts',(0.000181723932839053,-0.015541958668931,
-0.00965835423216842));
#15954=CARTESIAN_POINT('Ctrl Pts',(1.31004198167687E-8,-0.015553496475643,
-0.00965835328659218));
#15955=CARTESIAN_POINT('Ctrl Pts',(-0.000471589952940902,-0.0155834411124158,
-0.00965835083249169));
#15956=CARTESIAN_POINT('Ctrl Pts',(-0.000945830025214709,-0.0156134445270603,
-0.00979520887204593));
#15957=CARTESIAN_POINT('Ctrl Pts',(-0.00134601620199894,-0.0156433545931743,
-0.0100484025505935));
#15958=CARTESIAN_POINT('Ctrl Pts',(-0.0015032117943325,-0.0156551034511616,
-0.0101478585852677));
#15959=CARTESIAN_POINT('Ctrl Pts',(-0.00164912550741972,-0.0156668379057812,
-0.0102646968324588));
#15960=CARTESIAN_POINT('Ctrl Pts',(-0.00178013668995606,-0.0156785487368522,
-0.0103957073332519));
#15961=CARTESIAN_POINT('Ctrl Pts',(-0.00201240543112207,-0.0156993107812687,
-0.0106279748657605));
#15962=CARTESIAN_POINT('Ctrl Pts',(-0.00219837348351843,-0.0157199985733812,
-0.0109046529700258));
#15963=CARTESIAN_POINT('Ctrl Pts',(-0.00232586546977604,-0.0157411352460187,
-0.0112124447197997));
#15964=CARTESIAN_POINT('Ctrl Pts',(-0.00244671118957433,-0.0157611700458049,
-0.0115041910219888));
#15965=CARTESIAN_POINT('Ctrl Pts',(-0.00251113007154686,-0.015781608144953,
-0.0118262264809469));
#15966=CARTESIAN_POINT('Ctrl Pts',(-0.00251701645338492,-0.015800635682678,
-0.0121265134102956));
#15967=CARTESIAN_POINT('Ctrl Pts',(-0.00251734019229965,-0.0158016821581841,
-0.0121430285748379));
#15968=CARTESIAN_POINT('Ctrl Pts',(-0.0025175,-0.0158027243670605,-0.0121594779400862));
#15969=CARTESIAN_POINT('Ctrl Pts',(-0.0025175,-0.0158037620075599,-0.0121758532865581));
#15970=CARTESIAN_POINT('Ctrl Pts',(-0.0025175,-0.015823666543301,-0.0124899733207367));
#15971=CARTESIAN_POINT('Ctrl Pts',(-0.0024630951558248,-0.0158418900616207,
-0.0127769085051407));
#15972=CARTESIAN_POINT('Ctrl Pts',(-0.00235775854945272,-0.0158608768294718,
-0.0130583389082441));
#15973=CARTESIAN_POINT('Ctrl Pts',(-0.00225242194308064,-0.0158798635973229,
-0.0133397693113476));
#15974=CARTESIAN_POINT('Ctrl Pts',(-0.00209100657981397,-0.0158996136147054,
-0.0136125856001859));
#15975=CARTESIAN_POINT('Ctrl Pts',(-0.0018823955451073,-0.0159195265353501,
-0.0138474971666235));
#15976=CARTESIAN_POINT('Ctrl Pts',(-0.00155812287986674,-0.0159504799116144,
-0.0142126523457428));
#15977=CARTESIAN_POINT('Ctrl Pts',(-0.00111876532461567,-0.0159818269067479,
-0.0144870957714781));
#15978=CARTESIAN_POINT('Ctrl Pts',(-0.000629171305823964,-0.0160137889809416,
-0.0146134647646095));
#15979=CARTESIAN_POINT('Ctrl Pts',(-0.00048883424627106,-0.0160229505787908,
-0.0146496871289236));
#15980=CARTESIAN_POINT('Ctrl Pts',(-0.000344620800036344,-0.0160321627129445,
-0.014673952015472));
#15981=CARTESIAN_POINT('Ctrl Pts',(-0.000198603736845032,-0.016041430599005,
-0.0146855072080603));
#15982=CARTESIAN_POINT('Ctrl Pts',(0.000259338701600219,-0.0160704967796899,
-0.0147217468978262));
#15983=CARTESIAN_POINT('Ctrl Pts',(0.000738899690729382,-0.0161001113311382,
-0.0146292770516161));
#15984=CARTESIAN_POINT('Ctrl Pts',(0.00116198117812939,-0.0161302303745341,
-0.0144091481599846));
#15985=CARTESIAN_POINT('Ctrl Pts',(0.0013444321136084,-0.0161432190015645,
-0.0143142191134528));
#15986=CARTESIAN_POINT('Ctrl Pts',(0.00151628576184183,-0.016156301449233,
-0.0141962146500593));
#15987=CARTESIAN_POINT('Ctrl Pts',(0.00167165393585948,-0.0161694741985248,
-0.0140582399016628));
#15988=CARTESIAN_POINT('Ctrl Pts',(0.00202224925129645,-0.0161991991033988,
-0.0137468936382325));
#15989=CARTESIAN_POINT('Ctrl Pts',(0.00229094624963296,-0.01622938382382,
-0.0133274201072613));
#15990=CARTESIAN_POINT('Ctrl Pts',(0.00242300216787857,-0.0162600418379914,
-0.0128591297638758));
#15991=CARTESIAN_POINT('Ctrl Pts',(0.0024851695147177,-0.0162744745678965,
-0.0126386749097094));
#15992=CARTESIAN_POINT('Ctrl Pts',(0.00251750068801699,-0.0162890121891569,
-0.0124080172334331));
#15993=CARTESIAN_POINT('Ctrl Pts',(0.00251749999998895,-0.016303656107967,
-0.0121758458260761));
#15994=CARTESIAN_POINT('',(0.00251749991915687,-0.0173037452241442,-0.0121754098665498));
#15995=CARTESIAN_POINT('Ctrl Pts',(0.0025174992945757,-0.0163037743898821,
-0.0121739686617036));
#15996=CARTESIAN_POINT('Ctrl Pts',(0.00251713383351018,-0.0163346391685405,
-0.0116857823935164));
#15997=CARTESIAN_POINT('Ctrl Pts',(0.00237048180168344,-0.0163655039471989,
-0.0111977245059383));
#15998=CARTESIAN_POINT('Ctrl Pts',(0.00210192047764992,-0.0163963687258573,
-0.0107903077060607));
#15999=CARTESIAN_POINT('Ctrl Pts',(0.00200795198867354,-0.0164071681833874,
-0.0106477542642877));
#16000=CARTESIAN_POINT('Ctrl Pts',(0.00189951237851906,-0.0164179676409175,
-0.0105149261596554));
#16001=CARTESIAN_POINT('Ctrl Pts',(0.00177897624077857,-0.0164287670984476,
-0.0103945476460951));
#16002=CARTESIAN_POINT('Ctrl Pts',(0.00144083133054195,-0.016459063254153,
-0.0100568449253566));
#16003=CARTESIAN_POINT('Ctrl Pts',(0.00100215184109577,-0.0164893594098584,
-0.00981717015499711));
#16004=CARTESIAN_POINT('Ctrl Pts',(0.000533578279319637,-0.0165196555655639,
-0.00971554833191562));
#16005=CARTESIAN_POINT('Ctrl Pts',(0.000357754586890734,-0.016531023646047,
-0.00967741659418416));
#16006=CARTESIAN_POINT('Ctrl Pts',(0.000177989795265128,-0.0165423917265301,
-0.00965825322864707));
#16007=CARTESIAN_POINT('Ctrl Pts',(-1.40964375676471E-6,-0.0165537598070132,
-0.00965835368121463));
#16008=CARTESIAN_POINT('Ctrl Pts',(-0.000481280900188044,-0.0165841680128269,
-0.00965862237937818));
#16009=CARTESIAN_POINT('Ctrl Pts',(-0.000962613902861325,-0.0166145762186406,
-0.00980041594245372));
#16010=CARTESIAN_POINT('Ctrl Pts',(-0.00136670275312918,-0.0166449844244543,
-0.0100616324289869));
#16011=CARTESIAN_POINT('Ctrl Pts',(-0.00151628199501565,-0.0166562404548291,
-0.0101583254310283));
#16012=CARTESIAN_POINT('Ctrl Pts',(-0.00165542006449945,-0.0166674964852039,
-0.0102708741266331));
#16013=CARTESIAN_POINT('Ctrl Pts',(-0.00178096996615074,-0.0166787525155787,
-0.010396540995343));
#16014=CARTESIAN_POINT('Ctrl Pts',(-0.00212007971698423,-0.0167091550057883,
-0.0107359666737049));
#16015=CARTESIAN_POINT('Ctrl Pts',(-0.00236018527371475,-0.0167395574959981,
-0.0111764742764784));
#16016=CARTESIAN_POINT('Ctrl Pts',(-0.00246128192528678,-0.0167699599862077,
-0.0116467998542314));
#16017=CARTESIAN_POINT('Ctrl Pts',(-0.002498730331699,-0.0167812217321866,
-0.0118210187141826));
#16018=CARTESIAN_POINT('Ctrl Pts',(-0.00251756580689056,-0.0167924834781653,
-0.0119990707375693));
#16019=CARTESIAN_POINT('Ctrl Pts',(-0.00251749982649569,-0.0168037452241442,
-0.012176787949167));
#16020=CARTESIAN_POINT('Ctrl Pts',(-0.00251732170417675,-0.016834147714354,
-0.0126565577642434));
#16021=CARTESIAN_POINT('Ctrl Pts',(-0.00237567666252507,-0.0168645502045637,
-0.0131378331996337));
#16022=CARTESIAN_POINT('Ctrl Pts',(-0.00211462726198308,-0.0168949526947735,
-0.0135419271472545));
#16023=CARTESIAN_POINT('Ctrl Pts',(-0.00201792886601202,-0.0169062144407522,
-0.0136916123657435));
#16024=CARTESIAN_POINT('Ctrl Pts',(-0.00190535525634474,-0.016917476186731,
-0.0138308501418363));
#16025=CARTESIAN_POINT('Ctrl Pts',(-0.00177964827831328,-0.0169287379327098,
-0.0139564875149993));
#16026=CARTESIAN_POINT('Ctrl Pts',(-0.0014402227871498,-0.0169591461385235,
-0.0142957250637988));
#16027=CARTESIAN_POINT('Ctrl Pts',(-0.000999665739556573,-0.0169895543443372,
-0.0145359357992138));
#16028=CARTESIAN_POINT('Ctrl Pts',(-0.000529259072253469,-0.0170199625501508,
-0.0146370910004812));
#16029=CARTESIAN_POINT('Ctrl Pts',(-0.000355131346068953,-0.0170312185805257,
-0.014674535038614));
#16030=CARTESIAN_POINT('Ctrl Pts',(-0.000177171522077231,-0.0170424746109005,
-0.0146933856790558));
#16031=CARTESIAN_POINT('Ctrl Pts',(4.59681427768803E-7,-0.0170537306412753,
-0.0146933532445905));
#16032=CARTESIAN_POINT('Ctrl Pts',(0.000478562744435762,-0.0170840267969807,
-0.0146932659456422));
#16033=CARTESIAN_POINT('Ctrl Pts',(0.000958329964371957,-0.017114322952686,
-0.014552659577419));
#16034=CARTESIAN_POINT('Ctrl Pts',(0.00136154500052124,-0.0171446191083914,
-0.0142933993808747));
#16035=CARTESIAN_POINT('Ctrl Pts',(0.00151284409693271,-0.0171559871888745,
-0.0141961167154086));
#16036=CARTESIAN_POINT('Ctrl Pts',(0.00165350983650716,-0.0171673552693577,
-0.0140826484617815));
#16037=CARTESIAN_POINT('Ctrl Pts',(0.00178029842734652,-0.0171787233498408,
-0.0139558374886193));
#16038=CARTESIAN_POINT('Ctrl Pts',(0.00212453436044685,-0.0172095881284993,
-0.0136115407866458));
#16039=CARTESIAN_POINT('Ctrl Pts',(0.00236664363537164,-0.0172404529071577,
-0.0131635469362518));
#16040=CARTESIAN_POINT('Ctrl Pts',(0.00246546840766923,-0.0172713176858162,
-0.0126850406595211));
#16041=CARTESIAN_POINT('Ctrl Pts',(0.00250004678398457,-0.0172821171433462,
-0.0125176133058185));
#16042=CARTESIAN_POINT('Ctrl Pts',(0.00251749896185189,-0.0172929166008763,
-0.0123466829765938));
#16043=CARTESIAN_POINT('Ctrl Pts',(0.00251749999995351,-0.0173037160584063,
-0.0121758685863278));
#16044=CARTESIAN_POINT('',(0.00251749947371737,-0.018303848443002,-0.0121770002512912));
#16045=CARTESIAN_POINT('Ctrl Pts',(0.00251749983836023,-0.0173037743898821,
-0.0121749511467718));
#16046=CARTESIAN_POINT('Ctrl Pts',(0.00251732489744756,-0.0173346436410567,
-0.0116867632560798));
#16047=CARTESIAN_POINT('Ctrl Pts',(0.00237086248730374,-0.0173655128922312,
-0.0111986469117092));
#16048=CARTESIAN_POINT('Ctrl Pts',(0.00210245874673254,-0.0173963821434057,
-0.0107911246242246));
#16049=CARTESIAN_POINT('Ctrl Pts',(0.00200857675749333,-0.0174071795588979,
-0.0106485818901817));
#16050=CARTESIAN_POINT('Ctrl Pts',(0.00190022947733341,-0.01741797697439,
-0.0105157523906493));
#16051=CARTESIAN_POINT('Ctrl Pts',(0.00177978797063945,-0.0174287743898821,
-0.0103953586840481));
#16052=CARTESIAN_POINT('Ctrl Pts',(0.00144179465482541,-0.0174590750259716,
-0.0100574995089659));
#16053=CARTESIAN_POINT('Ctrl Pts',(0.0010032212774398,-0.0174893756620611,
-0.00981762428598563));
#16054=CARTESIAN_POINT('Ctrl Pts',(0.000534691162055855,-0.0175196762981507,
-0.00971578995175971));
#16055=CARTESIAN_POINT('Ctrl Pts',(0.000358941464853777,-0.0175310423287278,
-0.0096775910125297));
#16056=CARTESIAN_POINT('Ctrl Pts',(0.000179244643635947,-0.0175424083593049,
-0.00965834636490786));
#16057=CARTESIAN_POINT('Ctrl Pts',(-9.71885758251945E-8,-0.0175537743898821,
-0.00965835328843409));
#16058=CARTESIAN_POINT('Ctrl Pts',(-0.000479971656978348,-0.0175841870817443,
-0.00965837181408103));
#16059=CARTESIAN_POINT('Ctrl Pts',(-0.000961380981430865,-0.0176145997736064,
-0.00979991618612311));
#16060=CARTESIAN_POINT('Ctrl Pts',(-0.00136560720305024,-0.0176450124654686,
-0.0100609246312656));
#16061=CARTESIAN_POINT('Ctrl Pts',(-0.0015151879022545,-0.0176562664402731,
-0.0101575087310457));
#16062=CARTESIAN_POINT('Ctrl Pts',(-0.00165434246006101,-0.0176675204150776,
-0.0102699435837089));
#16063=CARTESIAN_POINT('Ctrl Pts',(-0.00177992543801329,-0.0176787743898821,
-0.0103954961074749));
#16064=CARTESIAN_POINT('Ctrl Pts',(-0.00211923648598154,-0.0177091813610098,
-0.0107347248716651));
#16065=CARTESIAN_POINT('Ctrl Pts',(-0.0023596010059073,-0.0177395883321375,
-0.011175094395759));
#16066=CARTESIAN_POINT('Ctrl Pts',(-0.00246097268831098,-0.0177699953032652,
-0.0116453632514138));
#16067=CARTESIAN_POINT('Ctrl Pts',(-0.00249851060273674,-0.0177812549988042,
-0.0118195037178842));
#16068=CARTESIAN_POINT('Ctrl Pts',(-0.00251744995374564,-0.0177925146943431,
-0.0119974857147075));
#16069=CARTESIAN_POINT('Ctrl Pts',(-0.00251749990051083,-0.0178037743898821,
-0.0121751455239136));
#16070=CARTESIAN_POINT('Ctrl Pts',(-0.0025176347824747,-0.0178341813610099,
-0.0126549184156753));
#16071=CARTESIAN_POINT('Ctrl Pts',(-0.00237630203724782,-0.0178645883321375,
-0.0131362885610932));
#16072=CARTESIAN_POINT('Ctrl Pts',(-0.00211551373521293,-0.0178949953032653,
-0.013540553944624));
#16073=CARTESIAN_POINT('Ctrl Pts',(-0.00201894387731103,-0.0179062549988042,
-0.0136902533381075));
#16074=CARTESIAN_POINT('Ctrl Pts',(-0.00190650237038634,-0.0179175146943432,
-0.0138295224041051));
#16075=CARTESIAN_POINT('Ctrl Pts',(-0.00178092620551187,-0.0179287743898821,
-0.0139552093781039));
#16076=CARTESIAN_POINT('Ctrl Pts',(-0.00144174214903808,-0.0179591870817443,
-0.0142946927325241));
#16077=CARTESIAN_POINT('Ctrl Pts',(-0.00100135469175334,-0.0179895997736064,
-0.014535220201561));
#16078=CARTESIAN_POINT('Ctrl Pts',(-0.000531018002186749,-0.0180200124654686,
-0.0146367121064325));
#16079=CARTESIAN_POINT('Ctrl Pts',(-0.000356973649979874,-0.0180312664402731,
-0.0146742683788421));
#16080=CARTESIAN_POINT('Ctrl Pts',(-0.000179086413295556,-0.0180425204150776,
-0.0146932461316884));
#16081=CARTESIAN_POINT('Ctrl Pts',(-1.5127137924576E-6,-0.0180537743898821,
-0.0146933528320788));
#16082=CARTESIAN_POINT('Ctrl Pts',(0.000476593567870745,-0.0180840750259716,
-0.0146936401163279));
#16083=CARTESIAN_POINT('Ctrl Pts',(0.00095647340039854,-0.0181143756620611,
-0.014553407831921));
#16084=CARTESIAN_POINT('Ctrl Pts',(0.00135989276293095,-0.0181446762981507,
-0.014294460830047));
#16085=CARTESIAN_POINT('Ctrl Pts',(0.00151121885378951,-0.0181560423287278,
-0.0141973275707826));
#16086=CARTESIAN_POINT('Ctrl Pts',(0.00165193110895003,-0.0181674083593049,
-0.0140840109266131));
#16087=CARTESIAN_POINT('Ctrl Pts',(0.00177878656316556,-0.0181787743898821,
-0.0139573483364254));
#16088=CARTESIAN_POINT('Ctrl Pts',(0.00212331606732685,-0.0182096436410565,
-0.0136133426358977));
#16089=CARTESIAN_POINT('Ctrl Pts',(0.00236580582515884,-0.0182405128922309,
-0.0131655527105787));
#16090=CARTESIAN_POINT('Ctrl Pts',(0.00246503618344002,-0.0182713821434054,
-0.0126871290089735));
#16091=CARTESIAN_POINT('Ctrl Pts',(0.00249974487791892,-0.0182821795588976,
-0.012519786449921));
#16092=CARTESIAN_POINT('Ctrl Pts',(0.00251734172976889,-0.0182929769743899,
-0.0123489287571923));
#16093=CARTESIAN_POINT('Ctrl Pts',(0.00251749893315368,-0.0183037743898821,
-0.0121781709513438));
#16094=CARTESIAN_POINT('',(0.00251749999999994,-0.0193037658457995,-0.0121758527464904));
#16095=CARTESIAN_POINT('Ctrl Pts',(0.00251749999998966,-0.0183039205383097,
-0.0121758605021413));
#16096=CARTESIAN_POINT('Ctrl Pts',(0.00251750139920864,-0.0183347784818584,
-0.0116876762924853));
#16097=CARTESIAN_POINT('Ctrl Pts',(0.00237121741640988,-0.0183656364254071,
-0.0111995101627397));
#16098=CARTESIAN_POINT('Ctrl Pts',(0.00210296441023168,-0.0183964943689557,
-0.0107918926876612));
#16099=CARTESIAN_POINT('Ctrl Pts',(0.00200905844461261,-0.0184072966523197,
-0.0106492001111798));
#16100=CARTESIAN_POINT('Ctrl Pts',(0.0019006601175944,-0.0184180989356836,
-0.0105162313326969));
#16101=CARTESIAN_POINT('Ctrl Pts',(0.00178014554476341,-0.0184289012190475,
-0.0103957161880573));
#16102=CARTESIAN_POINT('Ctrl Pts',(0.00144222588007803,-0.0184591905349901,
-0.0100577949200357));
#16103=CARTESIAN_POINT('Ctrl Pts',(0.00100370846356905,-0.0184894798509328,
-0.00981783290983037));
#16104=CARTESIAN_POINT('Ctrl Pts',(0.000535205959966458,-0.0185197691668754,
-0.0097159018987424));
#16105=CARTESIAN_POINT('Ctrl Pts',(0.000359325452537379,-0.0185311400778453,
-0.00967763598166606));
#16106=CARTESIAN_POINT('Ctrl Pts',(0.000179487594139983,-0.0185425109888153,
-0.0096583536237291));
#16107=CARTESIAN_POINT('Ctrl Pts',(4.72923594120771E-9,-0.0185538818997853,
-0.00965835328656254));
#16108=CARTESIAN_POINT('Ctrl Pts',(-0.00047986206250833,-0.0185842832563119,
-0.00965835238511138));
#16109=CARTESIAN_POINT('Ctrl Pts',(-0.000961271083096095,-0.0186146846128386,
-0.00979987295396124));
#16110=CARTESIAN_POINT('Ctrl Pts',(-0.00136550482274316,-0.0186450859693652,
-0.0100608585279203));
#16111=CARTESIAN_POINT('Ctrl Pts',(-0.00151520917150609,-0.0186563448397512,
-0.0101575122001749));
#16112=CARTESIAN_POINT('Ctrl Pts',(-0.00165447146738626,-0.0186676037101371,
-0.0102700424587043));
#16113=CARTESIAN_POINT('Ctrl Pts',(-0.00178013885661713,-0.0186788625805231,
-0.0103957094999044));
#16114=CARTESIAN_POINT('Ctrl Pts',(-0.00211940395598334,-0.0187092582289377,
-0.0107349736596895));
#16115=CARTESIAN_POINT('Ctrl Pts',(-0.00235971449685064,-0.0187396538773524,
-0.0111753648807987));
#16116=CARTESIAN_POINT('Ctrl Pts',(-0.00246103217853601,-0.0187700495257671,
-0.0116456393050277));
#16117=CARTESIAN_POINT('Ctrl Pts',(-0.00249858034868863,-0.018781314104265,
-0.0118199222515544));
#16118=CARTESIAN_POINT('Ctrl Pts',(-0.00251749984159334,-0.018792578682763,
-0.0119980507507866));
#16119=CARTESIAN_POINT('Ctrl Pts',(-0.002517499999999,-0.0188038432612609,
-0.0121758510436694));
#16120=CARTESIAN_POINT('Ctrl Pts',(-0.00251750042743114,-0.0188342389096755,
-0.0126556164597899));
#16121=CARTESIAN_POINT('Ctrl Pts',(-0.00237603699480804,-0.0188646345580901,
-0.0131369410996882));
#16122=CARTESIAN_POINT('Ctrl Pts',(-0.00211514174614456,-0.0188950302065047,
-0.0135411304172962));
#16123=CARTESIAN_POINT('Ctrl Pts',(-0.00201845438589362,-0.0189062947850027,
-0.0136909223294194));
#16124=CARTESIAN_POINT('Ctrl Pts',(-0.00190587290559756,-0.0189175593635007,
-0.0138302629243774));
#16125=CARTESIAN_POINT('Ctrl Pts',(-0.00178014202854226,-0.0189288239419987,
-0.0139559939012898));
#16126=CARTESIAN_POINT('Ctrl Pts',(-0.00144081382194874,-0.0189592252985253,
-0.0142953223773822));
#16127=CARTESIAN_POINT('Ctrl Pts',(-0.00100032772075606,-0.0189896266550519,
-0.0145356545566116));
#16128=CARTESIAN_POINT('Ctrl Pts',(-0.000529953127711334,-0.0190200280115784,
-0.0146369416499512));
#16129=CARTESIAN_POINT('Ctrl Pts',(-0.000355754105659654,-0.0190312868819645,
-0.0146744524187451));
#16130=CARTESIAN_POINT('Ctrl Pts',(-0.000177714129453871,-0.0190425457523505,
-0.0146933533037442));
#16131=CARTESIAN_POINT('Ctrl Pts',(2.43458683768248E-10,-0.0190538046227365,
-0.0146933532865581));
#16132=CARTESIAN_POINT('Ctrl Pts',(0.000478098543211599,-0.0190840939386791,
-0.0146933532403229));
#16133=CARTESIAN_POINT('Ctrl Pts',(0.00095788765689851,-0.0191143832546218,
-0.0145528371021288));
#16134=CARTESIAN_POINT('Ctrl Pts',(0.00136114808352063,-0.0191446725705644,
-0.0142936545389725));
#16135=CARTESIAN_POINT('Ctrl Pts',(0.00151253606525985,-0.0191560434815344,
-0.014196354822591));
#16136=CARTESIAN_POINT('Ctrl Pts',(0.00165328373806845,-0.0191674143925042,
-0.0140828523415883));
#16137=CARTESIAN_POINT('Ctrl Pts',(0.00178014237284466,-0.0191787853034742,
-0.0139559935569871));
#16138=CARTESIAN_POINT('Ctrl Pts',(0.00212440648315945,-0.0192096432466914,
-0.0136117290400828));
#16139=CARTESIAN_POINT('Ctrl Pts',(0.00236655471500398,-0.0192405011899086,
-0.0131637590122813));
#16140=CARTESIAN_POINT('Ctrl Pts',(0.00246542235843722,-0.0192713591331258,
-0.0126852635775003));
#16141=CARTESIAN_POINT('Ctrl Pts',(0.00250003230517401,-0.0192821613706837,
-0.0125177598226167));
#16142=CARTESIAN_POINT('Ctrl Pts',(0.00251750003666136,-0.0192929636082416,
-0.0123467481863637));
#16143=CARTESIAN_POINT('Ctrl Pts',(0.00251749999999994,-0.0193037658457995,
-0.0121758527464904));
#16144=CARTESIAN_POINT('',(0.00251749947628337,-0.0203037041496287,-0.012174691451596));
#16145=CARTESIAN_POINT('Ctrl Pts',(0.0025174999963034,-0.0193037743898821,
-0.0121757168592769));
#16146=CARTESIAN_POINT('Ctrl Pts',(0.00251747354082491,-0.0193346329618525,
-0.0116875324843154));
#16147=CARTESIAN_POINT('Ctrl Pts',(0.00237116161052997,-0.0193654915338229,
-0.011199374563954));
#16148=CARTESIAN_POINT('Ctrl Pts',(0.0021028851898957,-0.0193963501057933,
-0.0107917723177859));
#16149=CARTESIAN_POINT('Ctrl Pts',(0.0020089744578595,-0.0194071522145902,
-0.0106490902839838));
#16150=CARTESIAN_POINT('Ctrl Pts',(0.00190057297331317,-0.0194179543233872,
-0.0105161321686755));
#16151=CARTESIAN_POINT('Ctrl Pts',(0.00178005673749341,-0.0194287564321841,
-0.0103956273847961));
#16152=CARTESIAN_POINT('Ctrl Pts',(0.00144211995671279,-0.0194590463748431,
-0.0100577227161358));
#16153=CARTESIAN_POINT('Ctrl Pts',(0.00100359022221706,-0.0194893363175022,
-0.00981778252450338));
#16154=CARTESIAN_POINT('Ctrl Pts',(0.00053508231450667,-0.0195196262601613,
-0.00971587500073885));
#16155=CARTESIAN_POINT('Ctrl Pts',(0.000359206091161296,-0.0195309969982695,
-0.0096776192741754));
#16156=CARTESIAN_POINT('Ctrl Pts',(0.000179373751020931,-0.0195423677363778,
-0.00965834595937489));
#16157=CARTESIAN_POINT('Ctrl Pts',(-1.02807121700726E-7,-0.019553738474486,
-0.00965835328865726));
#16158=CARTESIAN_POINT('Ctrl Pts',(-0.000479969941798783,-0.0195841404588545,
-0.00965837288498654));
#16159=CARTESIAN_POINT('Ctrl Pts',(-0.000961373186645005,-0.0196145424432232,
-0.0097999142102839));
#16160=CARTESIAN_POINT('Ctrl Pts',(-0.00136559591408811,-0.0196449444275917,
-0.0100609173420373));
#16161=CARTESIAN_POINT('Ctrl Pts',(-0.00151529077974533,-0.0196562031239905,
-0.0101575740268089));
#16162=CARTESIAN_POINT('Ctrl Pts',(-0.00165454365490057,-0.0196674618203892,
-0.010270105715057));
#16163=CARTESIAN_POINT('Ctrl Pts',(-0.00178020212969005,-0.019678720516788,
-0.0103957727750511));
#16164=CARTESIAN_POINT('Ctrl Pts',(-0.00211945540596841,-0.0197091167924575,
-0.0107350492297008));
#16165=CARTESIAN_POINT('Ctrl Pts',(-0.00235975034622185,-0.0197395130681269,
-0.0111754493104245));
#16166=CARTESIAN_POINT('Ctrl Pts',(-0.00246105120592157,-0.0197699093437964,
-0.0116457276299143));
#16167=CARTESIAN_POINT('Ctrl Pts',(-0.00249859178927552,-0.0197811737488942,
-0.0118200057407289));
#16168=CARTESIAN_POINT('Ctrl Pts',(-0.00251750488525685,-0.0197924381539921,
-0.0119981284624587));
#16169=CARTESIAN_POINT('Ctrl Pts',(-0.00251749999904929,-0.01980370255909,
-0.0121759224735203));
#16170=CARTESIAN_POINT('Ctrl Pts',(-0.00251748681393115,-0.0198340988347594,
-0.0126556882246331));
#16171=CARTESIAN_POINT('Ctrl Pts',(-0.00237600953633413,-0.019864495110429,
-0.0131370091134419));
#16172=CARTESIAN_POINT('Ctrl Pts',(-0.00211510253618663,-0.0198948913860984,
-0.0135411911610115));
#16173=CARTESIAN_POINT('Ctrl Pts',(-0.00201841430455986,-0.0199061557911963,
-0.0136909749821151));
#16174=CARTESIAN_POINT('Ctrl Pts',(-0.00190583338544541,-0.0199174201962941,
-0.0138303077751249));
#16175=CARTESIAN_POINT('Ctrl Pts',(-0.00178010428520308,-0.0199286846013919,
-0.0139560316438587));
#16176=CARTESIAN_POINT('Ctrl Pts',(-0.00144076864279242,-0.0199590865857605,
-0.0142953531667276));
#16177=CARTESIAN_POINT('Ctrl Pts',(-0.00100027711999404,-0.0199894885701291,
-0.0145356760614747));
#16178=CARTESIAN_POINT('Ctrl Pts',(-0.00052990007681995,-0.0200198905544978,
-0.0146369530729516));
#16179=CARTESIAN_POINT('Ctrl Pts',(-0.000355706436766571,-0.0200311492508965,
-0.0146744587538493));
#16180=CARTESIAN_POINT('Ctrl Pts',(-0.00017767251696946,-0.0200424079472952,
-0.0146933557969358));
#16181=CARTESIAN_POINT('Ctrl Pts',(3.55668027982208E-8,-0.0200536666436939,
-0.0146933532863069));
#16182=CARTESIAN_POINT('Ctrl Pts',(0.00047813422732945,-0.0200839565863528,
-0.014693346531812));
#16183=CARTESIAN_POINT('Ctrl Pts',(0.000957921653604442,-0.0201142465290118,
-0.0145528234596369));
#16184=CARTESIAN_POINT('Ctrl Pts',(0.00136117858854318,-0.0201445364716708,
-0.014293634932548));
#16185=CARTESIAN_POINT('Ctrl Pts',(0.0015125598258468,-0.0201559072097791,
-0.0141963364696422));
#16186=CARTESIAN_POINT('Ctrl Pts',(0.00165330127616514,-0.0201672779478875,
-0.0140828365438326));
#16187=CARTESIAN_POINT('Ctrl Pts',(0.00178015458459382,-0.0201786486859959,
-0.0139559813451397));
#16188=CARTESIAN_POINT('Ctrl Pts',(0.00212441648830734,-0.0202095072579661,
-0.0136117143115169));
#16189=CARTESIAN_POINT('Ctrl Pts',(0.00236656167233786,-0.0202403658299364,
-0.0131637424207738));
#16190=CARTESIAN_POINT('Ctrl Pts',(0.00246542596178269,-0.0202712244019067,
-0.0126852461378702));
#16191=CARTESIAN_POINT('Ctrl Pts',(0.00250003361672395,-0.0202820265107037,
-0.0125177474956164));
#16192=CARTESIAN_POINT('Ctrl Pts',(0.00251750013213901,-0.0202928286195008,
-0.0123467413196633));
#16193=CARTESIAN_POINT('Ctrl Pts',(0.00251749999999925,-0.0203036307282978,
-0.0121758513399147));
#16194=CARTESIAN_POINT('',(0.00251749986350914,-0.0213038121901123,-0.01217643077317));
#16195=CARTESIAN_POINT('Ctrl Pts',(0.00251749897525818,-0.0203037743898821,
-0.0121735818169921));
#16196=CARTESIAN_POINT('Ctrl Pts',(0.00251705849677081,-0.0203346440943988,
-0.0116853938363173));
#16197=CARTESIAN_POINT('Ctrl Pts',(0.00237033046382402,-0.0203655137989155,
-0.0111973570147749));
#16198=CARTESIAN_POINT('Ctrl Pts',(0.0021017048578511,-0.0203963835034322,
-0.0107899806587582));
#16199=CARTESIAN_POINT('Ctrl Pts',(0.00200775058956061,-0.0204071804655822,
-0.0106474970436546));
#16200=CARTESIAN_POINT('Ctrl Pts',(0.00189933794761061,-0.0204179774277321,
-0.0105147334340231));
#16201=CARTESIAN_POINT('Ctrl Pts',(0.00177883905851618,-0.0204287743898821,
-0.010394410653775));
#16202=CARTESIAN_POINT('Ctrl Pts',(0.00144066537566995,-0.020459075486276,
-0.0100567312109801));
#16203=CARTESIAN_POINT('Ctrl Pts',(0.00100196371446668,-0.02048937658267,
-0.00981708960752238));
#16204=CARTESIAN_POINT('Ctrl Pts',(0.000533378912095895,-0.0205196776790639,
-0.00971550510263546));
#16205=CARTESIAN_POINT('Ctrl Pts',(0.000357618489739118,-0.0205310432493366,
-0.00967740199857939));
#16206=CARTESIAN_POINT('Ctrl Pts',(0.00017792148625705,-0.0205424088196094,
-0.00965825320302302));
#16207=CARTESIAN_POINT('Ctrl Pts',(-1.41054041913628E-6,-0.0205537743898821,
-0.00965835368171687));
#16208=CARTESIAN_POINT('Ctrl Pts',(-0.000481285466023079,-0.0205841875419004,
-0.0096586225528529));
#16209=CARTESIAN_POINT('Ctrl Pts',(-0.000962621300933848,-0.0206146006939189,
-0.00980041835081507));
#16210=CARTESIAN_POINT('Ctrl Pts',(-0.00136671151339475,-0.0206450138459373,
-0.01006163809194));
#16211=CARTESIAN_POINT('Ctrl Pts',(-0.00151623350711667,-0.0206562673605856,
-0.0101582949653016));
#16212=CARTESIAN_POINT('Ctrl Pts',(-0.00165532223979631,-0.0206675208752338,
-0.0102707953898936));
#16213=CARTESIAN_POINT('Ctrl Pts',(-0.00178083420496772,-0.0206787743898821,
-0.0103964051180471));
#16214=CARTESIAN_POINT('Ctrl Pts',(-0.00211997237410261,-0.0207091818203525,
-0.0107358074465291));
#16215=CARTESIAN_POINT('Ctrl Pts',(-0.00236011210471939,-0.0207395892508229,
-0.0111763001296675));
#16216=CARTESIAN_POINT('Ctrl Pts',(-0.0024612435032972,-0.0207699966812933,
-0.0116466211376127));
#16217=CARTESIAN_POINT('Ctrl Pts',(-0.00249869034723741,-0.0207812559174896,
-0.011820771180369));
#16218=CARTESIAN_POINT('Ctrl Pts',(-0.00251753872390049,-0.0207925151536858,
-0.0119987528246532));
#16219=CARTESIAN_POINT('Ctrl Pts',(-0.00251749994000549,-0.0208037743898821,
-0.0121764028976655));
#16220=CARTESIAN_POINT('Ctrl Pts',(-0.00251739519767926,-0.0208341818203525,
-0.0126561763164846));
#16221=CARTESIAN_POINT('Ctrl Pts',(-0.00237582175629021,-0.0208645892508229,
-0.0131374762202163));
#16222=CARTESIAN_POINT('Ctrl Pts',(-0.00211483113574972,-0.0208949966812933,
-0.0135416115072046));
#16223=CARTESIAN_POINT('Ctrl Pts',(-0.00201819176187889,-0.0209062559174896,
-0.0136912543603186));
#16224=CARTESIAN_POINT('Ctrl Pts',(-0.0019056877099657,-0.0209175151536858,
-0.0138304601068289));
#16225=CARTESIAN_POINT('Ctrl Pts',(-0.00178005707040119,-0.0209287743898821,
-0.0139560788554439));
#16226=CARTESIAN_POINT('Ctrl Pts',(-0.00144070689844957,-0.0209591875419005,
-0.0142953969078761));
#16227=CARTESIAN_POINT('Ctrl Pts',(-0.00100020153004592,-0.020989600693919,
-0.0145357093764282));
#16228=CARTESIAN_POINT('Ctrl Pts',(-0.000529814865194679,-0.0210200138459375,
-0.0146369714183467));
#16229=CARTESIAN_POINT('Ctrl Pts',(-0.000355761770664609,-0.0210312673605856,
-0.0146744405327399));
#16230=CARTESIAN_POINT('Ctrl Pts',(-0.000177875298078815,-0.0210425208752339,
-0.0146933313094496));
#16231=CARTESIAN_POINT('Ctrl Pts',(-3.11318268668838E-7,-0.0210537743898821,
-0.014693353267309));
#16232=CARTESIAN_POINT('Ctrl Pts',(0.000477795605346852,-0.021084075486276,
-0.0146934123908128));
#16233=CARTESIAN_POINT('Ctrl Pts',(0.000957608902555014,-0.02111437658267,
-0.0145529508021383));
#16234=CARTESIAN_POINT('Ctrl Pts',(0.0013609048698769,-0.0211446776790639,
-0.0142938108369224));
#16235=CARTESIAN_POINT('Ctrl Pts',(0.00151217624955624,-0.0211560432493366,
-0.0141966106086916));
#16236=CARTESIAN_POINT('Ctrl Pts',(0.00165282723223209,-0.0211674088196094,
-0.0140832338478495));
#16237=CARTESIAN_POINT('Ctrl Pts',(0.00177961672460848,-0.0211787743898821,
-0.0139565190506738));
#16238=CARTESIAN_POINT('Ctrl Pts',(0.00212398608501294,-0.0212096440943986,
-0.0136123525677949));
#16239=CARTESIAN_POINT('Ctrl Pts',(0.00236626713873879,-0.021240513798915,
-0.0131644493631118));
#16240=CARTESIAN_POINT('Ctrl Pts',(0.00246527438524578,-0.0212713835034315,
-0.0126859792077296));
#16241=CARTESIAN_POINT('Ctrl Pts',(0.00249990307735264,-0.0212821804655817,
-0.0125186298845476));
#16242=CARTESIAN_POINT('Ctrl Pts',(0.0025174202199173,-0.0212929774277319,
-0.0123477738068224));
#16243=CARTESIAN_POINT('Ctrl Pts',(0.00251749972707755,-0.0213037743898821,
-0.0121770255341664));
#16244=CARTESIAN_POINT('',(0.00251780046414957,-0.0223033403968196,-0.0121761624005998));
#16245=CARTESIAN_POINT('Ctrl Pts',(0.00251749999994073,-0.0213038499903425,
-0.0121758360121736));
#16246=CARTESIAN_POINT('Ctrl Pts',(0.00251749665014283,-0.0213347138852245,
-0.0116876498063799));
#16247=CARTESIAN_POINT('Ctrl Pts',(0.00237120678745751,-0.0213655777801066,
-0.0111994834398425));
#16248=CARTESIAN_POINT('Ctrl Pts',(0.00210294792643045,-0.0213964416749887,
-0.010791867640418));
#16249=CARTESIAN_POINT('Ctrl Pts',(0.00200908115279786,-0.0214072412967541,
-0.010649238316536));
#16250=CARTESIAN_POINT('Ctrl Pts',(0.0019007347840987,-0.0214180409185194,
-0.0105163244402839));
#16251=CARTESIAN_POINT('Ctrl Pts',(0.00178028171630679,-0.0214288405402849,
-0.010395852370664));
#16252=CARTESIAN_POINT('Ctrl Pts',(0.00144238479207546,-0.0214591358166468,
-0.0100579021421928));
#16253=CARTESIAN_POINT('Ctrl Pts',(0.00100388155370561,-0.0214894310930088,
-0.00981790589049112));
#16254=CARTESIAN_POINT('Ctrl Pts',(0.000535383004862202,-0.0215197263693707,
-0.00971594042466548));
#16255=CARTESIAN_POINT('Ctrl Pts',(0.000359579885819401,-0.0215310946096563,
-0.00967767809285879));
#16256=CARTESIAN_POINT('Ctrl Pts',(0.000179821417535125,-0.0215424628499418,
-0.00965838285146188));
#16257=CARTESIAN_POINT('Ctrl Pts',(4.14386135004118E-7,-0.0215538310902274,
-0.00965835332066254));
#16258=CARTESIAN_POINT('Ctrl Pts',(-0.000479456527140519,-0.0215842384148768,
-0.00965827433283503));
#16259=CARTESIAN_POINT('Ctrl Pts',(-0.000960891814846311,-0.0216146457395262,
-0.00979971888222035));
#16260=CARTESIAN_POINT('Ctrl Pts',(-0.00136516965727927,-0.0216450530641756,
-0.0100606421725451));
#16261=CARTESIAN_POINT('Ctrl Pts',(-0.00151482534279141,-0.0216563092561736,
-0.0101572308296049));
#16262=CARTESIAN_POINT('Ctrl Pts',(-0.00165405045888319,-0.0216675654481718,
-0.0102696841045556));
#16263=CARTESIAN_POINT('Ctrl Pts',(-0.00177969563557523,-0.0216788216401698,
-0.0103952663904156));
#16264=CARTESIAN_POINT('Ctrl Pts',(-0.00211904802334732,-0.0217092232499438,
-0.0107344489176758));
#16265=CARTESIAN_POINT('Ctrl Pts',(-0.00235946883020976,-0.0217396248597177,
-0.0111747841255715));
#16266=CARTESIAN_POINT('Ctrl Pts',(-0.00246090230640666,-0.0217700264694917,
-0.0116450368509399));
#16267=CARTESIAN_POINT('Ctrl Pts',(-0.00249847710495456,-0.0217812883763652,
-0.011819236258126));
#16268=CARTESIAN_POINT('Ctrl Pts',(-0.00251744013055233,-0.0217925502832388,
-0.0119972824892468));
#16269=CARTESIAN_POINT('Ctrl Pts',(-0.00251749985783616,-0.0218038121901123,
-0.0121750072399159));
#16270=CARTESIAN_POINT('Ctrl Pts',(-0.00251766109212767,-0.0218342137998863,
-0.0126547766588689));
#16271=CARTESIAN_POINT('Ctrl Pts',(-0.00237635673330881,-0.0218646154096603,
-0.0131361518485057));
#16272=CARTESIAN_POINT('Ctrl Pts',(-0.00211559356671986,-0.0218950170194343,
-0.0135404301845208));
#16273=CARTESIAN_POINT('Ctrl Pts',(-0.00201899702068176,-0.0219062789263078,
-0.0136901901809495));
#16274=CARTESIAN_POINT('Ctrl Pts',(-0.00190651651240216,-0.0219175408331812,
-0.0138295130796314));
#16275=CARTESIAN_POINT('Ctrl Pts',(-0.00178089202362918,-0.0219288027400547,
-0.0139552435894917));
#16276=CARTESIAN_POINT('Ctrl Pts',(-0.0014417039396801,-0.0219592100647042,
-0.0142947179320342));
#16277=CARTESIAN_POINT('Ctrl Pts',(-0.00100131523292127,-0.0219896173893536,
-0.0145352363725553));
#16278=CARTESIAN_POINT('Ctrl Pts',(-0.000530979723704272,-0.022020024714003,
-0.0146367203660679));
#16279=CARTESIAN_POINT('Ctrl Pts',(-0.000356870792507748,-0.0220312809060011,
-0.0146742877393531));
#16280=CARTESIAN_POINT('Ctrl Pts',(-0.000178916436407483,-0.0220425370979991,
-0.0146932628053001));
#16281=CARTESIAN_POINT('Ctrl Pts',(-1.27770712460287E-6,-0.0220537932899972,
-0.0146933529623206));
#16282=CARTESIAN_POINT('Ctrl Pts',(0.000476824869407315,-0.0220840885663592,
-0.014693595613819));
#16283=CARTESIAN_POINT('Ctrl Pts',(0.000956688669868174,-0.0221143838427211,
-0.0145533206203796));
#16284=CARTESIAN_POINT('Ctrl Pts',(0.00136008235768505,-0.0221446791190831,
-0.0142943391209015));
#16285=CARTESIAN_POINT('Ctrl Pts',(0.00151145501122909,-0.0221560473593686,
-0.0141971568446816));
#16286=CARTESIAN_POINT('Ctrl Pts',(0.00165220458265205,-0.0221674155996541,
-0.0140837802632861));
#16287=CARTESIAN_POINT('Ctrl Pts',(0.00177908491797799,-0.0221787838399396,
-0.0139570503853159));
#16288=CARTESIAN_POINT('Ctrl Pts',(0.00212355523473457,-0.0222096477348218,
-0.0136129885486668));
#16289=CARTESIAN_POINT('Ctrl Pts',(0.00236596974171468,-0.022240511629704,
-0.0131651600397046));
#16290=CARTESIAN_POINT('Ctrl Pts',(0.00246512068629229,-0.0222713755245862,
-0.0126867214221996));
#16291=CARTESIAN_POINT('Ctrl Pts',(0.00249981470994674,-0.0222821751463515,
-0.0125193104027319));
#16292=CARTESIAN_POINT('Ctrl Pts',(0.00251738343267912,-0.0222929747681168,
-0.0123483844243074));
#16293=CARTESIAN_POINT('Ctrl Pts',(0.00251749941967471,-0.0223037743898821,
-0.0121775626541275));
#16294=CARTESIAN_POINT('',(0.00251749967473612,-0.0233037176099892,-0.0121749448086545));
#16295=CARTESIAN_POINT('Ctrl Pts',(0.00251749999999092,-0.0223038816194607,
-0.0121758600475192));
#16296=CARTESIAN_POINT('Ctrl Pts',(0.0025175013076005,-0.0223345812349272,
-0.0116889607629736));
#16297=CARTESIAN_POINT('Ctrl Pts',(0.0023719606845788,-0.0223652878514534,
-0.0112019687080946));
#16298=CARTESIAN_POINT('Ctrl Pts',(0.0021050319083829,-0.0223960166366596,
-0.010795039427021));
#16299=CARTESIAN_POINT('Ctrl Pts',(0.00201064111538942,-0.0224068828851198,
-0.0106511419496481));
#16300=CARTESIAN_POINT('Ctrl Pts',(0.00190153428401059,-0.0224177519056763,
-0.0105171068557753));
#16301=CARTESIAN_POINT('Ctrl Pts',(0.0017801554621912,-0.0224286243690166,
-0.0103957261055874));
#16302=CARTESIAN_POINT('Ctrl Pts',(0.00144142058921467,-0.0224589664207296,
-0.0100569858510652));
#16303=CARTESIAN_POINT('Ctrl Pts',(0.00100161012373136,-0.0224893352853389,
-0.00981665712105438));
#16304=CARTESIAN_POINT('Ctrl Pts',(0.000531596077416871,-0.022519687231543,
-0.00971511927808115));
#16305=CARTESIAN_POINT('Ctrl Pts',(0.000356906568067011,-0.0225309680999166,
-0.00967738084003122));
#16306=CARTESIAN_POINT('Ctrl Pts',(0.00017830964556315,-0.0225422466312219,
-0.00965835423079078));
#16307=CARTESIAN_POINT('Ctrl Pts',(1.33318343165638E-8,-0.0225535205802314,
-0.0096583532865934));
#16308=CARTESIAN_POINT('Ctrl Pts',(-0.000487515190307265,-0.022584347755423,
-0.00965835070480611));
#16309=CARTESIAN_POINT('Ctrl Pts',(-0.00097570005348263,-0.0226151406697395,
-0.0098042645785878));
#16310=CARTESIAN_POINT('Ctrl Pts',(-0.00138377394701436,-0.022646067631192,
-0.0100727660526174));
#16311=CARTESIAN_POINT('Ctrl Pts',(-0.00152647526742239,-0.0226568826289301,
-0.0101666596230782));
#16312=CARTESIAN_POINT('Ctrl Pts',(-0.00165951649133449,-0.0226677140188173,
-0.0102750877733898));
#16313=CARTESIAN_POINT('Ctrl Pts',(-0.0017801366081372,-0.0226785689981989,
-0.0103957072514335));
#16314=CARTESIAN_POINT('Ctrl Pts',(-0.00208925477812789,-0.0227063875035252,
-0.01070482378445));
#16315=CARTESIAN_POINT('Ctrl Pts',(-0.0023182875516416,-0.0227343609362434,
-0.0111011289644275));
#16316=CARTESIAN_POINT('Ctrl Pts',(-0.00243164824112718,-0.0227620377754448,
-0.0115240150540011));
#16317=CARTESIAN_POINT('Ctrl Pts',(-0.00248901528948984,-0.0227760438526854,
-0.0117380198105225));
#16318=CARTESIAN_POINT('Ctrl Pts',(-0.00251749999999999,-0.0227899739739923,
-0.0119583162425569));
#16319=CARTESIAN_POINT('Ctrl Pts',(-0.0025175,-0.022803769622919,-0.012175853286558));
#16320=CARTESIAN_POINT('Ctrl Pts',(-0.00251750000000002,-0.02284482629222,
-0.0128232564296606));
#16321=CARTESIAN_POINT('Ctrl Pts',(-0.00226454183273898,-0.0228846919492015,
-0.0134500557724457));
#16322=CARTESIAN_POINT('Ctrl Pts',(-0.00182003347813458,-0.0229253542607035,
-0.0139151877536659));
#16323=CARTESIAN_POINT('Ctrl Pts',(-0.00150076880653732,-0.0229545596499691,
-0.014249265184822));
#16324=CARTESIAN_POINT('Ctrl Pts',(-0.00108140438732256,-0.022984176010916,
-0.0144976113812731));
#16325=CARTESIAN_POINT('Ctrl Pts',(-0.000624780936849887,-0.0230140057534222,
-0.0146145937464982));
#16326=CARTESIAN_POINT('Ctrl Pts',(-0.000445653060287442,-0.0230257076019102,
-0.0146604845185476));
#16327=CARTESIAN_POINT('Ctrl Pts',(-0.000261162728481951,-0.0230374422876512,
-0.0146866080241517));
#16328=CARTESIAN_POINT('Ctrl Pts',(-7.60742024150088E-5,-0.0230491978823017,
-0.0146922036130681));
#16329=CARTESIAN_POINT('Ctrl Pts',(0.000394806181150458,-0.0230791050787968,
-0.0147064392499884));
#16330=CARTESIAN_POINT('Ctrl Pts',(0.000875641029012556,-0.0231091476051378,
-0.0145843270790017));
#16331=CARTESIAN_POINT('Ctrl Pts',(0.00128748301215453,-0.0231393790289019,
-0.0143392288303353));
#16332=CARTESIAN_POINT('Ctrl Pts',(0.00145018545103835,-0.0231513222658196,
-0.0142424002299097));
#16333=CARTESIAN_POINT('Ctrl Pts',(0.00160218063497924,-0.0231632949844648,
-0.0141269606956049));
#16334=CARTESIAN_POINT('Ctrl Pts',(0.00173934420262757,-0.0231753004877138,
-0.0139958774607893));
#16335=CARTESIAN_POINT('Ctrl Pts',(0.00208806524676423,-0.02320582296318,
-0.0136626148948074));
#16336=CARTESIAN_POINT('Ctrl Pts',(0.00234152922365597,-0.023236557347308,
-0.0132226449996777));
#16337=CARTESIAN_POINT('Ctrl Pts',(0.00245239154138134,-0.023267485547987,
-0.0127446959517664));
#16338=CARTESIAN_POINT('Ctrl Pts',(0.00249551121723139,-0.0232795150095323,
-0.0125587986293792));
#16339=CARTESIAN_POINT('Ctrl Pts',(0.00251750054521379,-0.0232915737917502,
-0.0123675108385863));
#16340=CARTESIAN_POINT('Ctrl Pts',(0.00251749999998981,-0.0233036608300962,
-0.0121758461250867));
#16341=CARTESIAN_POINT('',(0.00251749989572715,-0.0243037413029277,-0.012175349188554));
#16342=CARTESIAN_POINT('Ctrl Pts',(0.00251749934948243,-0.0233037743898821,
-0.0121740434922223));
#16343=CARTESIAN_POINT('Ctrl Pts',(0.00251714839939817,-0.0233346387771943,
-0.0116858572981548));
#16344=CARTESIAN_POINT('Ctrl Pts',(0.00237051092282184,-0.0233655031645063,
-0.0111977951221388));
#16345=CARTESIAN_POINT('Ctrl Pts',(0.00210196178929609,-0.0233963675518184,
-0.0107903703792874));
#16346=CARTESIAN_POINT('Ctrl Pts',(0.00200799581241252,-0.0234071670739267,
-0.0106478114982889));
#16347=CARTESIAN_POINT('Ctrl Pts',(0.00189955788753691,-0.0234179665960352,
-0.0105149778851826));
#16348=CARTESIAN_POINT('Ctrl Pts',(0.0017790226651697,-0.0234287661181435,
-0.0103945940109858));
#16349=CARTESIAN_POINT('Ctrl Pts',(0.00144088668856546,-0.0234590618846693,
-0.010056882609542));
#16350=CARTESIAN_POINT('Ctrl Pts',(0.00100221362327,-0.0234893576511951,
-0.00981719643570375));
#16351=CARTESIAN_POINT('Ctrl Pts',(0.000533642873359993,-0.0235196534177209,
-0.00971556234162657));
#16352=CARTESIAN_POINT('Ctrl Pts',(0.00035781701212283,-0.0235310215606156,
-0.00967742530015393));
#16353=CARTESIAN_POINT('Ctrl Pts',(0.000178049411175644,-0.0235423897035102,
-0.00965825721461444));
#16354=CARTESIAN_POINT('Ctrl Pts',(-1.35325041630699E-6,-0.0235537578464049,
-0.00965835365026948));
#16355=CARTESIAN_POINT('Ctrl Pts',(-0.000481224337450019,-0.0235841656622088,
-0.00965861159896546));
#16356=CARTESIAN_POINT('Ctrl Pts',(-0.00096256037853341,-0.0236145734780127,
-0.00980039428131228));
#16357=CARTESIAN_POINT('Ctrl Pts',(-0.00136665501056534,-0.0236449812938166,
-0.0100616015673684));
#16358=CARTESIAN_POINT('Ctrl Pts',(-0.00151623915161095,-0.0236562373874332,
-0.0101582929471155));
#16359=CARTESIAN_POINT('Ctrl Pts',(-0.00165538209716498,-0.0236674934810497,
-0.0102708408343145));
#16360=CARTESIAN_POINT('Ctrl Pts',(-0.0017809366237846,-0.0236787495746663,
-0.0103965076225392));
#16361=CARTESIAN_POINT('Ctrl Pts',(-0.00212005261448095,-0.0237091516751793,
-0.0107359268257637));
#16362=CARTESIAN_POINT('Ctrl Pts',(-0.002360166398731,-0.0237395537756923,
-0.0111764297667141));
#16363=CARTESIAN_POINT('Ctrl Pts',(-0.00246127191791879,-0.0237699558762053,
-0.0116467532997273));
#16364=CARTESIAN_POINT('Ctrl Pts',(-0.00249872429842445,-0.0237812176851127,
-0.0118209746089168));
#16365=CARTESIAN_POINT('Ctrl Pts',(-0.00251756314240969,-0.0237924794940202,
-0.0119990295727695));
#16366=CARTESIAN_POINT('Ctrl Pts',(-0.00251749984030139,-0.0238037413029277,
-0.0121767499930103));
#16367=CARTESIAN_POINT('Ctrl Pts',(-0.00251732895149704,-0.0238341434034407,
-0.0126565196395877));
#16368=CARTESIAN_POINT('Ctrl Pts',(-0.00237569126217508,-0.0238645455039536,
-0.013137797076297));
#16369=CARTESIAN_POINT('Ctrl Pts',(-0.00211464809887879,-0.0238949476044665,
-0.0135418948920403));
#16370=CARTESIAN_POINT('Ctrl Pts',(-0.00201795023353186,-0.023906209413374,
-0.0136915842984982));
#16371=CARTESIAN_POINT('Ctrl Pts',(-0.00190537641728073,-0.0239174712222816,
-0.0138308261240018));
#16372=CARTESIAN_POINT('Ctrl Pts',(-0.00177966860435043,-0.0239287330311891,
-0.013956467199985));
#16373=CARTESIAN_POINT('Ctrl Pts',(-0.0014402471089149,-0.0239591408469931,
-0.0142957085001418));
#16374=CARTESIAN_POINT('Ctrl Pts',(-0.000999692969905732,-0.023989548662797,
-0.0145359242365833));
#16375=CARTESIAN_POINT('Ctrl Pts',(-0.000529287611887201,-0.0240199564786011,
-0.0146370848632089));
#16376=CARTESIAN_POINT('Ctrl Pts',(-0.000355157158661542,-0.0240312125722175,
-0.0146745316002892));
#16377=CARTESIAN_POINT('Ctrl Pts',(-0.000177194252723598,-0.024042468665834,
-0.0146933843058751));
#16378=CARTESIAN_POINT('Ctrl Pts',(4.40162458844756E-7,-0.0240537247594505,
-0.0146933532480789));
#16379=CARTESIAN_POINT('Ctrl Pts',(0.000478543041901331,-0.0240840205259763,
-0.0146932696560462));
#16380=CARTESIAN_POINT('Ctrl Pts',(0.000958311206875898,-0.0241143162925021,
-0.0145526671107832));
#16381=CARTESIAN_POINT('Ctrl Pts',(0.00136152817913595,-0.0241446120590279,
-0.014293410196636));
#16382=CARTESIAN_POINT('Ctrl Pts',(0.00151283077629276,-0.0241559802019226,
-0.0141961269790634));
#16383=CARTESIAN_POINT('Ctrl Pts',(0.00165349975956908,-0.0241673483448172,
-0.0140826575027536));
#16384=CARTESIAN_POINT('Ctrl Pts',(0.00178029114450994,-0.0241787164877119,
-0.0139558447727118));
#16385=CARTESIAN_POINT('Ctrl Pts',(0.0021245284090231,-0.024209580875024,
-0.013611549556476));
#16386=CARTESIAN_POINT('Ctrl Pts',(0.00236663950474416,-0.0242404452623361,
-0.0131635567966713));
#16387=CARTESIAN_POINT('Ctrl Pts',(0.00246546627037973,-0.0242713096496483,
-0.0126850510080965));
#16388=CARTESIAN_POINT('Ctrl Pts',(0.00250004598938024,-0.0242821091717566,
-0.0125176207011081));
#16389=CARTESIAN_POINT('Ctrl Pts',(0.00251749888842494,-0.0242929086938649,
-0.0123466872160051));
#16390=CARTESIAN_POINT('Ctrl Pts',(0.0025174999999467,-0.0243037082159733,
-0.0121758696681072));
#16391=CARTESIAN_POINT('',(0.00251749947769908,-0.0253038475563787,-0.0121769984087159));
#16392=CARTESIAN_POINT('Ctrl Pts',(0.0025174997915076,-0.0243037743898821,
-0.0121748287090009));
#16393=CARTESIAN_POINT('Ctrl Pts',(0.00251730110768886,-0.0243346438561,
-0.0116866407053165));
#16394=CARTESIAN_POINT('Ctrl Pts',(0.00237081488912746,-0.0243655133223179,
-0.0111985313831862));
#16395=CARTESIAN_POINT('Ctrl Pts',(0.00210239121357112,-0.0243963827885358,
-0.0107910220928385));
#16396=CARTESIAN_POINT('Ctrl Pts',(0.00200850477544109,-0.0244071799889846,
-0.0106484877366705));
#16397=CARTESIAN_POINT('Ctrl Pts',(0.00190015429315438,-0.0244179771894333,
-0.0105156667991757));
#16398=CARTESIAN_POINT('Ctrl Pts',(0.00177971076513969,-0.0244287743898821,
-0.0103952815125355));
#16399=CARTESIAN_POINT('Ctrl Pts',(0.00144170260947175,-0.0244590752443175,
-0.0100574368032553));
#16400=CARTESIAN_POINT('Ctrl Pts',(0.0010031185756684,-0.0244893760987529,
-0.00981758055491305));
#16401=CARTESIAN_POINT('Ctrl Pts',(0.000534583810026133,-0.0245196769531884,
-0.00971576662140625));
#16402=CARTESIAN_POINT('Ctrl Pts',(0.000358837011154647,-0.0245310427654196,
-0.00967757634353048));
#16403=CARTESIAN_POINT('Ctrl Pts',(0.000179144120941101,-0.0245424085776508,
-0.00965833954017976));
#16404=CARTESIAN_POINT('Ctrl Pts',(-1.9307286565947E-7,-0.0245537743898821,
-0.0096583532939617));
#16405=CARTESIAN_POINT('Ctrl Pts',(-0.000480067792651366,-0.0245841873000199,
-0.00965839009665786));
#16406=CARTESIAN_POINT('Ctrl Pts',(-0.000961471924135367,-0.0246146002101576,
-0.00979995294595022));
#16407=CARTESIAN_POINT('Ctrl Pts',(-0.00136568830462723,-0.0246450131202954,
-0.0100609770006718));
#16408=CARTESIAN_POINT('Ctrl Pts',(-0.001515261387586,-0.0246562668768243,
-0.0101575643100321));
#16409=CARTESIAN_POINT('Ctrl Pts',(-0.00165440826965524,-0.0246675206333532,
-0.0102700011398836));
#16410=CARTESIAN_POINT('Ctrl Pts',(-0.00177998385649334,-0.0246787743898821,
-0.0103955545137048));
#16411=CARTESIAN_POINT('Ctrl Pts',(-0.00211928394665964,-0.0247091815788996,
-0.0107347945852096));
#16412=CARTESIAN_POINT('Ctrl Pts',(-0.0023596340554676,-0.024739588767917,
-0.0111751722301901));
#16413=CARTESIAN_POINT('Ctrl Pts',(-0.00246099022860495,-0.0247699959569346,
-0.0116454446283417));
#16414=CARTESIAN_POINT('Ctrl Pts',(-0.00249852140471561,-0.0247812554345837,
-0.0118195817888982));
#16415=CARTESIAN_POINT('Ctrl Pts',(-0.002517454866124,-0.024792514912233,
-0.0119975596639281));
#16416=CARTESIAN_POINT('Ctrl Pts',(-0.00251749991904762,-0.0248037743898821,
-0.0121752148547111));
#16417=CARTESIAN_POINT('Ctrl Pts',(-0.00251762158834767,-0.0248341815788995,
-0.0126549879964489));
#16418=CARTESIAN_POINT('Ctrl Pts',(-0.00237627544809769,-0.024864588767917,
-0.0131363544427929));
#16419=CARTESIAN_POINT('Ctrl Pts',(-0.00211547580451566,-0.0248949959569345,
-0.0135406127417401));
#16420=CARTESIAN_POINT('Ctrl Pts',(-0.00201890430768491,-0.0249062554345837,
-0.0136903055423107));
#16421=CARTESIAN_POINT('Ctrl Pts',(-0.00190646228399861,-0.0249175149122329,
-0.0138295681218715));
#16422=CARTESIAN_POINT('Ctrl Pts',(-0.00178088658635174,-0.0249287743898821,
-0.0139552490313413));
#16423=CARTESIAN_POINT('Ctrl Pts',(-0.00144169479371151,-0.0249591873000199,
-0.0142947250110296));
#16424=CARTESIAN_POINT('Ctrl Pts',(-0.00100130174122861,-0.0249896002101577,
-0.0145352427148896));
#16425=CARTESIAN_POINT('Ctrl Pts',(-0.000530962569348486,-0.0250200131202955,
-0.0146367240673897));
#16426=CARTESIAN_POINT('Ctrl Pts',(-0.000356921923374615,-0.0250312668768244,
-0.0146742754371232));
#16427=CARTESIAN_POINT('Ctrl Pts',(-0.000179039012638287,-0.0250425206333532,
-0.0146932491770583));
#16428=CARTESIAN_POINT('Ctrl Pts',(-1.46993648989972E-6,-0.0250537743898821,
-0.0146933528574194));
#16429=CARTESIAN_POINT('Ctrl Pts',(0.000476636615291263,-0.0250840752443175,
-0.0146936320178509));
#16430=CARTESIAN_POINT('Ctrl Pts',(0.000956514274019615,-0.0251143760987529,
-0.0145533914309386));
#16431=CARTESIAN_POINT('Ctrl Pts',(0.00135992934321918,-0.0251446769531883,
-0.0142944373494292));
#16432=CARTESIAN_POINT('Ctrl Pts',(0.00151124982619627,-0.0251560427654196,
-0.0141973040004925));
#16433=CARTESIAN_POINT('Ctrl Pts',(0.001651956748588,-0.0251674085776508,
-0.0140839882941535));
#16434=CARTESIAN_POINT('Ctrl Pts',(0.00177880743895631,-0.0251787743898821,
-0.0139573274921288));
#16435=CARTESIAN_POINT('Ctrl Pts',(0.0021233330233452,-0.0252096438560999,
-0.0136133176431479));
#16436=CARTESIAN_POINT('Ctrl Pts',(0.00236581755152097,-0.0252405133223177,
-0.01316552473233));
#16437=CARTESIAN_POINT('Ctrl Pts',(0.00246504225247071,-0.0252713827885355,
-0.0126870997472149));
#16438=CARTESIAN_POINT('Ctrl Pts',(0.0024997480351387,-0.0252821799889844,
-0.0125197612377771));
#16439=CARTESIAN_POINT('Ctrl Pts',(0.00251734284924451,-0.0252929771894332,
-0.0123489079867308));
#16440=CARTESIAN_POINT('Ctrl Pts',(0.00251749894803741,-0.0253037743898821,
-0.0121781547275306));
#16441=CARTESIAN_POINT('',(0.00251749999991786,-0.0263037743898821,-0.0121758329495021));
#16442=CARTESIAN_POINT('Ctrl Pts',(0.00251749999999526,-0.0253039197054202,
-0.0121758581696978));
#16443=CARTESIAN_POINT('Ctrl Pts',(0.00251750094691551,-0.0253347779048283,
-0.011687673954906));
#16444=CARTESIAN_POINT('Ctrl Pts',(0.00237121650892537,-0.0253656361042366,
-0.0111995079564218));
#16445=CARTESIAN_POINT('Ctrl Pts',(0.00210296312023231,-0.0253964943036448,
-0.0107918907274754));
#16446=CARTESIAN_POINT('Ctrl Pts',(0.00200905712677098,-0.0254072966643753,
-0.010649198398321));
#16447=CARTESIAN_POINT('Ctrl Pts',(0.00190065881351593,-0.0254180990251058,
-0.0105162298587498));
#16448=CARTESIAN_POINT('Ctrl Pts',(0.00178014429023032,-0.0254289013858364,
-0.0103957149335191));
#16449=CARTESIAN_POINT('Ctrl Pts',(0.00144222437939734,-0.0254591909532291,
-0.0100577938956416));
#16450=CARTESIAN_POINT('Ctrl Pts',(0.00100370678302795,-0.0254894805206217,
-0.00981783219268631));
#16451=CARTESIAN_POINT('Ctrl Pts',(0.00053520419770457,-0.0255197700880144,
-0.0097159015153318));
#16452=CARTESIAN_POINT('Ctrl Pts',(0.000359323854807006,-0.0255311410807605,
-0.00967763576601365));
#16453=CARTESIAN_POINT('Ctrl Pts',(0.00017948618320112,-0.0255425120735066,
-0.00965835353703899));
#16454=CARTESIAN_POINT('Ctrl Pts',(3.51331674627921E-9,-0.0255538830662527,
-0.00965835328656055));
#16455=CARTESIAN_POINT('Ctrl Pts',(-0.000479863289043699,-0.0255842846751225,
-0.00965835261687869));
#16456=CARTESIAN_POINT('Ctrl Pts',(-0.000961272249621784,-0.0256146862839923,
-0.00979987342420779));
#16457=CARTESIAN_POINT('Ctrl Pts',(-0.0013655058674309,-0.0256450878928621,
-0.0100608592024028));
#16458=CARTESIAN_POINT('Ctrl Pts',(-0.0015152100039348,-0.025656346844131,
-0.0101575128423852));
#16459=CARTESIAN_POINT('Ctrl Pts',(-0.00165447210278662,-0.0256676057954,
-0.010270043028446));
#16460=CARTESIAN_POINT('Ctrl Pts',(-0.00178013932165148,-0.0256788647466689,
-0.0103957099649376));
#16461=CARTESIAN_POINT('Ctrl Pts',(-0.00211940433969015,-0.0257092606473649,
-0.0107349742206502));
#16462=CARTESIAN_POINT('Ctrl Pts',(-0.00235971476715102,-0.0257396565480609,
-0.0111753655143751));
#16463=CARTESIAN_POINT('Ctrl Pts',(-0.00246103232269861,-0.0257700524487569,
-0.0116456399741708));
#16464=CARTESIAN_POINT('Ctrl Pts',(-0.00249858040427162,-0.0257813171081996,
-0.0118199227397062));
#16465=CARTESIAN_POINT('Ctrl Pts',(-0.00251749984861343,-0.0257925817676425,
-0.0119980510444317));
#16466=CARTESIAN_POINT('Ctrl Pts',(-0.00251749999999909,-0.0258038464270852,
-0.0121758511430643));
#16467=CARTESIAN_POINT('Ctrl Pts',(-0.00251750040848933,-0.0258342423277812,
-0.0126556165695495));
#16468=CARTESIAN_POINT('Ctrl Pts',(-0.00237603695104173,-0.0258646382284771,
-0.0131369412119922));
#16469=CARTESIAN_POINT('Ctrl Pts',(-0.00211514167765687,-0.0258950341291731,
-0.0135411305234001));
#16470=CARTESIAN_POINT('Ctrl Pts',(-0.00201845441596638,-0.0259062987886159,
-0.013690922266338));
#16471=CARTESIAN_POINT('Ctrl Pts',(-0.00190587306977369,-0.0259175634480587,
-0.013830262714367));
#16472=CARTESIAN_POINT('Ctrl Pts',(-0.00178014235301023,-0.0259288281075014,
-0.0139559935768215));
#16473=CARTESIAN_POINT('Ctrl Pts',(-0.00144081420080273,-0.0259592297163713,
-0.0142953221222273));
#16474=CARTESIAN_POINT('Ctrl Pts',(-0.00100032813333106,-0.025989631325241,
-0.0145356543834411));
#16475=CARTESIAN_POINT('Ctrl Pts',(-0.000529953549387098,-0.0260200329341109,
-0.0146369415591505));
#16476=CARTESIAN_POINT('Ctrl Pts',(-0.000355754725191628,-0.0260312918853798,
-0.0146744523165701));
#16477=CARTESIAN_POINT('Ctrl Pts',(-0.0001777149521045,-0.0260425508366488,
-0.0146933532319434));
#16478=CARTESIAN_POINT('Ctrl Pts',(-7.73670714469243E-10,-0.0260538097879177,
-0.014693353286558));
#16479=CARTESIAN_POINT('Ctrl Pts',(0.0004780975372398,-0.0260840993553103,
-0.0146933534334858));
#16480=CARTESIAN_POINT('Ctrl Pts',(0.00095788671648783,-0.026114388922703,
-0.0145528374828911));
#16481=CARTESIAN_POINT('Ctrl Pts',(0.00136114725230904,-0.0261446784900957,
-0.0142936550732066));
#16482=CARTESIAN_POINT('Ctrl Pts',(0.00151253510701687,-0.0261560494828417,
-0.0141963555224329));
#16483=CARTESIAN_POINT('Ctrl Pts',(0.00165328268251051,-0.0261674204755878,
-0.0140828532383766));
#16484=CARTESIAN_POINT('Ctrl Pts',(0.0017801412588749,-0.0261787914683339,
-0.0139559946709575));
#16485=CARTESIAN_POINT('Ctrl Pts',(0.00212440559213063,-0.026209649667664,
-0.0136117303619771));
#16486=CARTESIAN_POINT('Ctrl Pts',(0.00236655410612732,-0.0262405078669941,
-0.0131637604750869));
#16487=CARTESIAN_POINT('Ctrl Pts',(0.0024654220453634,-0.0262713660663242,
-0.0126852650926994));
#16488=CARTESIAN_POINT('Ctrl Pts',(0.00250003216847695,-0.0262821684162683,
-0.0125177610036929));
#16489=CARTESIAN_POINT('Ctrl Pts',(0.00251750000546539,-0.0262929707662124,
-0.0123467490079382));
#16490=CARTESIAN_POINT('Ctrl Pts',(0.0025175,-0.0263037731161565,-0.0121758532060463));
#16491=CARTESIAN_POINT('',(0.00178014132163718,-0.0271787743898721,-0.0139559946081952));
#16492=CARTESIAN_POINT('Ctrl Pts',(0.00251749999991786,-0.0263037743898821,
-0.0121758329495021));
#16493=CARTESIAN_POINT('Ctrl Pts',(0.00251749603863613,-0.0263347748696889,
-0.0116854705911618));
#16494=CARTESIAN_POINT('Ctrl Pts',(0.00236996703968252,-0.0263657753494956,
-0.011195464878576));
#16495=CARTESIAN_POINT('Ctrl Pts',(0.00209960641145874,-0.0263967758293024,
-0.0107868035513213));
#16496=CARTESIAN_POINT('Ctrl Pts',(0.00205200751242907,-0.0264022336828289,
-0.0107148558369625));
#16497=CARTESIAN_POINT('Ctrl Pts',(0.00200072463137587,-0.0264076915363556,
-0.010645383814245));
#16498=CARTESIAN_POINT('Ctrl Pts',(0.00194604252731177,-0.0264131493898821,
-0.0105787544380537));
#16499=CARTESIAN_POINT('Ctrl Pts',(0.00163987935158639,-0.026443707719649,
-0.0102056989062584));
#16500=CARTESIAN_POINT('Ctrl Pts',(0.00122255791486552,-0.0264742660494157,
-0.00992269456928358));
#16501=CARTESIAN_POINT('Ctrl Pts',(0.000761937724844168,-0.0265048243791826,
-0.00977642478096363));
#16502=CARTESIAN_POINT('Ctrl Pts',(0.000673004174330689,-0.0265107243827491,
-0.00974818396154244));
#16503=CARTESIAN_POINT('Ctrl Pts',(0.000582539135272105,-0.0265166243863156,
-0.00972490620853916));
#16504=CARTESIAN_POINT('Ctrl Pts',(0.0004911249259527,-0.0265225243898821,
-0.00970672336751618));
#16505=CARTESIAN_POINT('Ctrl Pts',(1.61855418273218E-5,-0.0265531776557264,
-0.00961225504162464));
#16506=CARTESIAN_POINT('Ctrl Pts',(-0.000487496367874373,-0.0265838309215706,
-0.00965888445140582));
#16507=CARTESIAN_POINT('Ctrl Pts',(-0.000937385750862611,-0.0266144841874148,
-0.00983937854796585));
#16508=CARTESIAN_POINT('Ctrl Pts',(-0.00102258509778175,-0.0266202892549039,
-0.00987356023735698));
#16509=CARTESIAN_POINT('Ctrl Pts',(-0.00110587625694516,-0.026626094322393,
-0.00991239272061271));
#16510=CARTESIAN_POINT('Ctrl Pts',(-0.00118675249474565,-0.0266318993898821,
-0.00995562249535306));
#16511=CARTESIAN_POINT('Ctrl Pts',(-0.00161367118635103,-0.0266625424054887,
-0.0101838180614731));
#16512=CARTESIAN_POINT('Ctrl Pts',(-0.00197335343554593,-0.0266931854210953,
-0.0105392410064605));
#16513=CARTESIAN_POINT('Ctrl Pts',(-0.00220661996526684,-0.0267238284367018,
-0.0109639809422554));
#16514=CARTESIAN_POINT('Ctrl Pts',(-0.00225088842117747,-0.0267296437544286,
-0.0110445865102454));
#16515=CARTESIAN_POINT('Ctrl Pts',(-0.00229071598306191,-0.0267354590721554,
-0.0111275853827044));
#16516=CARTESIAN_POINT('Ctrl Pts',(-0.00232587061440539,-0.0267412743898821,
-0.0112124571400818));
#16517=CARTESIAN_POINT('Ctrl Pts',(-0.00251111310114769,-0.0267719174054887,
-0.0116596771731171));
#16518=CARTESIAN_POINT('Ctrl Pts',(-0.00256368021268813,-0.0268025604210954,
-0.0121625998300799));
#16519=CARTESIAN_POINT('Ctrl Pts',(-0.00247454555743809,-0.0268332034367019,
-0.0126389197333705));
#16520=CARTESIAN_POINT('Ctrl Pts',(-0.00245762991351471,-0.0268390187544287,
-0.0127293139560785));
#16521=CARTESIAN_POINT('Ctrl Pts',(-0.00243576286496692,-0.0268448340721554,
-0.0128187413173178));
#16522=CARTESIAN_POINT('Ctrl Pts',(-0.00240909508136888,-0.0268506493898821,
-0.0129066522595488));
#16523=CARTESIAN_POINT('Ctrl Pts',(-0.00226852586425637,-0.0268813026557263,
-0.0133700418127002));
#16524=CARTESIAN_POINT('Ctrl Pts',(-0.00198997083433534,-0.0269119559215704,
-0.0137922697976542));
#16525=CARTESIAN_POINT('Ctrl Pts',(-0.00161871280581066,-0.0269426091874145,
-0.0141039547108365));
#16526=CARTESIAN_POINT('Ctrl Pts',(-0.00154840454167825,-0.0269484142549037,
-0.014162981111664));
#16527=CARTESIAN_POINT('Ctrl Pts',(-0.00147489407355667,-0.0269542193223929,
-0.0142181323018698));
#16528=CARTESIAN_POINT('Ctrl Pts',(-0.00139864383421296,-0.0269600243898821,
-0.0142690808601912));
#16529=CARTESIAN_POINT('Ctrl Pts',(-0.000997256604347869,-0.026990582719649,
-0.0145372780601776));
#16530=CARTESIAN_POINT('Ctrl Pts',(-0.000515707761662423,-0.0270211410494158,
-0.014686894119793));
#16531=CARTESIAN_POINT('Ctrl Pts',(-3.25563712997477E-5,-0.0270516993791827,
-0.0146931427678629));
#16532=CARTESIAN_POINT('Ctrl Pts',(6.07273568369965E-5,-0.0270575993827492,
-0.0146943492161923));
#16533=CARTESIAN_POINT('Ctrl Pts',(0.000154031385954281,-0.0270634993863156,
-0.0146903637196954));
#16534=CARTESIAN_POINT('Ctrl Pts',(0.000246760680670542,-0.0270693993898821,
-0.0146812305867816));
#16535=CARTESIAN_POINT('Ctrl Pts',(0.000733989645193602,-0.0271003998696892,
-0.0146332422255406));
#16536=CARTESIAN_POINT('Ctrl Pts',(0.00120721401569154,-0.0271314003494962,
-0.0144388319660053));
#16537=CARTESIAN_POINT('Ctrl Pts',(0.00158787431793346,-0.0271624008293032,
-0.0141294298528711));
#16538=CARTESIAN_POINT('Ctrl Pts',(0.00165489225397286,-0.0271678586828295,
-0.0140749574245502));
#16539=CARTESIAN_POINT('Ctrl Pts',(0.00171909554998313,-0.0271733165363559,
-0.0140170403798492));
#16540=CARTESIAN_POINT('Ctrl Pts',(0.00178014132163675,-0.0271787743898821,
-0.0139559946081956));
#16541=CARTESIAN_POINT('',(0.00251838520168631,-0.027178765100316,-0.0121758301112765));
#16542=CARTESIAN_POINT('Origin',(0.,-0.0271787743898824,-0.0121758532865681));
#16543=CARTESIAN_POINT('',(0.00251749968591618,-0.0261786840658975,-0.0121751178742672));
#16544=CARTESIAN_POINT('Ctrl Pts',(0.00251749999997412,-0.0271787629041013,
-0.0121758647020315));
#16545=CARTESIAN_POINT('Ctrl Pts',(0.00251749778631676,-0.0271478961171008,
-0.0126640514115256));
#16546=CARTESIAN_POINT('Ctrl Pts',(0.00237120877539461,-0.0271170293301002,
-0.0131522185239118));
#16547=CARTESIAN_POINT('Ctrl Pts',(0.00210295040354148,-0.0270861625430997,
-0.0135598351687534));
#16548=CARTESIAN_POINT('Ctrl Pts',(0.00200909565457378,-0.0270753632732563,
-0.0137024467771531));
#16549=CARTESIAN_POINT('Ctrl Pts',(0.00190076493421896,-0.027064564003413,
-0.0138353454145956));
#16550=CARTESIAN_POINT('Ctrl Pts',(0.00178033019948072,-0.0270537647335697,
-0.0139558057103091));
#16551=CARTESIAN_POINT('Ctrl Pts',(0.00144244168384373,-0.0270234665868992,
-0.014293765939144));
#16552=CARTESIAN_POINT('Ctrl Pts',(0.00100394391224188,-0.0269931684402286,
-0.0145337743131699));
#16553=CARTESIAN_POINT('Ctrl Pts',(0.000535447156400708,-0.0269628702935582,
-0.0146357521854363));
#16554=CARTESIAN_POINT('Ctrl Pts',(0.000359664149981759,-0.0269515022333864,
-0.0146740149412649));
#16555=CARTESIAN_POINT('Ctrl Pts',(0.000179926162149245,-0.0269401341732146,
-0.0146933148536184));
#16556=CARTESIAN_POINT('Ctrl Pts',(5.38553941159415E-7,-0.0269287661130429,
-0.0146933532289533));
#16557=CARTESIAN_POINT('Ctrl Pts',(-0.00047933341202766,-0.0268983559111435,
-0.0146934558851377));
#16558=CARTESIAN_POINT('Ctrl Pts',(-0.000960776506469032,-0.0268679457092441,
-0.0145520344873474));
#16559=CARTESIAN_POINT('Ctrl Pts',(-0.00136506763759191,-0.0268375355073446,
-0.0142911302411906));
#16560=CARTESIAN_POINT('Ctrl Pts',(-0.00151471159540945,-0.0268262795024018,
-0.0141945593767794));
#16561=CARTESIAN_POINT('Ctrl Pts',(-0.0016539280448862,-0.0268150234974589,
-0.0140821268795949));
#16562=CARTESIAN_POINT('Ctrl Pts',(-0.00177956848708172,-0.0268037674925161,
-0.0139565672584766));
#16563=CARTESIAN_POINT('Ctrl Pts',(-0.00211894582072311,-0.0267733630074777,
-0.0136174082370379));
#16564=CARTESIAN_POINT('Ctrl Pts',(-0.00235939823293213,-0.0267429585224393,
-0.0131770892179304));
#16565=CARTESIAN_POINT('Ctrl Pts',(-0.00246086496060974,-0.0267125540374009,
-0.0127068428303753));
#16566=CARTESIAN_POINT('Ctrl Pts',(-0.00249844790463954,-0.026701292315597,
-0.0125326651066209));
#16567=CARTESIAN_POINT('Ctrl Pts',(-0.00251742343338017,-0.0266900305937932,
-0.0123546400921435));
#16568=CARTESIAN_POINT('Ctrl Pts',(-0.00251749976773793,-0.0266787688719893,
-0.0121769346927993));
#16569=CARTESIAN_POINT('Ctrl Pts',(-0.00251770585583697,-0.026648364386951,
-0.0116971642589626));
#16570=CARTESIAN_POINT('Ctrl Pts',(-0.0023764459218359,-0.0266179599019128,
-0.0112157750511857));
#16571=CARTESIAN_POINT('Ctrl Pts',(-0.00211571967966154,-0.0265875554168744,
-0.0108114719296447));
#16572=CARTESIAN_POINT('Ctrl Pts',(-0.00201914753240536,-0.0265762936950705,
-0.0106617193759164));
#16573=CARTESIAN_POINT('Ctrl Pts',(-0.00190669394497856,-0.0265650319732665,
-0.0105224001585939));
#16574=CARTESIAN_POINT('Ctrl Pts',(-0.00178109766155855,-0.0265537702514625,
-0.0103966688188902));
#16575=CARTESIAN_POINT('Ctrl Pts',(-0.00144194807119419,-0.0265233600495631,
-0.0100571545339503));
#16576=CARTESIAN_POINT('Ctrl Pts',(-0.00100158616073564,-0.0264929498476636,
-0.00981658502841946));
#16577=CARTESIAN_POINT('Ctrl Pts',(-0.000531261451121286,-0.0264625396457643,
-0.00971504701207152));
#16578=CARTESIAN_POINT('Ctrl Pts',(-0.000357175883597738,-0.0264512836408214,
-0.00967746382148041));
#16579=CARTESIAN_POINT('Ctrl Pts',(-0.000179243606041329,-0.0264400276358785,
-0.0096584684082667));
#16580=CARTESIAN_POINT('Ctrl Pts',(-1.62425849082956E-6,-0.0264287716309357,
-0.00965835381053346));
#16581=CARTESIAN_POINT('Ctrl Pts',(0.000476479391155565,-0.0263984734842652,
-0.00965804534416839));
#16582=CARTESIAN_POINT('Ctrl Pts',(0.000956363372561331,-0.0263681753375946,
-0.00979825490116403));
#16583=CARTESIAN_POINT('Ctrl Pts',(0.00135979315423783,-0.026337877190924,
-0.0100571818095027));
#16584=CARTESIAN_POINT('Ctrl Pts',(0.0015111626120142,-0.0263265091307523,
-0.0101543328565972));
#16585=CARTESIAN_POINT('Ctrl Pts',(0.00165191352108424,-0.0263151410705806,
-0.0102676761223036));
#16586=CARTESIAN_POINT('Ctrl Pts',(0.0017788003655274,-0.0263037730104089,
-0.0103943720181751));
#16587=CARTESIAN_POINT('Ctrl Pts',(0.00212332610501935,-0.0262729062223315,
-0.0107383792902235));
#16588=CARTESIAN_POINT('Ctrl Pts',(0.00236581221928291,-0.026242039434254,
-0.0111861696729781));
#16589=CARTESIAN_POINT('Ctrl Pts',(0.00246503937490897,-0.0262111726461765,
-0.0116645929515541));
#16590=CARTESIAN_POINT('Ctrl Pts',(0.00249975615864945,-0.0262003732274117,
-0.0118319797661205));
#16591=CARTESIAN_POINT('Ctrl Pts',(0.00251735203706798,-0.026189573808647,
-0.0120028834728062));
#16592=CARTESIAN_POINT('Ctrl Pts',(0.00251749906725531,-0.0261787743898821,
-0.0121736861758931));
#16593=CARTESIAN_POINT('',(0.00251749999999575,-0.0251788467684986,-0.0121758579128216));
#16594=CARTESIAN_POINT('Ctrl Pts',(0.00251749999998532,-0.0261786382120571,
-0.0121758446897297));
#16595=CARTESIAN_POINT('Ctrl Pts',(0.00251750166704566,-0.0261478195037794,
-0.0126640275621337));
#16596=CARTESIAN_POINT('Ctrl Pts',(0.00237121873593487,-0.0261169959543789,
-0.0131521924775708));
#16597=CARTESIAN_POINT('Ctrl Pts',(0.00200907480146766,-0.0260753702361943,
-0.0137024822819987));
#16598=CARTESIAN_POINT('Ctrl Pts',(0.00190069385417868,-0.0260645767719191,
-0.0138354341741625));
#16599=CARTESIAN_POINT('Ctrl Pts',(0.00144228680867142,-0.0260235087560348,
-0.0142938712727592));
#16600=CARTESIAN_POINT('Ctrl Pts',(0.00100377153889743,-0.0259932243669049,
-0.0145338478358197));
#16601=CARTESIAN_POINT('Ctrl Pts',(0.000359411550730674,-0.0259515769351503,
-0.0146740564015858));
#16602=CARTESIAN_POINT('Ctrl Pts',(0.000179599669795031,-0.0259402111956357,
-0.0146933431974975));
#16603=CARTESIAN_POINT('Ctrl Pts',(-0.000479728532090669,-0.0258984579692366,
-0.0146933802500336));
#16604=CARTESIAN_POINT('Ctrl Pts',(-0.00096114749117309,-0.02586807788922,
-0.0145518840146613));
#16605=CARTESIAN_POINT('Ctrl Pts',(-0.00151508659768241,-0.0258263868848362,
-0.0141942843912173));
#16606=CARTESIAN_POINT('Ctrl Pts',(-0.001654338303916,-0.0258151146282039,
-0.0140817776069311));
#16607=CARTESIAN_POINT('Ctrl Pts',(-0.00211924827589824,-0.0257733778097309,
-0.0136169416575881));
#16608=CARTESIAN_POINT('Ctrl Pts',(-0.00235957857502316,-0.0257428575514638,
-0.01317663284047));
#16609=CARTESIAN_POINT('Ctrl Pts',(-0.00249853586243591,-0.0257012067465951,
-0.0125321165801073));
#16610=CARTESIAN_POINT('Ctrl Pts',(-0.00251748166317325,-0.0256899602890659,
-0.0123539506799638));
#16611=CARTESIAN_POINT('Ctrl Pts',(-0.00251754944298543,-0.0256484646462054,
-0.0116961150930998));
#16612=CARTESIAN_POINT('Ctrl Pts',(-0.00237600299752491,-0.0256183952459406,
-0.011214565160755));
#16613=CARTESIAN_POINT('Ctrl Pts',(-0.00201834470620797,-0.0255771437662403,
-0.0106606690207983));
#16614=CARTESIAN_POINT('Ctrl Pts',(-0.00190592797971776,-0.0255659996184417,
-0.0105215342469508));
#16615=CARTESIAN_POINT('Ctrl Pts',(-0.00144127506136263,-0.0255246811609478,
-0.0100567496024728));
#16616=CARTESIAN_POINT('Ctrl Pts',(-0.00100104799894205,-0.0254943885822059,
-0.00981639652475952));
#16617=CARTESIAN_POINT('Ctrl Pts',(-0.000356473502259796,-0.0254527640577268,
-0.00967733905413254));
#16618=CARTESIAN_POINT('Ctrl Pts',(-0.000178188622811726,-0.0254414908164709,
-0.00965836961475007));
#16619=CARTESIAN_POINT('Ctrl Pts',(0.000477893330868105,-0.0253999078828381,
-0.00965830945616422));
#16620=CARTESIAN_POINT('Ctrl Pts',(0.000957717586045887,-0.0253695618264971,
-0.00979879622724106));
#16621=CARTESIAN_POINT('Ctrl Pts',(0.00151242291956161,-0.0253277393238667,
-0.0101552654986796));
#16622=CARTESIAN_POINT('Ctrl Pts',(0.00165319052650165,-0.0253163151440836,
-0.0102687717440038));
#16623=CARTESIAN_POINT('Ctrl Pts',(0.00212435153890391,-0.0252738555283969,
-0.0107398935001329));
#16624=CARTESIAN_POINT('Ctrl Pts',(0.00236652028836834,-0.02524275925144,
-0.0111878615075769));
#16625=CARTESIAN_POINT('Ctrl Pts',(0.00250002683427236,-0.0252006894127854,
-0.0118338920753196));
#16626=CARTESIAN_POINT('Ctrl Pts',(0.00251750031409437,-0.0251897718623775,
-0.0120049330891682));
#16627=CARTESIAN_POINT('Ctrl Pts',(0.00251749999999575,-0.0251788467684986,
-0.0121758579128216));
#16628=CARTESIAN_POINT('',(0.00251749969152233,-0.0241788307970502,-0.0121767269583493));
#16629=CARTESIAN_POINT('Ctrl Pts',(0.00251749973514484,-0.0251787743898821,
-0.0121770080790441));
#16630=CARTESIAN_POINT('Ctrl Pts',(0.00251727580147127,-0.0251479127705137,
-0.0126651935935195));
#16631=CARTESIAN_POINT('Ctrl Pts',(0.00237076574137828,-0.0251170511511452,
-0.0131532932779853));
#16632=CARTESIAN_POINT('Ctrl Pts',(0.00210232333480158,-0.0250861895317767,
-0.0135607875254116));
#16633=CARTESIAN_POINT('Ctrl Pts',(0.00200837910505686,-0.0250753891850758,
-0.0137033944022015));
#16634=CARTESIAN_POINT('Ctrl Pts',(0.0018999556107474,-0.025064588838375,
-0.0138362765659917));
#16635=CARTESIAN_POINT('Ctrl Pts',(0.00177942802041401,-0.0250537884916741,
-0.0139567076237136));
#16636=CARTESIAN_POINT('Ctrl Pts',(0.00144137008933471,-0.0250234954869726,
-0.0142944947984056));
#16637=CARTESIAN_POINT('Ctrl Pts',(0.00100275316589472,-0.024993202482271,
-0.0145342805422729));
#16638=CARTESIAN_POINT('Ctrl Pts',(0.000534207011796535,-0.0249629094775695,
-0.0146360218008163));
#16639=CARTESIAN_POINT('Ctrl Pts',(0.000358361691154154,-0.0249515405162017,
-0.0146742052840754));
#16640=CARTESIAN_POINT('Ctrl Pts',(0.000178569011540147,-0.0249401715548339,
-0.0146934145998264));
#16641=CARTESIAN_POINT('Ctrl Pts',(-8.62323990597464E-7,-0.0249288025934661,
-0.0146933531388714));
#16642=CARTESIAN_POINT('Ctrl Pts',(-0.000480731892182397,-0.02489839754428,
-0.0146931887682397));
#16643=CARTESIAN_POINT('Ctrl Pts',(-0.000962094346738138,-0.0248679924950939,
-0.0145515008288072));
#16644=CARTESIAN_POINT('Ctrl Pts',(-0.00136623928899328,-0.0248375874459078,
-0.0142903736707614));
#16645=CARTESIAN_POINT('Ctrl Pts',(-0.00151586660897812,-0.0248263305290246,
-0.0141936960861908));
#16646=CARTESIAN_POINT('Ctrl Pts',(-0.00165505246021516,-0.0248150736121414,
-0.0140811547956854));
#16647=CARTESIAN_POINT('Ctrl Pts',(-0.00178064760153243,-0.0248038166952582,
-0.0139554881842708));
#16648=CARTESIAN_POINT('Ctrl Pts',(-0.00211981764331208,-0.0247734173587111,
-0.0136161251372869));
#16649=CARTESIAN_POINT('Ctrl Pts',(-0.0023600027298034,-0.024743018022164,
-0.0131756626469667));
#16650=CARTESIAN_POINT('Ctrl Pts',(-0.00246118512021359,-0.024712618685617,
-0.012705356878651));
#16651=CARTESIAN_POINT('Ctrl Pts',(-0.00249867211522085,-0.0247013560560947,
-0.0125311136144103));
#16652=CARTESIAN_POINT('Ctrl Pts',(-0.0025175401703522,-0.0246900934265724,
-0.0123530324036204));
#16653=CARTESIAN_POINT('Ctrl Pts',(-0.00251749993550441,-0.0246788307970502,
-0.0121752834310746));
#16654=CARTESIAN_POINT('Ctrl Pts',(-0.00251739133629353,-0.0246484314605032,
-0.0116955152893069));
#16655=CARTESIAN_POINT('Ctrl Pts',(-0.00237581698877943,-0.0246180321239562,
-0.0112142206619956));
#16656=CARTESIAN_POINT('Ctrl Pts',(-0.00211482758018363,-0.0245876327874092,
-0.0108100895602516));
#16657=CARTESIAN_POINT('Ctrl Pts',(-0.00201813379169509,-0.0245763701578869,
-0.010660363303221));
#16658=CARTESIAN_POINT('Ctrl Pts',(-0.00190555753629768,-0.0245651075283645,
-0.0105210859285633));
#16659=CARTESIAN_POINT('Ctrl Pts',(-0.0017798417509926,-0.0245538448988422,
-0.0103954124446811));
#16660=CARTESIAN_POINT('Ctrl Pts',(-0.00144045434345245,-0.0245234398496561,
-0.0100561392357694));
#16661=CARTESIAN_POINT('Ctrl Pts',(-0.000999925048114809,-0.0244930348004701,
-0.00981588090801228));
#16662=CARTESIAN_POINT('Ctrl Pts',(-0.000529530905128816,-0.0244626297512839,
-0.00971467404267653));
#16663=CARTESIAN_POINT('Ctrl Pts',(-0.000355376022578128,-0.0244513728344007,
-0.00967720404010807));
#16664=CARTESIAN_POINT('Ctrl Pts',(-0.00017738560890287,-0.0244401159175175,
-0.00965833372630848));
#16665=CARTESIAN_POINT('Ctrl Pts',(2.77386968701596E-7,-0.0244288590006343,
-0.00965835330183983));
#16666=CARTESIAN_POINT('Ctrl Pts',(0.000478378631302506,-0.0243985659959327,
-0.00965840598071002));
#16667=CARTESIAN_POINT('Ctrl Pts',(0.000958154594833885,-0.0243682729912311,
-0.00979897658696198));
#16668=CARTESIAN_POINT('Ctrl Pts',(0.00136138767051821,-0.0243379799865295,
-0.0100582060400694));
#16669=CARTESIAN_POINT('Ctrl Pts',(0.001512720999939,-0.0243266110251618,
-0.0101554948256089));
#16670=CARTESIAN_POINT('Ctrl Pts',(0.00165341835785117,-0.0243152420637941,
-0.0102689757919928));
#16671=CARTESIAN_POINT('Ctrl Pts',(0.00178023405819179,-0.0243038731024263,
-0.010395804706307));
#16672=CARTESIAN_POINT('Ctrl Pts',(0.00212448167653426,-0.0242730114830577,
-0.0107400881946476));
#16673=CARTESIAN_POINT('Ctrl Pts',(0.00236660703117265,-0.0242421498636891,
-0.011188072299693));
#16674=CARTESIAN_POINT('Ctrl Pts',(0.00246544945886431,-0.0242112882443205,
-0.0116665741727259));
#16675=CARTESIAN_POINT('Ctrl Pts',(0.00250004040093587,-0.0242004878976197,
-0.0118340309112719));
#16676=CARTESIAN_POINT('Ctrl Pts',(0.00251749897647234,-0.0241896875509191,
-0.0120049925568173));
#16677=CARTESIAN_POINT('Ctrl Pts',(0.00251749999995483,-0.0241788872042183,
-0.0121758382050082));
#16678=CARTESIAN_POINT('',(0.00251749961839117,-0.0231787088666403,-0.0121748943155386));
#16679=CARTESIAN_POINT('Ctrl Pts',(0.00251749938308983,-0.0241787743898821,
-0.0121776157116905));
#16680=CARTESIAN_POINT('Ctrl Pts',(0.00251715761715276,-0.0241479040557949,
-0.0126658041288309));
#16681=CARTESIAN_POINT('Ctrl Pts',(0.00237052806672346,-0.0241170337217076,
-0.0131538709062047));
#16682=CARTESIAN_POINT('Ctrl Pts',(0.00210198450028724,-0.0240861633876204,
-0.0135613017376209));
#16683=CARTESIAN_POINT('Ctrl Pts',(0.00200806631828363,-0.024075367055041,
-0.013703793190634));
#16684=CARTESIAN_POINT('Ctrl Pts',(0.00189969006379212,-0.0240645707224615,
-0.0138365690828121));
#16685=CARTESIAN_POINT('Ctrl Pts',(0.0017792267323238,-0.0240537743898821,
-0.0139569087278581));
#16686=CARTESIAN_POINT('Ctrl Pts',(0.00144112599332246,-0.0240234726542492,
-0.0142946623199701));
#16687=CARTESIAN_POINT('Ctrl Pts',(0.00100247575010198,-0.0239931709186162,
-0.0145343995217319));
#16688=CARTESIAN_POINT('Ctrl Pts',(0.000533912379734766,-0.0239628691829833,
-0.0146360857594691));
#16689=CARTESIAN_POINT('Ctrl Pts',(0.000358173588608443,-0.0239515042519495,
-0.0146742240725006));
#16690=CARTESIAN_POINT('Ctrl Pts',(0.000178494707472031,-0.0239401393209158,
-0.0146934118272028));
#16691=CARTESIAN_POINT('Ctrl Pts',(-8.23759858439146E-7,-0.0239287743898821,
-0.0146933531517854));
#16692=CARTESIAN_POINT('Ctrl Pts',(-0.000480699474097822,-0.0238983605988304,
-0.0146931961299894));
#16693=CARTESIAN_POINT('Ctrl Pts',(-0.000962068926494477,-0.0238679468077788,
-0.0145515121105112));
#16694=CARTESIAN_POINT('Ctrl Pts',(-0.0013662203064985,-0.0238375330167271,
-0.0142903859356584));
#16695=CARTESIAN_POINT('Ctrl Pts',(-0.00151575329964231,-0.0238262801411121,
-0.0141937712005719));
#16696=CARTESIAN_POINT('Ctrl Pts',(-0.00165485831852499,-0.023815027265497,
-0.0140813129275911));
#16697=CARTESIAN_POINT('Ctrl Pts',(-0.00178039192185105,-0.0238037743898821,
-0.013955743972698));
#16698=CARTESIAN_POINT('Ctrl Pts',(-0.00211961493681556,-0.0237733663215084,
-0.0136164254290078));
#16699=CARTESIAN_POINT('Ctrl Pts',(-0.00235986424518859,-0.0237429582531347,
-0.0131759917540072));
#16700=CARTESIAN_POINT('Ctrl Pts',(-0.00246111229587264,-0.023712550184761,
-0.0127056952602677));
#16701=CARTESIAN_POINT('Ctrl Pts',(-0.00249859942318996,-0.0237012915864681,
-0.012531567813679));
#16702=CARTESIAN_POINT('Ctrl Pts',(-0.00251749188956349,-0.023690032988175,
-0.0123536047447747));
#16703=CARTESIAN_POINT('Ctrl Pts',(-0.0025174999973777,-0.0236787743898821,
-0.0121759681920881));
#16704=CARTESIAN_POINT('Ctrl Pts',(-0.00251752189557162,-0.0236483663215085,
-0.0116961940408852));
#16705=CARTESIAN_POINT('Ctrl Pts',(-0.00237607509735981,-0.0236179582531348,
-0.011214856218412));
#16706=CARTESIAN_POINT('Ctrl Pts',(-0.00211519055100145,-0.0235875501847612,
-0.0108106517692156));
#16707=CARTESIAN_POINT('Ctrl Pts',(-0.00201859795352949,-0.0235762915864682,
-0.0106609949259775));
#16708=CARTESIAN_POINT('Ctrl Pts',(-0.0019061403672986,-0.0235650329881751,
-0.0105217694096613));
#16709=CARTESIAN_POINT('Ctrl Pts',(-0.00178055439251249,-0.0235537743898821,
-0.0103961251316691));
#16710=CARTESIAN_POINT('Ctrl Pts',(-0.00144129851920226,-0.0235233605988305,
-0.0100567117590432));
#16711=CARTESIAN_POINT('Ctrl Pts',(-0.0010008596088619,-0.0234929468077789,
-0.0098162761052494));
#16712=CARTESIAN_POINT('Ctrl Pts',(-0.0005305006030715,-0.0234625330167273,
-0.00971488287630511));
#16713=CARTESIAN_POINT('Ctrl Pts',(-0.000356471282701629,-0.0234512801411122,
-0.00967736813861314));
#16714=CARTESIAN_POINT('Ctrl Pts',(-0.000178603996301796,-0.0234400272654971,
-0.00965842781167594));
#16715=CARTESIAN_POINT('Ctrl Pts',(-1.0535709026251E-6,-0.0234287743898821,
-0.00965835350701722));
#16716=CARTESIAN_POINT('Ctrl Pts',(0.000477054091173907,-0.0233984726542492,
-0.00965815341948388));
#16717=CARTESIAN_POINT('Ctrl Pts',(0.000956909392876984,-0.0233681709186163,
-0.00979847396983194));
#16718=CARTESIAN_POINT('Ctrl Pts',(0.00136028205916767,-0.0233378691829834,
-0.0100574956752218));
#16719=CARTESIAN_POINT('Ctrl Pts',(0.00151157050643154,-0.0233265042519496,
-0.0101546440317934));
#16720=CARTESIAN_POINT('Ctrl Pts',(0.00165224493730612,-0.0233151393209159,
-0.0102679695719795));
#16721=CARTESIAN_POINT('Ctrl Pts',(0.00177906414050594,-0.0233037743898821,
-0.0103946354352087));
#16722=CARTESIAN_POINT('Ctrl Pts',(0.00212354059705622,-0.0232729040557949,
-0.0107386953774739));
#16723=CARTESIAN_POINT('Ctrl Pts',(0.00236596066449794,-0.0232420337217078,
-0.0111865238080445));
#16724=CARTESIAN_POINT('Ctrl Pts',(0.0024651162146737,-0.0232111633876205,
-0.0116649635742397));
#16725=CARTESIAN_POINT('Ctrl Pts',(0.00249979404788967,-0.0232003670550411,
-0.0118322890984952));
#16726=CARTESIAN_POINT('Ctrl Pts',(0.00251736409974424,-0.0231895707224615,
-0.0120031261261098));
#16727=CARTESIAN_POINT('Ctrl Pts',(0.0025174992117169,-0.0231787743898821,
-0.0121738610504294));
#16728=CARTESIAN_POINT('Ctrl Pts',(0.00251749999997788,-0.0231786473855,
-0.0121758638389549));
#16729=CARTESIAN_POINT('Ctrl Pts',(0.00251749795369238,-0.0231477868810446,
-0.0126640490203062));
#16730=CARTESIAN_POINT('Ctrl Pts',(0.00237120997493988,-0.0231169263765892,
-0.0131522149255864));
#16731=CARTESIAN_POINT('Ctrl Pts',(0.0021029531720672,-0.0230860658721338,
-0.0135598309619895));
#16732=CARTESIAN_POINT('Ctrl Pts',(0.00200906595270055,-0.0230752650017718,
-0.0137024925303722));
#16733=CARTESIAN_POINT('Ctrl Pts',(0.00190069260959032,-0.0230644641314098,
-0.0138354343323198));
#16734=CARTESIAN_POINT('Ctrl Pts',(0.00178020769704895,-0.0230536632610477,
-0.0139559282303084));
#16735=CARTESIAN_POINT('Ctrl Pts',(0.00144229831669849,-0.0230233713735881,
-0.01429386281105));
#16736=CARTESIAN_POINT('Ctrl Pts',(0.00100378724406002,-0.0229930794861285,
-0.0145338404708914));
#16737=CARTESIAN_POINT('Ctrl Pts',(0.000535286428431861,-0.0229627875986689,
-0.0146357871656566));
#16738=CARTESIAN_POINT('Ctrl Pts',(0.000359443503242876,-0.0229514181113111,
-0.0146740509304631));
#16739=CARTESIAN_POINT('Ctrl Pts',(0.000179644245441134,-0.0229400486239533,
-0.0146933391444727));
#16740=CARTESIAN_POINT('Ctrl Pts',(1.98293912005771E-7,-0.0229286791365955,
-0.0146933532787487));
#16741=CARTESIAN_POINT('Ctrl Pts',(-0.000479670505837759,-0.0228982752060211,
-0.0146933910761913));
#16742=CARTESIAN_POINT('Ctrl Pts',(-0.00096109198559297,-0.0228678712754467,
-0.0145519063931369));
#16743=CARTESIAN_POINT('Ctrl Pts',(-0.0013653465885999,-0.0228374673448723,
-0.0142909501975763));
#16744=CARTESIAN_POINT('Ctrl Pts',(-0.00151502702686396,-0.0228262099006293,
-0.0141943278278402));
#16745=CARTESIAN_POINT('Ctrl Pts',(-0.00165427096627102,-0.0228149524563863,
-0.0140818347223467));
#16746=CARTESIAN_POINT('Ctrl Pts',(-0.00177992725547758,-0.0228036950121433,
-0.0139562086486159));
#16747=CARTESIAN_POINT('Ctrl Pts',(-0.00211923405946871,-0.0227732967929111,
-0.0136169834347829));
#16748=CARTESIAN_POINT('Ctrl Pts',(-0.00235959725416242,-0.022742898573679,
-0.0131766189178827));
#16749=CARTESIAN_POINT('Ctrl Pts',(-0.0024609702103146,-0.0227125003544468,
-0.0127063548171347));
#16750=CARTESIAN_POINT('Ctrl Pts',(-0.00249853094269033,-0.0227012371988616,
-0.0125321124481187));
#16751=CARTESIAN_POINT('Ctrl Pts',(-0.00251747121844593,-0.0226899740432763,
-0.0123540239500127));
#16752=CARTESIAN_POINT('Ctrl Pts',(-0.00251749996707782,-0.022678710887691,
-0.0121762604267775));
#16753=CARTESIAN_POINT('Ctrl Pts',(-0.00251757755698666,-0.0226483126684587,
-0.0116964930551988));
#16754=CARTESIAN_POINT('Ctrl Pts',(-0.00237619043761343,-0.0226179144492263,
-0.0112151441306248));
#16755=CARTESIAN_POINT('Ctrl Pts',(-0.00211535854080719,-0.022587516229994,
-0.0108109120812917));
#16756=CARTESIAN_POINT('Ctrl Pts',(-0.00201871504294884,-0.0225762530744089,
-0.0106611359240335));
#16757=CARTESIAN_POINT('Ctrl Pts',(-0.00190618239367656,-0.0225649899188239,
-0.0105218041976827));
#16758=CARTESIAN_POINT('Ctrl Pts',(-0.0017805030148144,-0.0225537267632388,
-0.0103960737316028));
#16759=CARTESIAN_POINT('Ctrl Pts',(-0.00144124222056347,-0.0225233228326644,
-0.0100566750317524));
#16760=CARTESIAN_POINT('Ctrl Pts',(-0.00100080296046634,-0.0224929189020899,
-0.00981625320281795));
#16761=CARTESIAN_POINT('Ctrl Pts',(-0.000530447146739297,-0.0224625149715155,
-0.00971487135356547));
#16762=CARTESIAN_POINT('Ctrl Pts',(-0.000356291889594958,-0.0224512575272725,
-0.00967733342693407));
#16763=CARTESIAN_POINT('Ctrl Pts',(-0.000178293543672711,-0.0224400000830296,
-0.0096583968363908));
#16764=CARTESIAN_POINT('Ctrl Pts',(-6.15986524236793E-7,-0.0224287426387866,
-0.00965835336191846));
#16765=CARTESIAN_POINT('Ctrl Pts',(0.000477484410783648,-0.022398450751327,
-0.00965823637943155));
#16766=CARTESIAN_POINT('Ctrl Pts',(0.000957309569357418,-0.0223681588638674,
-0.00979863625329785));
#16767=CARTESIAN_POINT('Ctrl Pts',(0.00136063427525223,-0.0223378669764078,
-0.0100577218886017));
#16768=CARTESIAN_POINT('Ctrl Pts',(0.00151201457966164,-0.02232649748905,
-0.0101549647843806));
#16769=CARTESIAN_POINT('Ctrl Pts',(0.00165276292502887,-0.0223151280016921,
-0.0102684063031234));
#16770=CARTESIAN_POINT('Ctrl Pts',(0.00177963184218455,-0.0223037585143343,
-0.0103952026312405));
#16771=CARTESIAN_POINT('Ctrl Pts',(0.00212399554653551,-0.0222728980098791,
-0.0107393693052175));
#16772=CARTESIAN_POINT('Ctrl Pts',(0.00236627236577061,-0.0222420375054239,
-0.01118727103047));
#16773=CARTESIAN_POINT('Ctrl Pts',(0.0024652768054868,-0.0222111770009687,
-0.0116657390617723));
#16774=CARTESIAN_POINT('Ctrl Pts',(0.00249992737706798,-0.0222003761306065,
-0.0118331981253807));
#16775=CARTESIAN_POINT('Ctrl Pts',(0.00251744388437495,-0.0221895752602443,
-0.0120041684931912));
#16776=CARTESIAN_POINT('Ctrl Pts',(0.00251749986487603,-0.0221787743898821,
-0.0121750284537333));
#16777=CARTESIAN_POINT('',(-0.00251750000001,-0.00883413153273949,-0.012175853286568));
#16778=CARTESIAN_POINT('Origin',(0.,-0.00883413153273949,-0.012175853286568));
#16779=CARTESIAN_POINT('Origin',(0.,0.0154212256101276,-0.012175853286558));
#16780=CARTESIAN_POINT('',(0.004,0.0153212256101276,-0.012175853286558));
#16781=CARTESIAN_POINT('Origin',(0.,0.0153212256101176,-0.012175853286568));
#16782=CARTESIAN_POINT('',(0.0042,0.0155212256101276,-0.012175853286558));
#16783=CARTESIAN_POINT('',(0.0041,0.0154212256101276,-0.012175853286558));
#16784=CARTESIAN_POINT('Origin',(0.,0.0155212256101176,-0.012175853286568));
#16785=CARTESIAN_POINT('Origin',(0.,0.0155212256101276,-0.012175853286558));
#16786=CARTESIAN_POINT('',(-0.0078,0.0155212256101276,-0.012175853286558));
#16787=CARTESIAN_POINT('Origin',(0.,0.0155212256101176,-0.012175853286568));
#16788=CARTESIAN_POINT('Origin',(0.,0.0155212256101279,-0.012175853286558));
#16789=CARTESIAN_POINT('',(0.004,0.00902122561010792,-0.012175853286558));
#16790=CARTESIAN_POINT('',(0.004,0.0155212256101279,-0.012175853286558));
#16791=CARTESIAN_POINT('',(-0.00400000000001,0.00902122561011792,-0.012175853286568));
#16792=CARTESIAN_POINT('Origin',(0.,0.00902122561011792,-0.012175853286568));
#16793=CARTESIAN_POINT('Origin',(0.,0.00902122561011792,-0.012175853286568));
#16794=CARTESIAN_POINT('Origin',(0.,0.0119212256101276,-0.012175853286558));
#16795=CARTESIAN_POINT('',(-0.008,0.0120212256101276,-0.012175853286558));
#16796=CARTESIAN_POINT('Origin',(0.,0.0120212256101176,-0.012175853286568));
#16797=CARTESIAN_POINT('',(-0.0078,0.0118212256101276,-0.012175853286558));
#16798=CARTESIAN_POINT('',(-0.0079,0.0119212256101276,-0.012175853286558));
#16799=CARTESIAN_POINT('Origin',(0.,0.0118212256101176,-0.012175853286568));
#16800=CARTESIAN_POINT('Origin',(0.,0.0188212256101277,-0.012175853286558));
#16801=CARTESIAN_POINT('',(-0.008,0.0153212256101276,-0.012175853286558));
#16802=CARTESIAN_POINT('',(-0.008,0.0188212256101277,-0.012175853286558));
#16803=CARTESIAN_POINT('Origin',(0.,0.0153212256101176,-0.012175853286568));
#16804=CARTESIAN_POINT('Origin',(0.,0.0118212256101276,-0.012175853286558));
#16805=CARTESIAN_POINT('',(0.006,0.0118212256101276,-0.012175853286558));
#16806=CARTESIAN_POINT('Origin',(0.,0.0118212256101176,-0.012175853286568));
#16807=CARTESIAN_POINT('Origin',(0.,0.0154212256101276,-0.012175853286558));
#16808=CARTESIAN_POINT('',(-0.0079,0.0154212256101276,-0.012175853286558));
#16809=CARTESIAN_POINT('Origin',(0.,0.00807122561012792,-0.012175853286558));
#16810=CARTESIAN_POINT('',(0.00210000000001,0.00712122561011792,-0.012175853286568));
#16811=CARTESIAN_POINT('',(-0.0021,0.00712122561012792,-0.012175853286558));
#16812=CARTESIAN_POINT('Origin',(0.,0.00712122561011792,-0.012175853286568));
#16813=CARTESIAN_POINT('',(-0.00305,0.00807122561012792,-0.012175853286558));
#16814=CARTESIAN_POINT('Origin',(0.,0.00712122561011792,-0.012175853286568));
#16815=CARTESIAN_POINT('Origin',(0.,0.0155212256101279,-0.012175853286558));
#16816=CARTESIAN_POINT('',(0.0021,-0.00853591724703519,-0.012175853286558));
#16817=CARTESIAN_POINT('',(0.0021,0.0155212256101279,-0.012175853286558));
#16818=CARTESIAN_POINT('',(-0.00210000000001,-0.00853591724702519,-0.012175853286568));
#16819=CARTESIAN_POINT('Origin',(0.,-0.00853591724702519,-0.012175853286568));
#16820=CARTESIAN_POINT('Origin',(0.,-0.00853591724702519,-0.012175853286568));
#16821=CARTESIAN_POINT('Origin',(3.42660592399111E-19,-0.0131787743898721,
-0.012175853286558));
#16822=CARTESIAN_POINT('Ctrl Pts',(0.00251750000000276,-0.0131787743898705,
-0.0121758532865581));
#16823=CARTESIAN_POINT('Ctrl Pts',(0.00252678255386265,-0.0131787743898701,
-0.0120910805509574));
#16824=CARTESIAN_POINT('Ctrl Pts',(0.00253138326894594,-0.0131787743898702,
-0.0120060302520078));
#16825=CARTESIAN_POINT('Ctrl Pts',(0.00253153840791565,-0.0131787743898704,
-0.011920995628507));
#16826=CARTESIAN_POINT('Ctrl Pts',(0.00253173885754197,-0.0131787743898706,
-0.0118111253713033));
#16827=CARTESIAN_POINT('Ctrl Pts',(0.00252452176116332,-0.0131787743898709,
-0.0117012808905388));
#16828=CARTESIAN_POINT('Ctrl Pts',(0.00251027895179543,-0.0131787743898711,
-0.01159205956687));
#16829=CARTESIAN_POINT('Ctrl Pts',(0.00250787645068956,-0.0131787743898711,
-0.0115736359297827));
#16830=CARTESIAN_POINT('Ctrl Pts',(0.0025052735027393,-0.0131787743898712,
-0.0115552290376494));
#16831=CARTESIAN_POINT('Ctrl Pts',(0.00250247449001427,-0.0131787743898712,
-0.0115368584649061));
#16832=CARTESIAN_POINT('Ctrl Pts',(0.0024778848322329,-0.0131787743898716,
-0.0113754708109787));
#16833=CARTESIAN_POINT('Ctrl Pts',(0.00243817399752059,-0.0131787743898719,
-0.0112165929618383));
#16834=CARTESIAN_POINT('Ctrl Pts',(0.00238459006941217,-0.0131787743898722,
-0.0110621287890247));
#16835=CARTESIAN_POINT('Ctrl Pts',(0.00237038445925664,-0.0131787743898723,
-0.0110211788643095));
#16836=CARTESIAN_POINT('Ctrl Pts',(0.00235519109693126,-0.0131787743898724,
-0.0109805154528752));
#16837=CARTESIAN_POINT('Ctrl Pts',(0.00233906126070756,-0.0131787743898725,
-0.0109402583288236));
#16838=CARTESIAN_POINT('Ctrl Pts',(0.00223492121084125,-0.0131787743898731,
-0.0106803437923044));
#16839=CARTESIAN_POINT('Ctrl Pts',(0.00209239429727179,-0.0131787743898737,
-0.0104379417852556));
#16840=CARTESIAN_POINT('Ctrl Pts',(0.0019166248406654,-0.0131787743898743,
-0.0102221995812248));
#16841=CARTESIAN_POINT('Ctrl Pts',(0.00188608523662504,-0.0131787743898744,
-0.0101847147894236));
#16842=CARTESIAN_POINT('Ctrl Pts',(0.0018545322737917,-0.0131787743898745,
-0.0101480373230837));
#16843=CARTESIAN_POINT('Ctrl Pts',(0.00182198107674273,-0.0131787743898746,
-0.0101122201309508));
#16844=CARTESIAN_POINT('Ctrl Pts',(0.00180781807866736,-0.0131787743898747,
-0.0100966361011997));
#16845=CARTESIAN_POINT('Ctrl Pts',(0.00179346144536564,-0.0131787743898747,
-0.0100812103074837));
#16846=CARTESIAN_POINT('Ctrl Pts',(0.00177893734013724,-0.0131787743898748,
-0.0100659730452282));
#16847=CARTESIAN_POINT('Ctrl Pts',(0.00171287262328748,-0.013178774389875,
-0.0099966644440688));
#16848=CARTESIAN_POINT('Ctrl Pts',(0.00164327513476541,-0.0131787743898752,
-0.00993117167958241));
#16849=CARTESIAN_POINT('Ctrl Pts',(0.00157035138407573,-0.0131787743898754,
-0.00986983987978509));
#16850=CARTESIAN_POINT('Ctrl Pts',(0.00155126698510032,-0.0131787743898755,
-0.00985378913464181));
#16851=CARTESIAN_POINT('Ctrl Pts',(0.00153195451165503,-0.0131787743898756,
-0.00983802345570631));
#16852=CARTESIAN_POINT('Ctrl Pts',(0.00151241711792581,-0.0131787743898756,
-0.00982254925039919));
#16853=CARTESIAN_POINT('Ctrl Pts',(0.00133945071125891,-0.0131787743898762,
-0.00968555463765327));
#16854=CARTESIAN_POINT('Ctrl Pts',(0.00114895456192055,-0.0131787743898767,
-0.00957130583923114));
#16855=CARTESIAN_POINT('Ctrl Pts',(0.000945893407857157,-0.0131787743898771,
-0.00947984027712986));
#16856=CARTESIAN_POINT('Ctrl Pts',(0.00092821365265431,-0.0131787743898771,
-0.00947187672174231));
#16857=CARTESIAN_POINT('Ctrl Pts',(0.000910433722123745,-0.0131787743898772,
-0.00946408495197249));
#16858=CARTESIAN_POINT('Ctrl Pts',(0.0008925836998557,-0.0131787743898772,
-0.00945647668080864));
#16859=CARTESIAN_POINT('Ctrl Pts',(0.000622478384141858,-0.0131787743898778,
-0.0093413488420928));
#16860=CARTESIAN_POINT('Ctrl Pts',(0.000335493839089116,-0.0131787743898777,
-0.00926745536012451));
#16861=CARTESIAN_POINT('Ctrl Pts',(4.26963611125967E-5,-0.0131787743898794,
-0.00923485885680396));
#16862=CARTESIAN_POINT('Ctrl Pts',(-1.2995058917788E-5,-0.0131787743898797,
-0.00922865885272438));
#16863=CARTESIAN_POINT('Ctrl Pts',(-6.890315766291E-5,-0.0131787743898796,
-0.00922396320906305));
#16864=CARTESIAN_POINT('Ctrl Pts',(-0.000124958449797895,-0.0131787743898795,
-0.00922078757979583));
#16865=CARTESIAN_POINT('Ctrl Pts',(-0.000141877207563949,-0.0131787743898795,
-0.00921982910290131));
#16866=CARTESIAN_POINT('Ctrl Pts',(-0.00015880937860213,-0.0131787743898795,
-0.00921900913120467));
#16867=CARTESIAN_POINT('Ctrl Pts',(-0.000175753060180348,-0.0131787743898794,
-0.00921832819105194));
#16868=CARTESIAN_POINT('Ctrl Pts',(-0.000190844981741937,-0.0131787743898794,
-0.00921772167024798));
#16869=CARTESIAN_POINT('Ctrl Pts',(-0.000205937547985643,-0.0131787743898794,
-0.00921722581492978));
#16870=CARTESIAN_POINT('Ctrl Pts',(-0.000221025143038285,-0.0131787743898794,
-0.00921684070026162));
#16871=CARTESIAN_POINT('Ctrl Pts',(-0.000581851158293263,-0.0131787743898789,
-0.00920763052523738));
#16872=CARTESIAN_POINT('Ctrl Pts',(-0.000940457786385863,-0.0131787743898784,
-0.00926106964733248));
#16873=CARTESIAN_POINT('Ctrl Pts',(-0.00127835860631399,-0.0131787743898775,
-0.00937986338687581));
#16874=CARTESIAN_POINT('Ctrl Pts',(-0.00129490141823496,-0.0131787743898775,
-0.00938567924281564));
#16875=CARTESIAN_POINT('Ctrl Pts',(-0.0013113946141123,-0.0131787743898372,
-0.00939165340181671));
#16876=CARTESIAN_POINT('Ctrl Pts',(-0.00132783707045352,-0.0131787743898773,
-0.00939778432924211));
#16877=CARTESIAN_POINT('Ctrl Pts',(-0.00289832479094294,-0.0131787743898724,
-0.0131986512412907));
#16878=CARTESIAN_POINT('Ctrl Pts',(-0.00285634487132818,-0.0131787743898806,
-0.0132905010317887));
#16879=CARTESIAN_POINT('Ctrl Pts',(-0.00280954766287239,-0.0131787743898807,
-0.0133799217860521));
#16880=CARTESIAN_POINT('Ctrl Pts',(-0.00275827179947781,-0.0131787743898807,
-0.0134666993224125));
#16881=CARTESIAN_POINT('Ctrl Pts',(-0.00269168072014957,-0.0131787743898808,
-0.0135793958120498));
#16882=CARTESIAN_POINT('Ctrl Pts',(-0.0026175373870451,-0.0131787743898809,
-0.0136876390597102));
#16883=CARTESIAN_POINT('Ctrl Pts',(-0.00253649519800816,-0.0131787743898809,
-0.0137908693804752));
#16884=CARTESIAN_POINT('Ctrl Pts',(-0.00252207060914627,-0.013178774389881,
-0.0138092432046871));
#16885=CARTESIAN_POINT('Ctrl Pts',(-0.00250742540379288,-0.013178774389881,
-0.0138274599974619));
#16886=CARTESIAN_POINT('Ctrl Pts',(-0.0024925785367831,-0.013178774389881,
-0.0138454979317755));
#16887=CARTESIAN_POINT('Ctrl Pts',(-0.00235107495916407,-0.013178774389881,
-0.0140174151609494));
#16888=CARTESIAN_POINT('Ctrl Pts',(-0.00219103071556285,-0.013178774389881,
-0.0141735316821853));
#16889=CARTESIAN_POINT('Ctrl Pts',(-0.0020156919207918,-0.013178774389881,
-0.0143109630813275));
#16890=CARTESIAN_POINT('Ctrl Pts',(-0.00200226753649631,-0.013178774389881,
-0.0143214851789543));
#16891=CARTESIAN_POINT('Ctrl Pts',(-0.00198875967272646,-0.013178774389881,
-0.0143318921255368));
#16892=CARTESIAN_POINT('Ctrl Pts',(-0.00197517451207161,-0.013178774389881,
-0.0143421793166972));
#16893=CARTESIAN_POINT('Ctrl Pts',(-0.00170331817561905,-0.0131787743898808,
-0.0145480390906311));
#16894=CARTESIAN_POINT('Ctrl Pts',(-0.00140009528713672,-0.0131787743898807,
-0.0147070178556508));
#16895=CARTESIAN_POINT('Ctrl Pts',(-0.00107703637109689,-0.0131787743898803,
-0.0148072378106216));
#16896=CARTESIAN_POINT('Ctrl Pts',(-0.00105976329426689,-0.0131787743898803,
-0.0148125962975605));
#16897=CARTESIAN_POINT('Ctrl Pts',(-0.00104243331187472,-0.0131787743898803,
-0.0148177848787372));
#16898=CARTESIAN_POINT('Ctrl Pts',(-0.00102504817405061,-0.0131787743898803,
-0.0148228010530932));
#16899=CARTESIAN_POINT('Ctrl Pts',(-0.0010118795244946,-0.0131787743898803,
-0.0148266006342569));
#16900=CARTESIAN_POINT('Ctrl Pts',(-0.000998688467597784,-0.0131787743898803,
-0.0148302986272678));
#16901=CARTESIAN_POINT('Ctrl Pts',(-0.000985476138224112,-0.0131787743898802,
-0.0148338942747791));
#16902=CARTESIAN_POINT('Ctrl Pts',(-0.000895925317347755,-0.0131787743898801,
-0.0148582649347222));
#16903=CARTESIAN_POINT('Ctrl Pts',(-0.00080539262624515,-0.01317877438988,
-0.0148779396012878));
#16904=CARTESIAN_POINT('Ctrl Pts',(-0.000714119979602021,-0.0131787743898799,
-0.0148926845173722));
#16905=CARTESIAN_POINT('Ctrl Pts',(-0.00069085444230266,-0.0131787743898799,
-0.0148964430190455));
#16906=CARTESIAN_POINT('Ctrl Pts',(-0.000667540798596598,-0.0131787743898798,
-0.0148998809501044));
#16907=CARTESIAN_POINT('Ctrl Pts',(-0.000644183020312907,-0.0131787743898798,
-0.0149029938915827));
#16908=CARTESIAN_POINT('Ctrl Pts',(-0.000452732095770299,-0.0131787743898795,
-0.0149285089691225));
#16909=CARTESIAN_POINT('Ctrl Pts',(-0.000258294496493731,-0.0131787743898793,
-0.0149322619746447));
#16910=CARTESIAN_POINT('Ctrl Pts',(-6.4245464843163E-5,-0.0131787743898789,
-0.0149152588842441));
#16911=CARTESIAN_POINT('Ctrl Pts',(-3.38914616751708E-5,-0.0131787743898788,
-0.0149125991860457));
#16912=CARTESIAN_POINT('Ctrl Pts',(-3.54767595355644E-6,-0.0131787743898787,
-0.0149094299724371));
#16913=CARTESIAN_POINT('Ctrl Pts',(2.6772004479569E-5,-0.0131787743898794,
-0.0149057533493354));
#16914=CARTESIAN_POINT('Ctrl Pts',(4.04780385078073E-5,-0.0131787743898798,
-0.0149040913291353));
#16915=CARTESIAN_POINT('Ctrl Pts',(5.41779522435996E-5,-0.0131787743898798,
-0.0149023256959705));
#16916=CARTESIAN_POINT('Ctrl Pts',(6.78581592279457E-5,-0.0131787743898798,
-0.0149004585336354));
#16917=CARTESIAN_POINT('Ctrl Pts',(0.000342411697294035,-0.0131787743898801,
-0.0148629857069577));
#16918=CARTESIAN_POINT('Ctrl Pts',(0.000610525518463131,-0.0131787743898805,
-0.014784763374177));
#16919=CARTESIAN_POINT('Ctrl Pts',(0.000862044456775896,-0.0131787743898807,
-0.0146687404422175));
#16920=CARTESIAN_POINT('Ctrl Pts',(0.000905520526633452,-0.0131787743898807,
-0.0146486854072814));
#16921=CARTESIAN_POINT('Ctrl Pts',(0.000948494845706522,-0.0131787743898808,
-0.0146274928944177));
#16922=CARTESIAN_POINT('Ctrl Pts',(0.000990905948759799,-0.0131787743898808,
-0.0146051688505092));
#16923=CARTESIAN_POINT('Ctrl Pts',(0.00100229353986641,-0.0131787743898808,
-0.0145991747342148));
#16924=CARTESIAN_POINT('Ctrl Pts',(0.00101364138349185,-0.0131787743898808,
-0.0145930985492073));
#16925=CARTESIAN_POINT('Ctrl Pts',(0.0010249455256613,-0.0131787743898808,
-0.0145869418657868));
#16926=CARTESIAN_POINT('Ctrl Pts',(0.00130440311096153,-0.013178774389881,
-0.0144347381995232));
#16927=CARTESIAN_POINT('Ctrl Pts',(0.00155385690165563,-0.013178774389881,
-0.0142359025658652));
#16928=CARTESIAN_POINT('Ctrl Pts',(0.00175560804622792,-0.0131787743898811,
-0.0139933321990506));
#16929=CARTESIAN_POINT('Ctrl Pts',(0.00176494058753933,-0.0131787743898811,
-0.0139821114549303));
#16930=CARTESIAN_POINT('Ctrl Pts',(0.00177416959711849,-0.0131787743898811,
-0.0139707962998009));
#16931=CARTESIAN_POINT('Ctrl Pts',(0.00178329441874934,-0.013178774389881,
-0.0139593884000934));
#16932=CARTESIAN_POINT('Ctrl Pts',(0.00177804161491497,-0.0271768105190238,
-0.0139532084980533));
#16933=CARTESIAN_POINT('Ctrl Pts',(0.00118560412354709,-0.0271237595111731,
-0.0145458929746017));
#16934=CARTESIAN_POINT('Ctrl Pts',(-0.000628566750056487,-0.0270176677375825,
-0.0150813178871608));
#16935=CARTESIAN_POINT('Ctrl Pts',(-0.00278856526638462,-0.0268585351982525,
-0.0132141579990934));
#16936=CARTESIAN_POINT('Ctrl Pts',(-0.00237858331883447,-0.0266994129010339,
-0.0103922510069768));
#16937=CARTESIAN_POINT('Ctrl Pts',(0.00021399493011458,-0.0265402906038154,
-0.0092099097251141));
#16938=CARTESIAN_POINT('Ctrl Pts',(0.00261164118167257,-0.0263811683065968,
-0.010753240507375));
#16939=CARTESIAN_POINT('Ctrl Pts',(0.00260817343599891,-0.0262220460093783,
-0.0136041152219484));
#16940=CARTESIAN_POINT('Ctrl Pts',(0.000208113514731238,-0.0260629237121599,
-0.01514229898489));
#16941=CARTESIAN_POINT('Ctrl Pts',(-0.0023834422823124,-0.0259038014149411,
-0.01395419390056));
#16942=CARTESIAN_POINT('Ctrl Pts',(-0.00278437835194816,-0.0257446791177227,
-0.0111316924551894));
#16943=CARTESIAN_POINT('Ctrl Pts',(-0.000626390273332243,-0.025585556820504,
-0.00926883337176216));
#16944=CARTESIAN_POINT('Ctrl Pts',(0.00210731212168579,-0.0254264345232856,
-0.01007766841686));
#16945=CARTESIAN_POINT('Ctrl Pts',(0.00290427350329033,-0.025267312226067,
-0.0128148422875521));
#16946=CARTESIAN_POINT('Ctrl Pts',(0.00103206954891863,-0.0251081899288485,
-0.014964752376489));
#16947=CARTESIAN_POINT('Ctrl Pts',(-0.00178866211946724,-0.0249490676316299,
-0.0145515245945));
#16948=CARTESIAN_POINT('Ctrl Pts',(-0.00296552147177021,-0.0247899453344113,
-0.0119549353984463));
#16949=CARTESIAN_POINT('Ctrl Pts',(-0.00141691873677219,-0.0246308230371928,
-0.0095613809395787));
#16950=CARTESIAN_POINT('Ctrl Pts',(0.00143390397998829,-0.0244717007399742,
-0.00957065777503687));
#16951=CARTESIAN_POINT('Ctrl Pts',(0.00296689668155396,-0.0243125784427557,
-0.0119742401091903));
#16952=CARTESIAN_POINT('Ctrl Pts',(0.00177316251331238,-0.0241534561455371,
-0.0145631150614389));
#16953=CARTESIAN_POINT('Ctrl Pts',(-0.00105019709697634,-0.0239943338483186,
-0.0149579765952903));
#16954=CARTESIAN_POINT('Ctrl Pts',(-0.0029083728138988,-0.0238352115511001,
-0.0127959271259884));
#16955=CARTESIAN_POINT('Ctrl Pts',(-0.00209360791553675,-0.0236760892538814,
-0.0100639986687876));
#16956=CARTESIAN_POINT('Ctrl Pts',(0.000645287777636742,-0.023516966956663,
-0.00927297063177001));
#16957=CARTESIAN_POINT('Ctrl Pts',(0.00279113160131327,-0.0233578446594443,
-0.0111498374965911));
#16958=CARTESIAN_POINT('Ctrl Pts',(0.00237178535469283,-0.0231987223622259,
-0.0139696643841129));
#16959=CARTESIAN_POINT('Ctrl Pts',(-0.000227350711525737,-0.0230396000650072,
-0.0151408888133467));
#16960=CARTESIAN_POINT('Ctrl Pts',(-0.00261754005891038,-0.0228804777677888,
-0.0135870967313543));
#16961=CARTESIAN_POINT('Ctrl Pts',(-0.00260207867671947,-0.0227213554705702,
-0.0107363010709901));
#16962=CARTESIAN_POINT('Ctrl Pts',(-0.000195176350967375,-0.0225622331733517,
-0.00920852617061793));
#16963=CARTESIAN_POINT('Ctrl Pts',(0.00239110284023198,-0.0224031108761331,
-0.0104078738668982));
#16964=CARTESIAN_POINT('Ctrl Pts',(0.00277983847401713,-0.0222439885789146,
-0.0132320834127006));
#16965=CARTESIAN_POINT('Ctrl Pts',(0.000613762986085649,-0.022084866281696,
-0.0150855644436793));
#16966=CARTESIAN_POINT('Ctrl Pts',(-0.00211639150052274,-0.0219257439844774,
-0.0142648748368236));
#16967=CARTESIAN_POINT('Ctrl Pts',(-0.00290147594298247,-0.0217666216872589,
-0.0115242695442317));
#16968=CARTESIAN_POINT('Ctrl Pts',(-0.00101995832285557,-0.0216074993900403,
-0.00938250242413448));
#16969=CARTESIAN_POINT('Ctrl Pts',(0.00179895220381959,-0.0214483770928218,
-0.00980796498907916));
#16970=CARTESIAN_POINT('Ctrl Pts',(0.00296453533731221,-0.0212892547956032,
-0.0124096357811838));
#16971=CARTESIAN_POINT('Ctrl Pts',(0.00140556165888287,-0.0211301324983847,
-0.0147964487234853));
#16972=CARTESIAN_POINT('Ctrl Pts',(-0.00144519375143724,-0.0209710102011662,
-0.0147748028901041));
#16973=CARTESIAN_POINT('Ctrl Pts',(-0.00296774354704725,-0.0208118879039476,
-0.0123645918886645));
#16974=CARTESIAN_POINT('Ctrl Pts',(-0.00176278802491834,-0.0206527656067291,
-0.00978092063611248));
#16975=CARTESIAN_POINT('Ctrl Pts',(0.00106225819433125,-0.0204936433095104,
-0.00939831272888084));
#16976=CARTESIAN_POINT('Ctrl Pts',(0.00291103580144525,-0.020334521012292,
-0.0115684040428596));
#16977=CARTESIAN_POINT('Ctrl Pts',(0.00208442535608753,-0.0201753987150733,
-0.0142967717092857));
#16978=CARTESIAN_POINT('Ctrl Pts',(-0.00065787664180178,-0.0200162764178549,
-0.0150759088627734));
#16979=CARTESIAN_POINT('Ctrl Pts',(-0.00279555697663806,-0.0198571541206363,
-0.0131897493420468));
#16980=CARTESIAN_POINT('Ctrl Pts',(-0.0023639800967097,-0.0196980318234177,
-0.010371768442842));
#16981=CARTESIAN_POINT('Ctrl Pts',(0.000240213177657409,-0.0195389095261993,
-0.00921183209057361));
#16982=CARTESIAN_POINT('Ctrl Pts',(0.00262363848165746,-0.0193797872289806,
-0.0107759800285337));
#16983=CARTESIAN_POINT('Ctrl Pts',(0.0025958082990893,-0.0192206649317622,
-0.013626681772405));
#16984=CARTESIAN_POINT('Ctrl Pts',(0.000182299964970184,-0.0190615426345435,
-0.0151439992977471));
#16985=CARTESIAN_POINT('Ctrl Pts',(-0.00239875118947593,-0.018902420337325,
-0.013933441620598));
#16986=CARTESIAN_POINT('Ctrl Pts',(-0.00277522956952002,-0.0187432980401064,
-0.0111075720233));
#16987=CARTESIAN_POINT('Ctrl Pts',(-0.000601132642494807,-0.018584175742888,
-0.00926350654087479));
#16988=CARTESIAN_POINT('Ctrl Pts',(0.00212543536334061,-0.0184250534456693,
-0.0100960339344926));
#16989=CARTESIAN_POINT('Ctrl Pts',(0.00289862156103897,-0.0182659311484509,
-0.0128400197316981));
#16990=CARTESIAN_POINT('Ctrl Pts',(0.00100782901646378,-0.0181068088512323,
-0.0149736032207967));
#16991=CARTESIAN_POINT('Ctrl Pts',(-0.0018092089931206,-0.0179476865540137,
-0.0145359140569992));
#16992=CARTESIAN_POINT('Ctrl Pts',(-0.00296349310521268,-0.0177885642567952,
-0.0119292105563712));
#16993=CARTESIAN_POINT('Ctrl Pts',(-0.00139417826899081,-0.0176294419595766,
-0.00954918410769673));
#16994=CARTESIAN_POINT('Ctrl Pts',(0.00145645639226353,-0.0174703196623581,
-0.00958319850845797));
#16995=CARTESIAN_POINT('Ctrl Pts',(0.00296853450650743,-0.0173111973651395,
-0.0119999928166982));
#16996=CARTESIAN_POINT('Ctrl Pts',(0.0017523803714217,-0.017152075067921,
-0.0145784117258758));
#16997=CARTESIAN_POINT('Ctrl Pts',(-0.00107429930442917,-0.0169929527707024,
-0.014948758807064));
#16998=CARTESIAN_POINT('Ctrl Pts',(-0.00291364398395591,-0.0168338304734839,
-0.0127706664985865));
#16999=CARTESIAN_POINT('Ctrl Pts',(-0.00207520355930568,-0.0166747081762654,
-0.0100459109858006));
#17000=CARTESIAN_POINT('Ctrl Pts',(0.000670453121618061,-0.0165155858790467,
-0.00927867938167256));
#17001=CARTESIAN_POINT('Ctrl Pts',(0.00279992972710902,-0.0163564635818283,
-0.0111740960535678));
#17002=CARTESIAN_POINT('Ctrl Pts',(0.00235613033278755,-0.0161973412846097,
-0.013990177911836));
#17003=CARTESIAN_POINT('Ctrl Pts',(-0.000253071113445288,-0.0160382189873912,
-0.0151388043592267));
#17004=CARTESIAN_POINT('Ctrl Pts',(-0.00262968753099502,-0.0158790966901726,
-0.0135643299949519));
#17005=CARTESIAN_POINT('Ctrl Pts',(-0.00258948902257005,-0.015719974392954,
-0.0107137758623792));
#17006=CARTESIAN_POINT('Ctrl Pts',(-0.000169420211623477,-0.0155608520957355,
-0.00920694421604582));
#17007=CARTESIAN_POINT('Ctrl Pts',(0.00240635450886322,-0.0154017297985169,
-0.0104286892022747));
#17008=CARTESIAN_POINT('Ctrl Pts',(0.00277056817242066,-0.0152426075012984,
-0.0132561654242236));
#17009=CARTESIAN_POINT('Ctrl Pts',(0.000588491471565203,-0.0150834852040798,
-0.0150907810950793));
#17010=CARTESIAN_POINT('Ctrl Pts',(-0.00213444017556847,-0.0149243629068613,
-0.0142464306998757));
#17011=CARTESIAN_POINT('Ctrl Pts',(-0.00289571072485587,-0.0147652406096428,
-0.0114991177966801));
#17012=CARTESIAN_POINT('Ctrl Pts',(-0.000995684446481558,-0.0146061183124242,
-0.0093737546786092));
#17013=CARTESIAN_POINT('Ctrl Pts',(0.00181943901096383,-0.0144469960152056,
-0.00982366893049069));
#17014=CARTESIAN_POINT('Ctrl Pts',(0.00296238076824064,-0.0142878737179871,
-0.012435342848044));
#17015=CARTESIAN_POINT('Ctrl Pts',(0.00138279676337737,-0.0141287514207685,
-0.0148085639739896));
#17016=CARTESIAN_POINT('Ctrl Pts',(-0.00146774688362298,-0.01396962912355,
-0.0147621306115525));
#17017=CARTESIAN_POINT('Ctrl Pts',(-0.00296916099271162,-0.0138105068263315,
-0.0123388987639402));
#17018=CARTESIAN_POINT('Ctrl Pts',(-0.00174215309885327,-0.0136513845291129,
-0.00976558372456728));
#17019=CARTESIAN_POINT('Ctrl Pts',(0.00108673957578367,-0.0134922622318943,
-0.00940789155737695));
#17020=CARTESIAN_POINT('Ctrl Pts',(0.00291537148706041,-0.0133331399346758,
-0.0115931828919089));
#17021=CARTESIAN_POINT('Ctrl Pts',(0.00206758582828193,-0.0131740176374573,
-0.0143157742579136));
#17022=CARTESIAN_POINT('Ctrl Pts',(-0.000686797985030798,-0.0130148766356141,
-0.0150681813871851));
#17023=CARTESIAN_POINT('Ctrl Pts',(-0.00209243490244101,-0.0129087763995103,
-0.0138021198294159));
#17024=CARTESIAN_POINT('Ctrl Pts',(-0.00237105117954937,-0.0128557169291459,
-0.0130116402165948));
#17025=CARTESIAN_POINT('Ctrl Pts',(0.0019117872489877,-0.0272859922955674,
-0.0140869025003421));
#17026=CARTESIAN_POINT('Ctrl Pts',(0.00127478616176987,-0.0272329412877163,
-0.0147241691511522));
#17027=CARTESIAN_POINT('Ctrl Pts',(-0.000675848016050572,-0.0271268495141259,
-0.0152998691302945));
#17028=CARTESIAN_POINT('Ctrl Pts',(-0.00299832325324907,-0.0269677169747958,
-0.0132922600642947));
#17029=CARTESIAN_POINT('Ctrl Pts',(-0.00255750215375024,-0.0268085946775773,
-0.0102580870955053));
#17030=CARTESIAN_POINT('Ctrl Pts',(0.000230091790489749,-0.0266494723803588,
-0.00898680920883726));
#17031=CARTESIAN_POINT('Ctrl Pts',(0.00280809080517024,-0.0264903500831402,
-0.01064623049895));
#17032=CARTESIAN_POINT('Ctrl Pts',(0.00280436221304618,-0.0263312277859216,
-0.0137115501641726));
#17033=CARTESIAN_POINT('Ctrl Pts',(0.000223767970596245,-0.0261721054887031,
-0.0153654372722831));
#17034=CARTESIAN_POINT('Ctrl Pts',(-0.00256272661213327,-0.0260129831914847,
-0.01408796202557));
#17035=CARTESIAN_POINT('Ctrl Pts',(-0.00299382139594434,-0.0258538608942659,
-0.0110531498883035));
#17036=CARTESIAN_POINT('Ctrl Pts',(-0.0006735078231022,-0.0256947385970475,
-0.00905016513671916));
#17037=CARTESIAN_POINT('Ctrl Pts',(0.00226582573213212,-0.025535616299829,
-0.00991984136520626));
#17038=CARTESIAN_POINT('Ctrl Pts',(0.0031227351511842,-0.0253764940026104,
-0.0128629075231386));
#17039=CARTESIAN_POINT('Ctrl Pts',(0.00110970260040032,-0.0252173717053917,
-0.0151745354738127));
#17040=CARTESIAN_POINT('Ctrl Pts',(-0.0019232066359191,-0.0250582494081734,
-0.0147302243857556));
#17041=CARTESIAN_POINT('Ctrl Pts',(-0.0031885902381428,-0.0248991271109547,
-0.0119383177879384));
#17042=CARTESIAN_POINT('Ctrl Pts',(-0.0015235004350235,-0.0247400048137363,
-0.00936471835368694));
#17043=CARTESIAN_POINT('Ctrl Pts',(0.00154176332107131,-0.0245808825165175,
-0.00937469299971953));
#17044=CARTESIAN_POINT('Ctrl Pts',(0.00319006889224584,-0.0244217602192992,
-0.0119590746136147));
#17045=CARTESIAN_POINT('Ctrl Pts',(0.00190654113767505,-0.0242626379220806,
-0.0147426866963774));
#17046=CARTESIAN_POINT('Ctrl Pts',(-0.00112919371632327,-0.0241035156248619,
-0.0151672500132313));
#17047=CARTESIAN_POINT('Ctrl Pts',(-0.0031271428150348,-0.0239443933276435,
-0.0128425695488265));
#17048=CARTESIAN_POINT('Ctrl Pts',(-0.00225109068523927,-0.0237852710304249,
-0.00990514336835257));
#17049=CARTESIAN_POINT('Ctrl Pts',(0.000693826811962741,-0.0236261487332063,
-0.00905461360455169));
#17050=CARTESIAN_POINT('Ctrl Pts',(0.00300108262983063,-0.0234670264359878,
-0.0110726598134331));
#17051=CARTESIAN_POINT('Ctrl Pts',(0.00255019284160814,-0.0233079041387693,
-0.014104596210588));
#17052=CARTESIAN_POINT('Ctrl Pts',(-0.000244452203872613,-0.0231487818415506,
-0.0153639210265705));
#17053=CARTESIAN_POINT('Ctrl Pts',(-0.00281443340041212,-0.0229896595443322,
-0.013693251529854));
#17054=CARTESIAN_POINT('Ctrl Pts',(-0.00279780900136746,-0.0228305372471135,
-0.0106280168653581));
#17055=CARTESIAN_POINT('Ctrl Pts',(-0.000209857663596484,-0.022671414949895,
-0.00898532158232617));
#17056=CARTESIAN_POINT('Ctrl Pts',(0.00257096340300922,-0.0225122926526765,
-0.0102748851187573));
#17057=CARTESIAN_POINT('Ctrl Pts',(0.00298894002496421,-0.0223531703554579,
-0.0133115338410611));
#17058=CARTESIAN_POINT('Ctrl Pts',(0.000659930701765533,-0.0221940480582394,
-0.0153044351160038));
#17059=CARTESIAN_POINT('Ctrl Pts',(-0.00227558806870716,-0.0220349257610208,
-0.0144220126166641));
#17060=CARTESIAN_POINT('Ctrl Pts',(-0.00311972715627565,-0.0218758034638022,
-0.0114752569226835));
#17061=CARTESIAN_POINT('Ctrl Pts',(-0.00109668035875944,-0.0217166811665838,
-0.00917238446111915));
#17062=CARTESIAN_POINT('Ctrl Pts',(0.00193427074819341,-0.0215575588693652,
-0.00962985064175281));
#17063=CARTESIAN_POINT('Ctrl Pts',(0.00318752992590557,-0.0213984365721466,
-0.0124272210771164));
#17064=CARTESIAN_POINT('Ctrl Pts',(0.00151128906915194,-0.021239314274928,
-0.0149935718928306));
#17065=CARTESIAN_POINT('Ctrl Pts',(-0.00155390231766119,-0.0210801919777095,
-0.0149702978435032));
#17066=CARTESIAN_POINT('Ctrl Pts',(-0.00319097945960156,-0.020921069680491,
-0.0123787889489587));
#17067=CARTESIAN_POINT('Ctrl Pts',(-0.00189538627242324,-0.0207619473832725,
-0.00960077199211658));
#17068=CARTESIAN_POINT('Ctrl Pts',(0.00114216205853669,-0.0206028250860538,
-0.00918938402893757));
#17069=CARTESIAN_POINT('Ctrl Pts',(0.00313000611451711,-0.0204437027888353,
-0.0115227112516539));
#17070=CARTESIAN_POINT('Ctrl Pts',(0.00224121740672834,-0.0202845804916167,
-0.0144563087959796));
#17071=CARTESIAN_POINT('Ctrl Pts',(-0.000707362620004616,-0.0201254581943983,
-0.0152940532350047));
#17072=CARTESIAN_POINT('Ctrl Pts',(-0.00300584088523195,-0.0199663358971797,
-0.0132660153696177));
#17073=CARTESIAN_POINT('Ctrl Pts',(-0.0025418004662205,-0.0198072135999612,
-0.010236063817416));
#17074=CARTESIAN_POINT('Ctrl Pts',(0.000258282194427836,-0.0196480913027426,
-0.00898887617607948));
#17075=CARTESIAN_POINT('Ctrl Pts',(0.00282099055112725,-0.0194889690055241,
-0.0106706805040763));
#17076=CARTESIAN_POINT('Ctrl Pts',(0.00279106696119298,-0.0193298467083055,
-0.0137358141876099));
#17077=CARTESIAN_POINT('Ctrl Pts',(0.000196012706112937,-0.019170724411087,
-0.0153672654839583));
#17078=CARTESIAN_POINT('Ctrl Pts',(-0.00257918706686371,-0.0190116021138684,
-0.0140656487434252));
#17079=CARTESIAN_POINT('Ctrl Pts',(-0.00298398443518755,-0.0188524798166499,
-0.0110272150992978));
#17080=CARTESIAN_POINT('Ctrl Pts',(-0.000646350294184092,-0.0186933575194313,
-0.00904443761758662));
#17081=CARTESIAN_POINT('Ctrl Pts',(0.00228531221772131,-0.0185342352222128,
-0.00993958835095536));
#17082=CARTESIAN_POINT('Ctrl Pts',(0.0031166580655651,-0.0183751129249941,
-0.0128899788336617));
#17083=CARTESIAN_POINT('Ctrl Pts',(0.00108363867677383,-0.0182159906277757,
-0.0151840520853187));
#17084=CARTESIAN_POINT('Ctrl Pts',(-0.00194529906093746,-0.0180568683305571,
-0.014713439611826));
#17085=CARTESIAN_POINT('Ctrl Pts',(-0.00318640929631981,-0.0178977460333385,
-0.0119106579038002));
#17086=CARTESIAN_POINT('Ctrl Pts',(-0.00149904941206893,-0.0177386237361201,
-0.00935160406689274));
#17087=CARTESIAN_POINT('Ctrl Pts',(0.00156601214284244,-0.0175795014389015,
-0.00938817705658642));
#17088=CARTESIAN_POINT('Ctrl Pts',(0.00319182991563014,-0.0174203791416829,
-0.0119867644592445));
#17089=CARTESIAN_POINT('Ctrl Pts',(0.00188419574736476,-0.0172612568444644,
-0.0147591339874741));
#17090=CARTESIAN_POINT('Ctrl Pts',(-0.00115510891003655,-0.0171021345472458,
-0.0151573388560083));
#17091=CARTESIAN_POINT('Ctrl Pts',(-0.00313281048648741,-0.0169430122500273,
-0.0128154087979401));
#17092=CARTESIAN_POINT('Ctrl Pts',(-0.00223130193942295,-0.0167838899528087,
-0.00988569511618116));
#17093=CARTESIAN_POINT('Ctrl Pts',(0.000720885112137661,-0.0166247676555902,
-0.00906075177093641));
#17094=CARTESIAN_POINT('Ctrl Pts',(0.00301054255729814,-0.0164656453583716,
-0.0110987431173996));
#17095=CARTESIAN_POINT('Ctrl Pts',(0.00253336023712347,-0.0163065230611531,
-0.0141266527813699));
#17096=CARTESIAN_POINT('Ctrl Pts',(-0.000272107313863377,-0.0161474007639344,
-0.0153616797782363));
#17097=CARTESIAN_POINT('Ctrl Pts',(-0.00282749461452771,-0.015988278466716,
-0.0136687722623329));
#17098=CARTESIAN_POINT('Ctrl Pts',(-0.002784272343918,-0.0158291561694974,
-0.0106037972935313));
#17099=CARTESIAN_POINT('Ctrl Pts',(-0.000182164127985299,-0.0156700338722789,
-0.00898362063193561));
#17100=CARTESIAN_POINT('Ctrl Pts',(0.00258736231368171,-0.0155109115750603,
-0.0102972661993925));
#17101=CARTESIAN_POINT('Ctrl Pts',(0.00297897240427542,-0.0153517892778418,
-0.0133374273196913));
#17102=CARTESIAN_POINT('Ctrl Pts',(0.000632758244823287,-0.0151926669806233,
-0.0153100441678648));
#17103=CARTESIAN_POINT('Ctrl Pts',(-0.00229499437873055,-0.0150335446834047,
-0.0144021810977954));
#17104=CARTESIAN_POINT('Ctrl Pts',(-0.00311352827408435,-0.0148744223861861,
-0.011448213241672));
#17105=CARTESIAN_POINT('Ctrl Pts',(-0.00107058058305899,-0.0147153000889676,
-0.00916297870356417));
#17106=CARTESIAN_POINT('Ctrl Pts',(0.00195629858845448,-0.014556177791749,
-0.00964673584550599));
#17107=CARTESIAN_POINT('Ctrl Pts',(0.00318521328852005,-0.0143970554945306,
-0.0124548618489747));
#17108=CARTESIAN_POINT('Ctrl Pts',(0.00148681178100139,-0.0142379331973119,
-0.0150065984616343));
#17109=CARTESIAN_POINT('Ctrl Pts',(-0.00157815191349504,-0.0140788109000934,
-0.0149566723465815));
#17110=CARTESIAN_POINT('Ctrl Pts',(-0.00319250352660007,-0.0139196886028748,
-0.0123511631679746));
#17111=CARTESIAN_POINT('Ctrl Pts',(-0.0018731991716242,-0.0137605663056563,
-0.00958428142649361));
#17112=CARTESIAN_POINT('Ctrl Pts',(0.00116848494800438,-0.0136014440084377,
-0.00919968338415261));
#17113=CARTESIAN_POINT('Ctrl Pts',(0.00313466793368104,-0.0134423217112193,
-0.011549353984456));
#17114=CARTESIAN_POINT('Ctrl Pts',(0.0022231111969143,-0.0132831994140006,
-0.0144767407306771));
#17115=CARTESIAN_POINT('Ctrl Pts',(-0.000738459448529337,-0.0131240584121574,
-0.0152857444928626));
#17116=CARTESIAN_POINT('Ctrl Pts',(-0.00224982943721194,-0.0130179581760535,
-0.0139244488278607));
#17117=CARTESIAN_POINT('Ctrl Pts',(-0.00254940344125551,-0.0129648987056893,
-0.0130745087411389));
#17118=CARTESIAN_POINT('Ctrl Pts',(0.00204553288306044,-0.0273951740721106,
-0.0142205965026308));
#17119=CARTESIAN_POINT('Ctrl Pts',(0.00136396819999266,-0.0273421230642597,
-0.0149024453277029));
#17120=CARTESIAN_POINT('Ctrl Pts',(-0.000723129282044651,-0.0272360312906692,
-0.0155184203734285));
#17121=CARTESIAN_POINT('Ctrl Pts',(-0.00320808124011354,-0.0270768987513391,
-0.013370362129496));
#17122=CARTESIAN_POINT('Ctrl Pts',(-0.00273642098866601,-0.0269177764541206,
-0.0101239231840337));
#17123=CARTESIAN_POINT('Ctrl Pts',(0.000246188650864915,-0.026758654156902,
-0.00876370869256043));
#17124=CARTESIAN_POINT('Ctrl Pts',(0.00300454042866792,-0.0265995318596834,
-0.0105392204905252));
#17125=CARTESIAN_POINT('Ctrl Pts',(0.00300055099009345,-0.026440409562465,
-0.0138189851063969));
#17126=CARTESIAN_POINT('Ctrl Pts',(0.000239422426461252,-0.0262812872652464,
-0.0155885755596761));
#17127=CARTESIAN_POINT('Ctrl Pts',(-0.00274201094195411,-0.0261221649680278,
-0.01422173015058));
#17128=CARTESIAN_POINT('Ctrl Pts',(-0.00320326443994053,-0.0259630426708093,
-0.0109746073214176));
#17129=CARTESIAN_POINT('Ctrl Pts',(-0.000720625372872156,-0.0258039203735906,
-0.00883149690167625));
#17130=CARTESIAN_POINT('Ctrl Pts',(0.00242433934257846,-0.0256447980763722,
-0.0097620143135525));
#17131=CARTESIAN_POINT('Ctrl Pts',(0.00334119679907805,-0.0254856757791536,
-0.012910972758725));
#17132=CARTESIAN_POINT('Ctrl Pts',(0.001187335651882,-0.0253265534819351,
-0.0153843185711368));
#17133=CARTESIAN_POINT('Ctrl Pts',(-0.00205775115237095,-0.0251674311847165,
-0.0149089241770113));
#17134=CARTESIAN_POINT('Ctrl Pts',(-0.00341165900451537,-0.025008308887498,
-0.0119217001774306));
#17135=CARTESIAN_POINT('Ctrl Pts',(-0.00163008213327481,-0.0248491865902795,
-0.00916805576779518));
#17136=CARTESIAN_POINT('Ctrl Pts',(0.00164962266215434,-0.0246900642930608,
-0.0091787282244021));
#17137=CARTESIAN_POINT('Ctrl Pts',(0.00341324110293771,-0.0245309419958423,
-0.011943909118039));
#17138=CARTESIAN_POINT('Ctrl Pts',(0.00203991976203773,-0.0243718196986238,
-0.014922258331316));
#17139=CARTESIAN_POINT('Ctrl Pts',(-0.00120819033567019,-0.0242126974014052,
-0.0153765234311726));
#17140=CARTESIAN_POINT('Ctrl Pts',(-0.00334591281617079,-0.0240535751041867,
-0.0128892119716646));
#17141=CARTESIAN_POINT('Ctrl Pts',(-0.00240857345494178,-0.0238944528069681,
-0.00974628806791765));
#17142=CARTESIAN_POINT('Ctrl Pts',(0.000742365846288737,-0.0237353305097496,
-0.00883625657733327));
#17143=CARTESIAN_POINT('Ctrl Pts',(0.003211033658348,-0.023576208212531,
-0.0109954821302748));
#17144=CARTESIAN_POINT('Ctrl Pts',(0.00272860032852343,-0.0234170859153125,
-0.0142395280370631));
#17145=CARTESIAN_POINT('Ctrl Pts',(-0.000261553696219489,-0.0232579636180939,
-0.0155869532397943));
#17146=CARTESIAN_POINT('Ctrl Pts',(-0.00301132674191384,-0.0230988413208754,
-0.0137994063283536));
#17147=CARTESIAN_POINT('Ctrl Pts',(-0.00299353932601547,-0.0229397190236568,
-0.0105197326597259));
#17148=CARTESIAN_POINT('Ctrl Pts',(-0.000224538976225593,-0.0227805967264383,
-0.00876211699403452));
#17149=CARTESIAN_POINT('Ctrl Pts',(0.00275082396578644,-0.0226214744292197,
-0.0101418963706166));
#17150=CARTESIAN_POINT('Ctrl Pts',(0.0031980415759113,-0.0224623521320012,
-0.0133909842694217));
#17151=CARTESIAN_POINT('Ctrl Pts',(0.000706098417445418,-0.0223032298347826,
-0.0155233057883285));
#17152=CARTESIAN_POINT('Ctrl Pts',(-0.00243478463689158,-0.0221441075375641,
-0.0145791503965046));
#17153=CARTESIAN_POINT('Ctrl Pts',(-0.00333797836956883,-0.0219849852403455,
-0.011426244301135));
#17154=CARTESIAN_POINT('Ctrl Pts',(-0.0011734023946633,-0.021825862943127,
-0.00896226649810381));
#17155=CARTESIAN_POINT('Ctrl Pts',(0.00206958929256724,-0.0216667406459084,
-0.00945173629442646));
#17156=CARTESIAN_POINT('Ctrl Pts',(0.00341052451449892,-0.0215076183486899,
-0.0124448063730491));
#17157=CARTESIAN_POINT('Ctrl Pts',(0.00161701647942103,-0.0213484960514714,
-0.015190695062176));
#17158=CARTESIAN_POINT('Ctrl Pts',(-0.00166261088388514,-0.0211893737542528,
-0.0151657927969023));
#17159=CARTESIAN_POINT('Ctrl Pts',(-0.00341421537215588,-0.0210302514570342,
-0.0123929860092532));
#17160=CARTESIAN_POINT('Ctrl Pts',(-0.00202798451992814,-0.0208711291598156,
-0.00942062334812066));
#17161=CARTESIAN_POINT('Ctrl Pts',(0.00122206592274213,-0.0207120068625972,
-0.0089804553289943));
#17162=CARTESIAN_POINT('Ctrl Pts',(0.00334897642758895,-0.0205528845653786,
-0.0114770184604482));
#17163=CARTESIAN_POINT('Ctrl Pts',(0.00239800945736913,-0.02039376226816,
-0.0146158458826736));
#17164=CARTESIAN_POINT('Ctrl Pts',(-0.000756848598207453,-0.0202346399709415,
-0.0155121976072364));
#17165=CARTESIAN_POINT('Ctrl Pts',(-0.00321612479382583,-0.0200755176737229,
-0.0133422813971887));
#17166=CARTESIAN_POINT('Ctrl Pts',(-0.00271962083573129,-0.0199163953765044,
-0.01010035919199));
#17167=CARTESIAN_POINT('Ctrl Pts',(0.000276351211198263,-0.0197572730792858,
-0.00876592026158535));
#17168=CARTESIAN_POINT('Ctrl Pts',(0.00301834262059706,-0.0195981507820673,
-0.0105653809796189));
#17169=CARTESIAN_POINT('Ctrl Pts',(0.00298632562329664,-0.0194390284848487,
-0.0138449466028145));
#17170=CARTESIAN_POINT('Ctrl Pts',(0.000209725447255692,-0.0192799061876302,
-0.0155905316701697));
#17171=CARTESIAN_POINT('Ctrl Pts',(-0.00275962294425149,-0.0191207838904117,
-0.0141978558662525));
#17172=CARTESIAN_POINT('Ctrl Pts',(-0.00319273930085507,-0.018961661593193,
-0.0109468581752957));
#17173=CARTESIAN_POINT('Ctrl Pts',(-0.000691567945873381,-0.0188025392959746,
-0.00882536869429835));
#17174=CARTESIAN_POINT('Ctrl Pts',(0.00244518907210201,-0.018643416998756,
-0.00978314276741825));
#17175=CARTESIAN_POINT('Ctrl Pts',(0.00333469457009122,-0.0184842947015375,
-0.0129399379356254));
#17176=CARTESIAN_POINT('Ctrl Pts',(0.00115944833708388,-0.0183251724043189,
-0.0153945009498407));
#17177=CARTESIAN_POINT('Ctrl Pts',(-0.00208138912875434,-0.0181660501071004,
-0.0148909651666526));
#17178=CARTESIAN_POINT('Ctrl Pts',(-0.00340932548742695,-0.0180069278098818,
-0.0118921052512293));
#17179=CARTESIAN_POINT('Ctrl Pts',(-0.00160392055514706,-0.0178478055126632,
-0.00915402402608875));
#17180=CARTESIAN_POINT('Ctrl Pts',(0.00167556789342136,-0.0176886832154447,
-0.00919315560471498));
#17181=CARTESIAN_POINT('Ctrl Pts',(0.00341512532475283,-0.0175295609182261,
-0.0119735361017907));
#17182=CARTESIAN_POINT('Ctrl Pts',(0.00201601112330781,-0.0173704386210076,
-0.0149398562490724));
#17183=CARTESIAN_POINT('Ctrl Pts',(-0.00123591851564392,-0.0172113163237891,
-0.0153659189049525));
#17184=CARTESIAN_POINT('Ctrl Pts',(-0.0033519769890189,-0.0170521940265705,
-0.0128601510972937));
#17185=CARTESIAN_POINT('Ctrl Pts',(-0.00238740031954021,-0.016893071729352,
-0.00972547924656174));
#17186=CARTESIAN_POINT('Ctrl Pts',(0.000771317102657261,-0.0167339494321333,
-0.00884282416020026));
#17187=CARTESIAN_POINT('Ctrl Pts',(0.00322115538748726,-0.0165748271349149,
-0.0110233901812313));
#17188=CARTESIAN_POINT('Ctrl Pts',(0.00271059014145939,-0.0164157048376963,
-0.0142631276509039));
#17189=CARTESIAN_POINT('Ctrl Pts',(-0.000291143514281472,-0.0162565825404778,
-0.0155845551972457));
#17190=CARTESIAN_POINT('Ctrl Pts',(-0.00302530169806039,-0.0160974602432592,
-0.0137732145297137));
#17191=CARTESIAN_POINT('Ctrl Pts',(-0.00297905566526595,-0.0159383379460406,
-0.0104938187246836));
#17192=CARTESIAN_POINT('Ctrl Pts',(-0.000194908044347123,-0.0157792156488221,
-0.0087602970478254));
#17193=CARTESIAN_POINT('Ctrl Pts',(0.0027683701185002,-0.0156200933516036,
-0.0101658431965103));
#17194=CARTESIAN_POINT('Ctrl Pts',(0.00318737663613016,-0.015460971054385,
-0.0134186892151591));
#17195=CARTESIAN_POINT('Ctrl Pts',(0.000677025018081376,-0.0153018487571665,
-0.0155293072406504));
#17196=CARTESIAN_POINT('Ctrl Pts',(-0.00245554858189265,-0.0151427264599479,
-0.0145579314957151));
#17197=CARTESIAN_POINT('Ctrl Pts',(-0.00333134582331285,-0.0149836041627294,
-0.0113973086866639));
#17198=CARTESIAN_POINT('Ctrl Pts',(-0.00114547671963643,-0.0148244818655108,
-0.00895220272851903));
#17199=CARTESIAN_POINT('Ctrl Pts',(0.00209315816594511,-0.0146653595682923,
-0.00946980276052119));
#17200=CARTESIAN_POINT('Ctrl Pts',(0.00340804580879949,-0.0145062372710737,
-0.0124743808499052));
#17201=CARTESIAN_POINT('Ctrl Pts',(0.00159082679862542,-0.0143471149738551,
-0.015204632949279));
#17202=CARTESIAN_POINT('Ctrl Pts',(-0.00168855694336709,-0.0141879926766366,
-0.0151512140816105));
#17203=CARTESIAN_POINT('Ctrl Pts',(-0.00341584606048853,-0.0140288703794181,
-0.0123634275720089));
#17204=CARTESIAN_POINT('Ctrl Pts',(-0.00200424524439513,-0.0138697480821995,
-0.00940297912842001));
#17205=CARTESIAN_POINT('Ctrl Pts',(0.00125023032022508,-0.0137106257849809,
-0.00899147521092818));
#17206=CARTESIAN_POINT('Ctrl Pts',(0.00335396438030165,-0.0135515034877625,
-0.0115055250770028));
#17207=CARTESIAN_POINT('Ctrl Pts',(0.00237863656554669,-0.0133923811905438,
-0.0146377072034405));
#17208=CARTESIAN_POINT('Ctrl Pts',(-0.000790120912027881,-0.0132332401887006,
-0.0155033075985401));
#17209=CARTESIAN_POINT('Ctrl Pts',(-0.00240722397198286,-0.0131271399525968,
-0.0140467778263056));
#17210=CARTESIAN_POINT('Ctrl Pts',(-0.00272775570296166,-0.0130740804822326,
-0.0131373772656828));
#17211=CARTESIAN_POINT('Ctrl Pts',(0.00217927851713317,-0.0275043558486539,
-0.0143542905049196));
#17212=CARTESIAN_POINT('Ctrl Pts',(0.00145315023821544,-0.0274513048408029,
-0.0150807215042535));
#17213=CARTESIAN_POINT('Ctrl Pts',(-0.000770410548038733,-0.0273452130672124,
-0.0157369716165624));
#17214=CARTESIAN_POINT('Ctrl Pts',(-0.00341783922697799,-0.0271860805278823,
-0.0134484641946973));
#17215=CARTESIAN_POINT('Ctrl Pts',(-0.00291533982358178,-0.0270269582306638,
-0.00998975927256213));
#17216=CARTESIAN_POINT('Ctrl Pts',(0.000262285511240084,-0.0268678359334452,
-0.00854060817628358));
#17217=CARTESIAN_POINT('Ctrl Pts',(0.00320099005216559,-0.0267087136362267,
-0.0104322104821004));
#17218=CARTESIAN_POINT('Ctrl Pts',(0.00319673976714072,-0.0265495913390081,
-0.0139264200486212));
#17219=CARTESIAN_POINT('Ctrl Pts',(0.000255076882326259,-0.0263904690417896,
-0.0158117138470693));
#17220=CARTESIAN_POINT('Ctrl Pts',(-0.00292129527177496,-0.026231346744571,
-0.0143554982755902));
#17221=CARTESIAN_POINT('Ctrl Pts',(-0.00341270748393672,-0.0260722244473525,
-0.0108960647545318));
#17222=CARTESIAN_POINT('Ctrl Pts',(-0.000767742922642114,-0.0259131021501339,
-0.00861282866663324));
#17223=CARTESIAN_POINT('Ctrl Pts',(0.00258285295302481,-0.0257539798529154,
-0.00960418726189884));
#17224=CARTESIAN_POINT('Ctrl Pts',(0.00355965844697192,-0.0255948575556968,
-0.0129590379943115));
#17225=CARTESIAN_POINT('Ctrl Pts',(0.00126496870336369,-0.0254357352584783,
-0.0155941016684606));
#17226=CARTESIAN_POINT('Ctrl Pts',(-0.00219229566882281,-0.0252766129612597,
-0.0150876239682666));
#17227=CARTESIAN_POINT('Ctrl Pts',(-0.00363472777088795,-0.0251174906640412,
-0.0119050825669227));
#17228=CARTESIAN_POINT('Ctrl Pts',(-0.00173666383152611,-0.0249583683668226,
-0.00897139318190331));
#17229=CARTESIAN_POINT('Ctrl Pts',(0.00175748200323739,-0.0247992460696041,
-0.00898276344908466));
#17230=CARTESIAN_POINT('Ctrl Pts',(0.00363641331362957,-0.0246401237723855,
-0.0119287436224631));
#17231=CARTESIAN_POINT('Ctrl Pts',(0.00217329838640041,-0.024481001475167,
-0.0151018299662544));
#17232=CARTESIAN_POINT('Ctrl Pts',(-0.00128718695501713,-0.0243218791779484,
-0.0155857968491138));
#17233=CARTESIAN_POINT('Ctrl Pts',(-0.00356468281730678,-0.0241627568807299,
-0.0129358543945025));
#17234=CARTESIAN_POINT('Ctrl Pts',(-0.00256605622464431,-0.0240036345835113,
-0.00958743276748271));
#17235=CARTESIAN_POINT('Ctrl Pts',(0.000790904880614737,-0.0238445122862928,
-0.00861789955011497));
#17236=CARTESIAN_POINT('Ctrl Pts',(0.00342098468686536,-0.0236853899890742,
-0.0109183044471168));
#17237=CARTESIAN_POINT('Ctrl Pts',(0.00290700781543874,-0.0235262676918557,
-0.0143744598635381));
#17238=CARTESIAN_POINT('Ctrl Pts',(-0.000278655188566368,-0.0233671453946371,
-0.0158099854530181));
#17239=CARTESIAN_POINT('Ctrl Pts',(-0.00320822008341556,-0.0232080230974186,
-0.0139055611268533));
#17240=CARTESIAN_POINT('Ctrl Pts',(-0.00318926965066348,-0.0230489008002001,
-0.0104114484540937));
#17241=CARTESIAN_POINT('Ctrl Pts',(-0.000239220288854699,-0.0228897785029815,
-0.00853891240574276));
#17242=CARTESIAN_POINT('Ctrl Pts',(0.00293068452856366,-0.022730656205763,
-0.0100089076224755));
#17243=CARTESIAN_POINT('Ctrl Pts',(0.00340714312685838,-0.0225715339085444,
-0.0134704346977821));
#17244=CARTESIAN_POINT('Ctrl Pts',(0.000752266133125304,-0.0224124116113258,
-0.0157421764606531));
#17245=CARTESIAN_POINT('Ctrl Pts',(-0.002593981205076,-0.0222532893141073,
-0.0147362881763453));
#17246=CARTESIAN_POINT('Ctrl Pts',(-0.00355622958286202,-0.0220941670168887,
-0.0113772316795867));
#17247=CARTESIAN_POINT('Ctrl Pts',(-0.00125012443056717,-0.0219350447196702,
-0.00875214853508845));
#17248=CARTESIAN_POINT('Ctrl Pts',(0.00220490783694106,-0.0217759224224516,
-0.00927362194710001));
#17249=CARTESIAN_POINT('Ctrl Pts',(0.00363351910309228,-0.0216168001252331,
-0.0124623916689818));
#17250=CARTESIAN_POINT('Ctrl Pts',(0.00172274388969011,-0.0214576778280145,
-0.0153878182315213));
#17251=CARTESIAN_POINT('Ctrl Pts',(-0.00177131945010908,-0.021298555530796,
-0.0153612877503014));
#17252=CARTESIAN_POINT('Ctrl Pts',(-0.00363745128471018,-0.0211394332335774,
-0.0124071830695474));
#17253=CARTESIAN_POINT('Ctrl Pts',(-0.00216058276743305,-0.0209803109363589,
-0.00924047470412463));
#17254=CARTESIAN_POINT('Ctrl Pts',(0.00130196978694757,-0.0208211886391403,
-0.00877152662905103));
#17255=CARTESIAN_POINT('Ctrl Pts',(0.00356794674066081,-0.0206620663419218,
-0.0114313256692425));
#17256=CARTESIAN_POINT('Ctrl Pts',(0.00255480150800994,-0.0205029440447033,
-0.0147753829693676));
#17257=CARTESIAN_POINT('Ctrl Pts',(-0.000806334576410288,-0.0203438217474846,
-0.0157303419794677));
#17258=CARTESIAN_POINT('Ctrl Pts',(-0.00342640870241972,-0.0201846994502662,
-0.0134185474247594));
#17259=CARTESIAN_POINT('Ctrl Pts',(-0.00289744120524209,-0.0200255771530476,
-0.00996465456656415));
#17260=CARTESIAN_POINT('Ctrl Pts',(0.00029442022796869,-0.0198664548558291,
-0.00854296434709121));
#17261=CARTESIAN_POINT('Ctrl Pts',(0.00321569469006684,-0.0197073325586105,
-0.0104600814551616));
#17262=CARTESIAN_POINT('Ctrl Pts',(0.00318158428540032,-0.019548210261392,
-0.0139540790180195));
#17263=CARTESIAN_POINT('Ctrl Pts',(0.000223438188398445,-0.0193890879641734,
-0.0158137978563808));
#17264=CARTESIAN_POINT('Ctrl Pts',(-0.00294005882163927,-0.0192299656669548,
-0.0143300629890799));
#17265=CARTESIAN_POINT('Ctrl Pts',(-0.0034014941665226,-0.0190708433697363,
-0.0108665012512935));
#17266=CARTESIAN_POINT('Ctrl Pts',(-0.000736785597562666,-0.0189117210725177,
-0.00860629977101019));
#17267=CARTESIAN_POINT('Ctrl Pts',(0.00260506592648272,-0.0187525987752992,
-0.00962669718388102));
#17268=CARTESIAN_POINT('Ctrl Pts',(0.00355273107461734,-0.0185934764780806,
-0.012989897037589));
#17269=CARTESIAN_POINT('Ctrl Pts',(0.00123525799739393,-0.0184343541808621,
-0.0156049498143626));
#17270=CARTESIAN_POINT('Ctrl Pts',(-0.0022174791965712,-0.0182752318836436,
-0.0150684907214794));
#17271=CARTESIAN_POINT('Ctrl Pts',(-0.0036322416785341,-0.018116109586425,
-0.0118735525986582));
#17272=CARTESIAN_POINT('Ctrl Pts',(-0.00170879169822517,-0.0179569872892065,
-0.00895644398528475));
#17273=CARTESIAN_POINT('Ctrl Pts',(0.00178512364400027,-0.0177978649919879,
-0.00899813415284341));
#17274=CARTESIAN_POINT('Ctrl Pts',(0.00363842073387552,-0.0176387426947694,
-0.011960307744337));
#17275=CARTESIAN_POINT('Ctrl Pts',(0.00214782649925085,-0.0174796203975508,
-0.0151205785106708));
#17276=CARTESIAN_POINT('Ctrl Pts',(-0.00131672812125129,-0.0173204981003323,
-0.0155744989538967));
#17277=CARTESIAN_POINT('Ctrl Pts',(-0.00357114349155041,-0.0171613758031137,
-0.0129048933966471));
#17278=CARTESIAN_POINT('Ctrl Pts',(-0.0025434986996575,-0.0170022535058952,
-0.00956526337694232));
#17279=CARTESIAN_POINT('Ctrl Pts',(0.000821749093176863,-0.0168431312086766,
-0.0086248965494641));
#17280=CARTESIAN_POINT('Ctrl Pts',(0.00343176821767638,-0.016684008911458,
-0.0109480372450631));
#17281=CARTESIAN_POINT('Ctrl Pts',(0.00288782004579531,-0.0165248866142396,
-0.014399602520438));
#17282=CARTESIAN_POINT('Ctrl Pts',(-0.000310179714699567,-0.0163657643170209,
-0.0158074306162551));
#17283=CARTESIAN_POINT('Ctrl Pts',(-0.00322310878159308,-0.0162066420198024,
-0.0138776567970947));
#17284=CARTESIAN_POINT('Ctrl Pts',(-0.00317383898661389,-0.0160475197225839,
-0.0103838401558357));
#17285=CARTESIAN_POINT('Ctrl Pts',(-0.000207651960708945,-0.0158883974253653,
-0.00853697346371519));
#17286=CARTESIAN_POINT('Ctrl Pts',(0.00294937792331869,-0.0157292751281468,
-0.0100344201936282));
#17287=CARTESIAN_POINT('Ctrl Pts',(0.00339578086798491,-0.0155701528309282,
-0.0134999511106268));
#17288=CARTESIAN_POINT('Ctrl Pts',(0.000721291791339459,-0.0154110305337097,
-0.0157485703134361));
#17289=CARTESIAN_POINT('Ctrl Pts',(-0.00261610278505474,-0.0152519082364911,
-0.0147136818936349));
#17290=CARTESIAN_POINT('Ctrl Pts',(-0.00354916337254134,-0.0150927859392726,
-0.0113464041316556));
#17291=CARTESIAN_POINT('Ctrl Pts',(-0.00122037285621386,-0.0149336636420541,
-0.0087414267534739));
#17292=CARTESIAN_POINT('Ctrl Pts',(0.00223001774343573,-0.0147745413448354,
-0.00929286967553652));
#17293=CARTESIAN_POINT('Ctrl Pts',(0.00363087832907891,-0.014615419047617,
-0.0124938998508358));
#17294=CARTESIAN_POINT('Ctrl Pts',(0.00169484181624943,-0.0144562967503983,
-0.0154026674369236));
#17295=CARTESIAN_POINT('Ctrl Pts',(-0.00179896197323913,-0.0142971744531799,
-0.0153457558166395));
#17296=CARTESIAN_POINT('Ctrl Pts',(-0.00363918859437698,-0.0141380521559613,
-0.0123756919760434));
#17297=CARTESIAN_POINT('Ctrl Pts',(-0.00213529131716607,-0.0139789298587427,
-0.00922167683034632));
#17298=CARTESIAN_POINT('Ctrl Pts',(0.00133197569244577,-0.0138198075615242,
-0.00878326703770384));
#17299=CARTESIAN_POINT('Ctrl Pts',(0.00357326082692228,-0.0136606852643056,
-0.0114616961695499));
#17300=CARTESIAN_POINT('Ctrl Pts',(0.00253416193417905,-0.0135015629670871,
-0.014798673676204));
#17301=CARTESIAN_POINT('Ctrl Pts',(-0.000841782375526419,-0.0133424219652438,
-0.0157208707042176));
#17302=CARTESIAN_POINT('Ctrl Pts',(-0.00256461850675379,-0.01323632172914,
-0.0141691068247504));
#17303=CARTESIAN_POINT('Ctrl Pts',(-0.00290610796466779,-0.0131832622587755,
-0.0132002457902267));
#17304=CARTESIAN_POINT('Ctrl Pts',(0.00178014132164786,-0.0271787743898808,
-0.0139559946082058));
#17305=CARTESIAN_POINT('Ctrl Pts',(0.00159188778177753,-0.027178774389881,
-0.0141905448606472));
#17306=CARTESIAN_POINT('Ctrl Pts',(0.00136108477584615,-0.0271787743898809,
-0.0143859446782764));
#17307=CARTESIAN_POINT('Ctrl Pts',(0.00110253657449065,-0.0271787743898808,
-0.0145397492409188));
#17308=CARTESIAN_POINT('Ctrl Pts',(0.00108435986445509,-0.0271787743898808,
-0.014550562160609));
#17309=CARTESIAN_POINT('Ctrl Pts',(0.00106604363144548,-0.0271787743898808,
-0.0145611678146568));
#17310=CARTESIAN_POINT('Ctrl Pts',(0.00104759204748925,-0.0271787743898808,
-0.0145715645217343));
#17311=CARTESIAN_POINT('Ctrl Pts',(0.00102977915444992,-0.0271787743898808,
-0.0145816013528038));
#17312=CARTESIAN_POINT('Ctrl Pts',(0.00101183438704971,-0.0271787743898808,
-0.0145914463741348));
#17313=CARTESIAN_POINT('Ctrl Pts',(0.000993792858541382,-0.0271787743898807,
-0.0146010815780363));
#17314=CARTESIAN_POINT('Ctrl Pts',(0.000750757191878033,-0.0271787743898806,
-0.0147308764677853));
#17315=CARTESIAN_POINT('Ctrl Pts',(0.000489586583346331,-0.0271787743898804,
-0.0148233339409982));
#17316=CARTESIAN_POINT('Ctrl Pts',(0.000220202998773276,-0.02717877438988,
-0.0148759520475625));
#17317=CARTESIAN_POINT('Ctrl Pts',(0.000185586155698519,-0.02717877438988,
-0.0148827136798301));
#17318=CARTESIAN_POINT('Ctrl Pts',(0.000150830466630735,-0.0271787743898799,
-0.0148888130189507));
#17319=CARTESIAN_POINT('Ctrl Pts',(0.000115954661106575,-0.0271787743898799,
-0.0148942405572793));
#17320=CARTESIAN_POINT('Ctrl Pts',(9.56456236842798E-5,-0.0271787743898799,
-0.0148974011460418));
#17321=CARTESIAN_POINT('Ctrl Pts',(7.52958492378998E-5,-0.0271787743898798,
-0.0149003339054926));
#17322=CARTESIAN_POINT('Ctrl Pts',(5.49090021173358E-5,-0.0271787743898798,
-0.0149030367816552));
#17323=CARTESIAN_POINT('Ctrl Pts',(4.02446667567445E-5,-0.0271787743898798,
-0.014904980970585));
#17324=CARTESIAN_POINT('Ctrl Pts',(2.55602201095934E-5,-0.0271787743898798,
-0.0149068062467938));
#17325=CARTESIAN_POINT('Ctrl Pts',(1.08737028632742E-5,-0.0271787743898796,
-0.0149085100975743));
#17326=CARTESIAN_POINT('Ctrl Pts',(-8.37418793519446E-5,-0.0271787743898786,
-0.0149194868887972));
#17327=CARTESIAN_POINT('Ctrl Pts',(-0.000178600902109579,-0.0271787743898791,
-0.0149254498948637));
#17328=CARTESIAN_POINT('Ctrl Pts',(-0.000273310347805921,-0.0271787743898792,
-0.0149263099508221));
#17329=CARTESIAN_POINT('Ctrl Pts',(-0.000367683085058819,-0.0271787743898794,
-0.014927166949133));
#17330=CARTESIAN_POINT('Ctrl Pts',(-0.000461908229692522,-0.0271787743898795,
-0.0149229576474026));
#17331=CARTESIAN_POINT('Ctrl Pts',(-0.000555618552463728,-0.0271787743898797,
-0.0149135474060006));
#17332=CARTESIAN_POINT('Ctrl Pts',(-0.000568622442957223,-0.0271787743898797,
-0.0149122415760227));
#17333=CARTESIAN_POINT('Ctrl Pts',(-0.000581616441170821,-0.0271787743898797,
-0.0149108355161016));
#17334=CARTESIAN_POINT('Ctrl Pts',(-0.000594599583223318,-0.0271787743898797,
-0.0149093287881527));
#17335=CARTESIAN_POINT('Ctrl Pts',(-0.000686222435460218,-0.0271787743898799,
-0.0148986957139969));
#17336=CARTESIAN_POINT('Ctrl Pts',(-0.000777304615406129,-0.02717877438988,
-0.0148830535254043));
#17337=CARTESIAN_POINT('Ctrl Pts',(-0.000867587973888055,-0.0271787743898801,
-0.014862658476978));
#17338=CARTESIAN_POINT('Ctrl Pts',(-0.000904118649592721,-0.0271787743898802,
-0.0148544061820637));
#17339=CARTESIAN_POINT('Ctrl Pts',(-0.00094051853516899,-0.0271787743898802,
-0.0148453751478637));
#17340=CARTESIAN_POINT('Ctrl Pts',(-0.000976770333537329,-0.0271787743898803,
-0.0148355799669997));
#17341=CARTESIAN_POINT('Ctrl Pts',(-0.000991818294032867,-0.0271787743898803,
-0.0148315140309269));
#17342=CARTESIAN_POINT('Ctrl Pts',(-0.00100684073583925,-0.0271787743898803,
-0.0148273164133904));
#17343=CARTESIAN_POINT('Ctrl Pts',(-0.00102183640859416,-0.0271787743898803,
-0.014822988092282));
#17344=CARTESIAN_POINT('Ctrl Pts',(-0.001313021104889,-0.0271787743898808,
-0.014738941121665));
#17345=CARTESIAN_POINT('Ctrl Pts',(-0.00158953777575494,-0.0271787743898808,
-0.014607373158194));
#17346=CARTESIAN_POINT('Ctrl Pts',(-0.0018425581172716,-0.027178774389881,
-0.0144374263141347));
#17347=CARTESIAN_POINT('Ctrl Pts',(-0.00187516285324282,-0.027178774389881,
-0.0144155266046233));
#17348=CARTESIAN_POINT('Ctrl Pts',(-0.00190737673303968,-0.027178774389881,
-0.0143929827017157));
#17349=CARTESIAN_POINT('Ctrl Pts',(-0.00193917946553789,-0.027178774389881,
-0.0143698084371997));
#17350=CARTESIAN_POINT('Ctrl Pts',(-0.00196084834500122,-0.027178774389881,
-0.0143540185881836));
#17351=CARTESIAN_POINT('Ctrl Pts',(-0.00198232634019788,-0.027178774389881,
-0.0143379360750785));
#17352=CARTESIAN_POINT('Ctrl Pts',(-0.00200360683979679,-0.027178774389881,
-0.0143215649815428));
#17353=CARTESIAN_POINT('Ctrl Pts',(-0.002016225356077,-0.027178774389881,
-0.0143118575538884));
#17354=CARTESIAN_POINT('Ctrl Pts',(-0.00202877384413721,-0.027178774389881,
-0.0143020490191849));
#17355=CARTESIAN_POINT('Ctrl Pts',(-0.00204124055375976,-0.027178774389881,
-0.0142921487089482));
#17356=CARTESIAN_POINT('Ctrl Pts',(-0.00218907523485341,-0.0271787743898811,
-0.0141747473054594));
#17357=CARTESIAN_POINT('Ctrl Pts',(-0.00232581856094753,-0.0271787743898811,
-0.0140441925400865));
#17358=CARTESIAN_POINT('Ctrl Pts',(-0.0024493802750837,-0.0271787743898811,
-0.0139022590018999));
#17359=CARTESIAN_POINT('Ctrl Pts',(-0.0024731161684946,-0.027178774389881,
-0.0138749939274602));
#17360=CARTESIAN_POINT('Ctrl Pts',(-0.00249636476998995,-0.027178774389881,
-0.013847307320566));
#17361=CARTESIAN_POINT('Ctrl Pts',(-0.00251910979700554,-0.027178774389881,
-0.01381920955006));
#17362=CARTESIAN_POINT('Ctrl Pts',(-0.00253166456181397,-0.027178774389881,
-0.0138037001861844));
#17363=CARTESIAN_POINT('Ctrl Pts',(-0.0025440610497504,-0.027178774389881,
-0.013788071445362));
#17364=CARTESIAN_POINT('Ctrl Pts',(-0.00255629300276171,-0.027178774389881,
-0.0137723303642783));
#17365=CARTESIAN_POINT('Ctrl Pts',(-0.00268294210004683,-0.0271787743898809,
-0.0136093479110518));
#17366=CARTESIAN_POINT('Ctrl Pts',(-0.00279213110827008,-0.0271787743898808,
-0.0134342130497224));
#17367=CARTESIAN_POINT('Ctrl Pts',(-0.00288099910591139,-0.0271787743898807,
-0.0132489814220675));
#17368=CARTESIAN_POINT('Ctrl Pts',(-0.00288859728608324,-0.0271787743898807,
-0.0132331441879922));
#17369=CARTESIAN_POINT('Ctrl Pts',(-0.00289604652716329,-0.0271787743899213,
-0.0132172327756286));
#17370=CARTESIAN_POINT('Ctrl Pts',(-0.00290334727505161,-0.027178774389873,
-0.0132012491818455));
#17371=CARTESIAN_POINT('Ctrl Pts',(-0.00133026104482802,-0.0271737656056343,
-0.00939549384111197));
#17372=CARTESIAN_POINT('Ctrl Pts',(-0.000403564519673555,-0.0271207189867622,
-0.00895210654872306));
#17373=CARTESIAN_POINT('Ctrl Pts',(0.00191213026985457,-0.0270146316021502,
-0.00907331532630318));
#17374=CARTESIAN_POINT('Ctrl Pts',(0.00364752743133458,-0.0268555034517987,
-0.0121131487462191));
#17375=CARTESIAN_POINT('Ctrl Pts',(0.00202223804807116,-0.0266963811545802,
-0.0152083353095718));
#17376=CARTESIAN_POINT('Ctrl Pts',(-0.00145746560947327,-0.0265372588573616,
-0.0155175293308395));
#17377=CARTESIAN_POINT('Ctrl Pts',(-0.00359977297117066,-0.026378136560143,
-0.0127550489129778));
#17378=CARTESIAN_POINT('Ctrl Pts',(-0.00243264631344909,-0.0262190142629245,
-0.00946051572784691));
#17379=CARTESIAN_POINT('Ctrl Pts',(0.000969663846264036,-0.0260598919657059,
-0.00866138325036077));
#17380=CARTESIAN_POINT('Ctrl Pts',(0.00348107948700157,-0.0259007696684874,
-0.0110922917925086));
#17381=CARTESIAN_POINT('Ctrl Pts',(0.00279306816967889,-0.0257416473712688,
-0.0145190138345622));
#17382=CARTESIAN_POINT('Ctrl Pts',(-0.000461841671043204,-0.0255825250740504,
-0.0157922709603413));
#17383=CARTESIAN_POINT('Ctrl Pts',(-0.00329233215877127,-0.0254234027768317,
-0.0137418498867445));
#17384=CARTESIAN_POINT('Ctrl Pts',(-0.00309698560073088,-0.0252642804796132,
-0.0102522037919197));
#17385=CARTESIAN_POINT('Ctrl Pts',(-5.5363207118422E-5,-0.0251051581823947,
-0.00853048588183138));
#17386=CARTESIAN_POINT('Ctrl Pts',(0.0030371455487437,-0.0249460358851761,
-0.0101590447958442));
#17387=CARTESIAN_POINT('Ctrl Pts',(0.00333836262133237,-0.0247869135879575,
-0.0136411513774764));
#17388=CARTESIAN_POINT('Ctrl Pts',(0.000571458082834102,-0.024627791290739,
-0.0157765757479082));
#17389=CARTESIAN_POINT('Ctrl Pts',(-0.00272064575727319,-0.0244686689935204,
-0.0146027552459517));
#17390=CARTESIAN_POINT('Ctrl Pts',(-0.00351233923191389,-0.0243095466963019,
-0.0111984900766984));
#17391=CARTESIAN_POINT('Ctrl Pts',(-0.00107601677663968,-0.0241504243990833,
-0.00869247072691854));
#17392=CARTESIAN_POINT('Ctrl Pts',(0.00234921920222027,-0.0239913021018648,
-0.00938785485574907));
#17393=CARTESIAN_POINT('Ctrl Pts',(0.00361540474722111,-0.0238321798046462,
-0.0126455495059498));
#17394=CARTESIAN_POINT('Ctrl Pts',(0.0015588518368198,-0.0236730575074277,
-0.0154715697542866));
#17395=CARTESIAN_POINT('Ctrl Pts',(-0.00193036418608369,-0.0235139352102091,
-0.0152686611019598));
#17396=CARTESIAN_POINT('Ctrl Pts',(-0.00364547860084178,-0.0233548129129906,
-0.0122233067916808));
#17397=CARTESIAN_POINT('Ctrl Pts',(-0.00201021516003761,-0.0231956906157721,
-0.00913434032706003));
#17398=CARTESIAN_POINT('Ctrl Pts',(0.00147253693880004,-0.0230365683185534,
-0.00884067697422658));
#17399=CARTESIAN_POINT('Ctrl Pts',(0.00360195366021276,-0.022877446021335,
-0.0116122080975127));
#17400=CARTESIAN_POINT('Ctrl Pts',(0.00242099412922516,-0.0227183237241164,
-0.0149017574478925));
#17401=CARTESIAN_POINT('Ctrl Pts',(-0.000984980554711353,-0.0225592014268979,
-0.015686064017702));
#17402=CARTESIAN_POINT('Ctrl Pts',(-0.0034857086570125,-0.0224000791296793,
-0.0132443106926007));
#17403=CARTESIAN_POINT('Ctrl Pts',(-0.0027828955007027,-0.0222409568324608,
-0.00982059136855261));
#17404=CARTESIAN_POINT('Ctrl Pts',(0.000477538338332731,-0.0220818345352422,
-0.00856147599501673));
#17405=CARTESIAN_POINT('Ctrl Pts',(0.00329909046922294,-0.0219227122380236,
-0.0106241548151851));
#17406=CARTESIAN_POINT('Ctrl Pts',(0.00308861282535697,-0.0217635899408051,
-0.0141129224348428));
#17407=CARTESIAN_POINT('Ctrl Pts',(3.95449286407195E-5,-0.0216044676435865,
-0.0158214262550787));
#17408=CARTESIAN_POINT('Ctrl Pts',(-0.00304586674288027,-0.021445345346368,
-0.014179465488259));
#17409=CARTESIAN_POINT('Ctrl Pts',(-0.00333197395745346,-0.0212862230491495,
-0.0106960845150796));
#17410=CARTESIAN_POINT('Ctrl Pts',(-0.000555829820637072,-0.0211271007519309,
-0.00857268533589575));
#17411=CARTESIAN_POINT('Ctrl Pts',(0.00273114982723726,-0.0209679784547124,
-0.00976077840337707));
#17412=CARTESIAN_POINT('Ctrl Pts',(0.00350806566426024,-0.0208088561574938,
-0.0131684465393202));
#17413=CARTESIAN_POINT('Ctrl Pts',(0.0010608930305098,-0.0206497338602753,
-0.0156638716420152));
#17414=CARTESIAN_POINT('Ctrl Pts',(-0.00236129356128513,-0.0204906115630567,
-0.0149536327572187));
#17415=CARTESIAN_POINT('Ctrl Pts',(-0.00361333281957622,-0.0203314892658382,
-0.011690475078185));
#17416=CARTESIAN_POINT('Ctrl Pts',(-0.00154453780633458,-0.0201723669686196,
-0.00887340434145793));
#17417=CARTESIAN_POINT('Ctrl Pts',(0.00194376499571779,-0.020013244671401,
-0.00909144998743974));
#17418=CARTESIAN_POINT('Ctrl Pts',(0.0036456501783873,-0.0198541223741825,
-0.0121442171203124));
#17419=CARTESIAN_POINT('Ctrl Pts',(0.00199699981425714,-0.019695000076964,
-0.0152260594782847));
#17420=CARTESIAN_POINT('Ctrl Pts',(-0.00148699364019134,-0.0195358777797454,
-0.0155046092079528));
#17421=CARTESIAN_POINT('Ctrl Pts',(-0.00360436528356685,-0.0193767554825269,
-0.0127238651229339));
#17422=CARTESIAN_POINT('Ctrl Pts',(-0.00240914427122477,-0.0192176331853083,
-0.00943947064690133));
#17423=CARTESIAN_POINT('Ctrl Pts',(0.00100020127943993,-0.0190585108880898,
-0.00866994919905135));
#17424=CARTESIAN_POINT('Ctrl Pts',(0.00349031163837243,-0.0188993885908712,
-0.0111225296244144));
#17425=CARTESIAN_POINT('Ctrl Pts',(0.0027726503676781,-0.0187402662936527,
-0.0145431673782673));
#17426=CARTESIAN_POINT('Ctrl Pts',(-0.000493215794101875,-0.0185811439964341,
-0.0157881246288907));
#17427=CARTESIAN_POINT('Ctrl Pts',(-0.00330579187879757,-0.0184220216992156,
-0.0137132231588611));
#17428=CARTESIAN_POINT('Ctrl Pts',(-0.00308017925688279,-0.018262899401997,
-0.0102254015912665));
#17429=CARTESIAN_POINT('Ctrl Pts',(-2.3727254960886E-5,-0.0181037771047785,
-0.00853014305567693));
#17430=CARTESIAN_POINT('Ctrl Pts',(0.00305453128551212,-0.0179446548075599,
-0.0101854752581386));
#17431=CARTESIAN_POINT('Ctrl Pts',(0.0033255222193557,-0.0177855325103414,
-0.0136700647972919));
#17432=CARTESIAN_POINT('Ctrl Pts',(0.000540191273020311,-0.0176264102131228,
-0.0157813989399443));
#17433=CARTESIAN_POINT('Ctrl Pts',(-0.00274160257393495,-0.0174672879159043,
-0.0145790556077934));
#17434=CARTESIAN_POINT('Ctrl Pts',(-0.00350372601109839,-0.0173081656186857,
-0.0111680486876026));
#17435=CARTESIAN_POINT('Ctrl Pts',(-0.00104574933649522,-0.0171490433214672,
-0.00868326479166292));
#17436=CARTESIAN_POINT('Ctrl Pts',(0.00237332348080628,-0.0169899210242486,
-0.009408345070505));
#17437=CARTESIAN_POINT('Ctrl Pts',(0.00361119286507359,-0.0168307987270301,
-0.0126769043455143));
#17438=CARTESIAN_POINT('Ctrl Pts',(0.0015301947024884,-0.0166716764298115,
-0.0154849725405016));
#17439=CARTESIAN_POINT('Ctrl Pts',(-0.00195712921450782,-0.016512554132593,
-0.0152517940063453));
#17440=CARTESIAN_POINT('Ctrl Pts',(-0.00364575312774022,-0.0163534318353744,
-0.0121916715160949));
#17441=CARTESIAN_POINT('Ctrl Pts',(-0.00198374687138292,-0.0161943095381559,
-0.00911701128752997));
#17442=CARTESIAN_POINT('Ctrl Pts',(0.00150142234134212,-0.0160351872409373,
-0.00885358041046971));
#17443=CARTESIAN_POINT('Ctrl Pts',(0.00360670906987409,-0.0158760649437188,
-0.0116434851379063));
#17444=CARTESIAN_POINT('Ctrl Pts',(0.00239724903111026,-0.0157169426465002,
-0.0149226628552886));
#17445=CARTESIAN_POINT('Ctrl Pts',(-0.00101540311647332,-0.0155578203492816,
-0.0156773848040705));
#17446=CARTESIAN_POINT('Ctrl Pts',(-0.00349484903028939,-0.0153986980520632,
-0.0132140232339141));
#17447=CARTESIAN_POINT('Ctrl Pts',(-0.00276235281219855,-0.0152395757548446,
-0.0097965318648716));
#17448=CARTESIAN_POINT('Ctrl Pts',(0.00050888351868074,-0.0150804534576261,
-0.0085657553464899));
#17449=CARTESIAN_POINT('Ctrl Pts',(0.0033124319335464,-0.0149213311604074,
-0.0106528420306022));
#17450=CARTESIAN_POINT('Ctrl Pts',(0.00307168598205126,-0.014762208863189,
-0.0141396486977521));
#17451=CARTESIAN_POINT('Ctrl Pts',(7.91251657260586E-6,-0.0146030865659703,
-0.0158216363008853));
#17452=CARTESIAN_POINT('Ctrl Pts',(-0.00306314496881806,-0.0144439642687519,
-0.0141529515189099));
#17453=CARTESIAN_POINT('Ctrl Pts',(-0.00331899483268342,-0.0142848419715333,
-0.0106672431795996));
#17454=CARTESIAN_POINT('Ctrl Pts',(-0.000524568178194816,-0.0141257196743148,
-0.00856796635198887));
#17455=CARTESIAN_POINT('Ctrl Pts',(0.00275205403218279,-0.0139665973770961,
-0.00978463054201357));
#17456=CARTESIAN_POINT('Ctrl Pts',(0.003499221564516,-0.0138074750798777,
-0.0131987289322313));
#17457=CARTESIAN_POINT('Ctrl Pts',(0.0010307800885073,-0.0136483527826591,
-0.0156731844728732));
#17458=CARTESIAN_POINT('Ctrl Pts',(-0.00238569018355137,-0.0134892304854405,
-0.0149325700177128));
#17459=CARTESIAN_POINT('Ctrl Pts',(-0.00360823372354723,-0.013330108188222,
-0.0116600593943641));
#17460=CARTESIAN_POINT('Ctrl Pts',(-0.00151732056346516,-0.0131709858910035,
-0.00885830501571057));
#17461=CARTESIAN_POINT('Ctrl Pts',(0.00197391249517797,-0.0130118514625948,
-0.00911217318149874));
#17462=CARTESIAN_POINT('Ctrl Pts',(0.00308245941021202,-0.0129057577999257,
-0.0111491278697729));
#17463=CARTESIAN_POINT('Ctrl Pts',(0.00308220579556829,-0.0128527049029959,
-0.0121765580884125));
#17464=CARTESIAN_POINT('Ctrl Pts',(-0.00124852020439948,-0.0272831116917783,
-0.00956633919409565));
#17465=CARTESIAN_POINT('Ctrl Pts',(-0.000378766602653055,-0.0272300650729058,
-0.00915019681732398));
#17466=CARTESIAN_POINT('Ctrl Pts',(0.00179463518430394,-0.0271239776882938,
-0.00926395765272372));
#17467=CARTESIAN_POINT('Ctrl Pts',(0.00342339701807277,-0.0269648495379425,
-0.0121170017657793));
#17468=CARTESIAN_POINT('Ctrl Pts',(0.00189797714586813,-0.0268057272407237,
-0.0150219977255996));
#17469=CARTESIAN_POINT('Ctrl Pts',(-0.00136790840242943,-0.0266466049435053,
-0.015312192634436));
#17470=CARTESIAN_POINT('Ctrl Pts',(-0.00337857693663336,-0.0264874826462867,
-0.0127194589530521));
#17471=CARTESIAN_POINT('Ctrl Pts',(-0.00228316696509127,-0.0263283603490681,
-0.00962736566678117));
#17472=CARTESIAN_POINT('Ctrl Pts',(0.000910080700508586,-0.0261692380518497,
-0.00887733765685602));
#17473=CARTESIAN_POINT('Ctrl Pts',(0.00326717683686211,-0.026010115754631,
-0.011158873631858));
#17474=CARTESIAN_POINT('Ctrl Pts',(0.00262144190094663,-0.0258509934574125,
-0.0143750331375423));
#17475=CARTESIAN_POINT('Ctrl Pts',(-0.000433462785197627,-0.0256918711601939,
-0.0155700521551341));
#17476=CARTESIAN_POINT('Ctrl Pts',(-0.00309002750685791,-0.0255327488629754,
-0.0136456237522536));
#17477=CARTESIAN_POINT('Ctrl Pts',(-0.00290668445135645,-0.0253736265657569,
-0.0103704067017869));
#17478=CARTESIAN_POINT('Ctrl Pts',(-5.19612920610198E-5,-0.0252145042685382,
-0.00875448356746734));
#17479=CARTESIAN_POINT('Ctrl Pts',(0.0028505214040893,-0.0250553819713197,
-0.0102829720668527));
#17480=CARTESIAN_POINT('Ctrl Pts',(0.00313322952555102,-0.0248962596741012,
-0.0135511128862376));
#17481=CARTESIAN_POINT('Ctrl Pts',(0.000536343573436004,-0.0247371373768827,
-0.0155553213698408));
#17482=CARTESIAN_POINT('Ctrl Pts',(-0.00255346964430465,-0.0245780150796641,
-0.0144536288721698));
#17483=CARTESIAN_POINT('Ctrl Pts',(-0.00329651575741394,-0.0244188927824455,
-0.0112585463269271));
#17484=CARTESIAN_POINT('Ctrl Pts',(-0.0010098985391857,-0.024259770485227,
-0.0089065148944645));
#17485=CARTESIAN_POINT('Ctrl Pts',(0.00220486621775386,-0.0241006481880085,
-0.00955916960313173));
#17486=CARTESIAN_POINT('Ctrl Pts',(0.003393248183533,-0.02394152589079,
-0.0126166879799594));
#17487=CARTESIAN_POINT('Ctrl Pts',(0.00146306472816122,-0.0237824035935714,
-0.015269057146003));
#17488=CARTESIAN_POINT('Ctrl Pts',(-0.00181174867710741,-0.0236232812963528,
-0.0150786166658714));
#17489=CARTESIAN_POINT('Ctrl Pts',(-0.00342147408251391,-0.0234641589991344,
-0.0122203909058064));
#17490=CARTESIAN_POINT('Ctrl Pts',(-0.00188669303085664,-0.0233050367019156,
-0.00932123283695521));
#17491=CARTESIAN_POINT('Ctrl Pts',(0.0013820536404974,-0.0231459144046971,
-0.00904561428018408));
#17492=CARTESIAN_POINT('Ctrl Pts',(0.0033806236284005,-0.0229867921074786,
-0.011646842526323));
#17493=CARTESIAN_POINT('Ctrl Pts',(0.00227223077517162,-0.02282766981026,
-0.0147342582206233));
#17494=CARTESIAN_POINT('Ctrl Pts',(-0.000924456239832787,-0.0226685475130416,
-0.0154703713336528));
#17495=CARTESIAN_POINT('Ctrl Pts',(-0.00327152155725417,-0.022509425215823,
-0.0131786569574399));
#17496=CARTESIAN_POINT('Ctrl Pts',(-0.00261189431417872,-0.0223503029186044,
-0.00996531566109326));
#17497=CARTESIAN_POINT('Ctrl Pts',(0.000448194935950225,-0.0221911806213858,
-0.00878356942441171));
#17498=CARTESIAN_POINT('Ctrl Pts',(0.00309637053793389,-0.0220320583241672,
-0.0107195023694375));
#17499=CARTESIAN_POINT('Ctrl Pts',(0.00289882615973626,-0.0218729360269489,
-0.0139938949245925));
#17500=CARTESIAN_POINT('Ctrl Pts',(3.71150027894397E-5,-0.0217138137297301,
-0.0155974159381194));
#17501=CARTESIAN_POINT('Ctrl Pts',(-0.00285870670510849,-0.0215546914325116,
-0.0140563490924984));
#17502=CARTESIAN_POINT('Ctrl Pts',(-0.00312723342729426,-0.0213955691352931,
-0.0107870121893814));
#17503=CARTESIAN_POINT('Ctrl Pts',(-0.000521675624473279,-0.0212364468380746,
-0.00879408998247798));
#17504=CARTESIAN_POINT('Ctrl Pts',(0.00256332826839168,-0.021077324540856,
-0.00990917803622847));
#17505=CARTESIAN_POINT('Ctrl Pts',(0.00329250478860355,-0.0209182022436374,
-0.0131074544453246));
#17506=CARTESIAN_POINT('Ctrl Pts',(0.000995704105181346,-0.0207590799464189,
-0.015449542617713));
#17507=CARTESIAN_POINT('Ctrl Pts',(-0.00221619864104495,-0.0205999576492002,
-0.0147829459365079));
#17508=CARTESIAN_POINT('Ctrl Pts',(-0.00339130357007781,-0.020440835351982,
-0.011720300218771));
#17509=CARTESIAN_POINT('Ctrl Pts',(-0.00144963025502779,-0.0202817130547632,
-0.00907633064174633));
#17510=CARTESIAN_POINT('Ctrl Pts',(0.00182432604427043,-0.0201225907575447,
-0.00928097798938392));
#17511=CARTESIAN_POINT('Ctrl Pts',(0.00342163511709659,-0.0199634684603261,
-0.0121461610747165));
#17512=CARTESIAN_POINT('Ctrl Pts',(0.0018742897313094,-0.0198043461631076,
-0.0150386327934535));
#17513=CARTESIAN_POINT('Ctrl Pts',(-0.00139562201780662,-0.0196452238658891,
-0.0153000664171568));
#17514=CARTESIAN_POINT('Ctrl Pts',(-0.0033828870642086,-0.0194861015686706,
-0.0126901913201535));
#17515=CARTESIAN_POINT('Ctrl Pts',(-0.00226110905797912,-0.0193269792714519,
-0.00960761374751241));
#17516=CARTESIAN_POINT('Ctrl Pts',(0.000938741693370724,-0.0191678569742334,
-0.00888537725182994));
#17517=CARTESIAN_POINT('Ctrl Pts',(0.00327584169821501,-0.0190087346770149,
-0.0111872534331147));
#17518=CARTESIAN_POINT('Ctrl Pts',(0.00260227871607661,-0.0188496123797963,
-0.0143977025131817));
#17519=CARTESIAN_POINT('Ctrl Pts',(-0.000462909055676917,-0.0186904900825777,
-0.0155661606042158));
#17520=CARTESIAN_POINT('Ctrl Pts',(-0.00310266016453344,-0.0185313677853593,
-0.0136187560571594));
#17521=CARTESIAN_POINT('Ctrl Pts',(-0.0028909108105827,-0.0183722454881406,
-0.0103452514218003));
#17522=CARTESIAN_POINT('Ctrl Pts',(-2.22692811525819E-5,-0.0182131231909222,
-0.00875416180702642));
#17523=CARTESIAN_POINT('Ctrl Pts',(0.00286683883570031,-0.0180540008937035,
-0.0103077784507683));
#17524=CARTESIAN_POINT('Ctrl Pts',(0.00312117813055393,-0.017894878596485,
-0.0135782496568423));
#17525=CARTESIAN_POINT('Ctrl Pts',(0.000506998022101241,-0.0177357562992665,
-0.0155598481901445));
#17526=CARTESIAN_POINT('Ctrl Pts',(-0.00257313872288425,-0.0175766340020479,
-0.0144313855108441));
#17527=CARTESIAN_POINT('Ctrl Pts',(-0.00328843179505563,-0.0174175117048294,
-0.0112299754765036));
#17528=CARTESIAN_POINT('Ctrl Pts',(-0.000981490949034324,-0.0172583894076109,
-0.00889787463831949));
#17529=CARTESIAN_POINT('Ctrl Pts',(0.00222748935547867,-0.0170992671103922,
-0.00957840075119452));
#17530=CARTESIAN_POINT('Ctrl Pts',(0.00338929510982602,-0.0169401448131737,
-0.0126461161518617));
#17531=CARTESIAN_POINT('Ctrl Pts',(0.00143616849501057,-0.0167810225159553,
-0.0152816363682914));
#17532=CARTESIAN_POINT('Ctrl Pts',(-0.00183686906899497,-0.0166219002187365,
-0.015062786006358));
#17533=CARTESIAN_POINT('Ctrl Pts',(-0.00342173174049819,-0.0164627779215181,
-0.012190699529896));
#17534=CARTESIAN_POINT('Ctrl Pts',(-0.00186185114490522,-0.0163036556242994,
-0.00930496861869497));
#17535=CARTESIAN_POINT('Ctrl Pts',(0.00140916411541224,-0.016144533327081,
-0.00905772483616733));
#17536=CARTESIAN_POINT('Ctrl Pts',(0.00338508683136765,-0.0159854110298623,
-0.0116761976795967));
#17537=CARTESIAN_POINT('Ctrl Pts',(0.00224994474727718,-0.0158262887326441,
-0.0147538790488936));
#17538=CARTESIAN_POINT('Ctrl Pts',(-0.000953009419809811,-0.0156671664354252,
-0.0154622254335535));
#17539=CARTESIAN_POINT('Ctrl Pts',(-0.00328010028002164,-0.0155080441382069,
-0.0131502305788299));
#17540=CARTESIAN_POINT('Ctrl Pts',(-0.00259261391673356,-0.0153489218409881,
-0.00994273454698003));
#17541=CARTESIAN_POINT('Ctrl Pts',(0.000477614042167904,-0.0151897995437698,
-0.00878758582164199));
#17542=CARTESIAN_POINT('Ctrl Pts',(0.00310889220639052,-0.015030677246551,
-0.0107464268352748));
#17543=CARTESIAN_POINT('Ctrl Pts',(0.00288293942386135,-0.0148715549493327,
-0.0140189789329983));
#17544=CARTESIAN_POINT('Ctrl Pts',(7.42631444178104E-6,-0.0147124326521141,
-0.0155976130771956));
#17545=CARTESIAN_POINT('Ctrl Pts',(-0.0028749232321303,-0.0145533103548955,
-0.0140314643328042));
#17546=CARTESIAN_POINT('Ctrl Pts',(-0.0031150518336335,-0.0143941880576769,
-0.0107599430737303));
#17547=CARTESIAN_POINT('Ctrl Pts',(-0.000492334922989443,-0.0142350657604584,
-0.00878966096700406));
#17548=CARTESIAN_POINT('Ctrl Pts',(0.00258294796809865,-0.0140759434632399,
-0.00993156452730224));
#17549=CARTESIAN_POINT('Ctrl Pts',(0.00328420413418439,-0.0139168211660213,
-0.013135876069437));
#17550=CARTESIAN_POINT('Ctrl Pts',(0.000967441519690922,-0.0137576988688027,
-0.0154582832010229));
#17551=CARTESIAN_POINT('Ctrl Pts',(-0.00223909615874415,-0.0135985765715841,
-0.0147631774437484));
#17552=CARTESIAN_POINT('Ctrl Pts',(-0.00338651779931415,-0.0134394542743657,
-0.0116917534941046));
#17553=CARTESIAN_POINT('Ctrl Pts',(-0.00142408543601453,-0.013280331977147,
-0.00906215912755997));
#17554=CARTESIAN_POINT('Ctrl Pts',(0.0018526210637589,-0.0131211975487384,
-0.00930042780081984));
#17555=CARTESIAN_POINT('Ctrl Pts',(0.00289305085483324,-0.0130151038860693,
-0.011212217290292));
#17556=CARTESIAN_POINT('Ctrl Pts',(0.00289281282410381,-0.0129620509891397,
-0.0121765147802993));
#17557=CARTESIAN_POINT('Ctrl Pts',(-0.00116677936397096,-0.0273924577779218,
-0.00973718454707944));
#17558=CARTESIAN_POINT('Ctrl Pts',(-0.000353968685632551,-0.0273394111590494,
-0.00934828708592501));
#17559=CARTESIAN_POINT('Ctrl Pts',(0.00167714009875331,-0.0272333237744374,
-0.00945459997914426));
#17560=CARTESIAN_POINT('Ctrl Pts',(0.00319926660481094,-0.0270741956240859,
-0.0121208547853397));
#17561=CARTESIAN_POINT('Ctrl Pts',(0.00177371624366508,-0.0269150733268674,
-0.0148356601416275));
#17562=CARTESIAN_POINT('Ctrl Pts',(-0.00127835119538558,-0.0267559510296487,
-0.0151068559380321));
#17563=CARTESIAN_POINT('Ctrl Pts',(-0.00315738090209607,-0.0265968287324303,
-0.0126838689931265));
#17564=CARTESIAN_POINT('Ctrl Pts',(-0.00213368761673345,-0.0264377064352117,
-0.00979421560571543));
#17565=CARTESIAN_POINT('Ctrl Pts',(0.000850497554753141,-0.0262785841379932,
-0.00909329206335137));
#17566=CARTESIAN_POINT('Ctrl Pts',(0.00305327418672263,-0.0261194618407746,
-0.0112254554712075));
#17567=CARTESIAN_POINT('Ctrl Pts',(0.00244981563221435,-0.0259603395435561,
-0.0142310524405224));
#17568=CARTESIAN_POINT('Ctrl Pts',(-0.000405083899352055,-0.0258012172463375,
-0.0153478333499265));
#17569=CARTESIAN_POINT('Ctrl Pts',(-0.00288772285494454,-0.025642094949119,
-0.013549397617763));
#17570=CARTESIAN_POINT('Ctrl Pts',(-0.00271638330198203,-0.0254829726519004,
-0.0104886096116541));
#17571=CARTESIAN_POINT('Ctrl Pts',(-4.85593770036155E-5,-0.0253238503546819,
-0.00897848125310329));
#17572=CARTESIAN_POINT('Ctrl Pts',(0.00266389725943493,-0.0251647280574633,
-0.0104068993378612));
#17573=CARTESIAN_POINT('Ctrl Pts',(0.00292809642976967,-0.0250056057602447,
-0.0134610743949989));
#17574=CARTESIAN_POINT('Ctrl Pts',(0.000501229064037909,-0.0248464834630263,
-0.0153340669917736));
#17575=CARTESIAN_POINT('Ctrl Pts',(-0.0023862935313361,-0.0246873611658076,
-0.0143045024983878));
#17576=CARTESIAN_POINT('Ctrl Pts',(-0.00308069228291397,-0.0245282388685892,
-0.011318602577156));
#17577=CARTESIAN_POINT('Ctrl Pts',(-0.000943780301731716,-0.0243691165713705,
-0.00912055906201046));
#17578=CARTESIAN_POINT('Ctrl Pts',(0.00206051323328746,-0.0242099942741521,
-0.00973048435051448));
#17579=CARTESIAN_POINT('Ctrl Pts',(0.00317109161984489,-0.0240508719769334,
-0.0125878264539693));
#17580=CARTESIAN_POINT('Ctrl Pts',(0.00136727761950265,-0.023891749679715,
-0.0150665445377193));
#17581=CARTESIAN_POINT('Ctrl Pts',(-0.00169313316813111,-0.0237326273824963,
-0.0148885722297828));
#17582=CARTESIAN_POINT('Ctrl Pts',(-0.00319746956418605,-0.0235735050852778,
-0.0122174750199319));
#17583=CARTESIAN_POINT('Ctrl Pts',(-0.00176317090167569,-0.0234143827880593,
-0.00950812534685026));
#17584=CARTESIAN_POINT('Ctrl Pts',(0.00129157034219474,-0.0232552604908407,
-0.0092505515861417));
#17585=CARTESIAN_POINT('Ctrl Pts',(0.00315929359658823,-0.0230961381936222,
-0.0116814769551331));
#17586=CARTESIAN_POINT('Ctrl Pts',(0.00212346742111806,-0.0229370158964036,
-0.0145667589933541));
#17587=CARTESIAN_POINT('Ctrl Pts',(-0.000863931924954216,-0.0227778935991851,
-0.0152546786496038));
#17588=CARTESIAN_POINT('Ctrl Pts',(-0.00305733445749584,-0.0226187713019664,
-0.013113003222279));
#17589=CARTESIAN_POINT('Ctrl Pts',(-0.00244089312765475,-0.022459649004748,
-0.0101100399536339));
#17590=CARTESIAN_POINT('Ctrl Pts',(0.000418851533567719,-0.0223005267075294,
-0.00900566285380667));
#17591=CARTESIAN_POINT('Ctrl Pts',(0.00289365060664484,-0.0221414044103109,
-0.0108148499236899));
#17592=CARTESIAN_POINT('Ctrl Pts',(0.00270903949411558,-0.0219822821130924,
-0.0138748674143422));
#17593=CARTESIAN_POINT('Ctrl Pts',(3.46850769381592E-5,-0.0218231598158738,
-0.0153734056211602));
#17594=CARTESIAN_POINT('Ctrl Pts',(-0.00267154666733671,-0.0216640375186552,
-0.0139332326967378));
#17595=CARTESIAN_POINT('Ctrl Pts',(-0.00292249289713507,-0.0215049152214367,
-0.0108779398636833));
#17596=CARTESIAN_POINT('Ctrl Pts',(-0.000487521428309481,-0.0213457929242181,
-0.00901549462906021));
#17597=CARTESIAN_POINT('Ctrl Pts',(0.00239550670954607,-0.0211866706269996,
-0.0100575776690799));
#17598=CARTESIAN_POINT('Ctrl Pts',(0.00307694391294687,-0.021027548329781,
-0.0130464623513294));
#17599=CARTESIAN_POINT('Ctrl Pts',(0.000930515179852897,-0.0208684260325625,
-0.0152352135934109));
#17600=CARTESIAN_POINT('Ctrl Pts',(-0.0020711037208048,-0.0207093037353439,
-0.0146122591157974));
#17601=CARTESIAN_POINT('Ctrl Pts',(-0.00316927432057939,-0.0205501814381254,
-0.011750125359357));
#17602=CARTESIAN_POINT('Ctrl Pts',(-0.00135472270372102,-0.0203910591409068,
-0.00927925694203484));
#17603=CARTESIAN_POINT('Ctrl Pts',(0.00170488709282307,-0.0202319368436883,
-0.00947050599132809));
#17604=CARTESIAN_POINT('Ctrl Pts',(0.00319762005580587,-0.0200728145464697,
-0.0121481050291209));
#17605=CARTESIAN_POINT('Ctrl Pts',(0.00175157964836166,-0.0199136922492512,
-0.0148512061086225));
#17606=CARTESIAN_POINT('Ctrl Pts',(-0.00130425039542191,-0.0197545699520326,
-0.0150955236263609));
#17607=CARTESIAN_POINT('Ctrl Pts',(-0.00316140884485033,-0.0195954476548141,
-0.0126565175173729));
#17608=CARTESIAN_POINT('Ctrl Pts',(-0.00211307384473349,-0.0194363253575955,
-0.00977575684812358));
#17609=CARTESIAN_POINT('Ctrl Pts',(0.000877282107301528,-0.019277203060377,
-0.00910080530460862));
#17610=CARTESIAN_POINT('Ctrl Pts',(0.00306137175805757,-0.0191180807631584,
-0.0112519772418149));
#17611=CARTESIAN_POINT('Ctrl Pts',(0.00243190706447511,-0.0189589584659399,
-0.014252237648096));
#17612=CARTESIAN_POINT('Ctrl Pts',(-0.000432602317251961,-0.0187998361687213,
-0.015344196579541));
#17613=CARTESIAN_POINT('Ctrl Pts',(-0.0028995284502693,-0.0186407138715028,
-0.0135242889554577));
#17614=CARTESIAN_POINT('Ctrl Pts',(-0.00270164236428262,-0.0184815915742842,
-0.010465101252334));
#17615=CARTESIAN_POINT('Ctrl Pts',(-2.08113073442808E-5,-0.0183224692770657,
-0.0089781805583758));
#17616=CARTESIAN_POINT('Ctrl Pts',(0.0026791463858885,-0.0181633469798471,
-0.0104300816433981));
#17617=CARTESIAN_POINT('Ctrl Pts',(0.00291683404175214,-0.0180042246826286,
-0.0134864345163929));
#17618=CARTESIAN_POINT('Ctrl Pts',(0.000473804771182178,-0.0178451023854101,
-0.0153382974403444));
#17619=CARTESIAN_POINT('Ctrl Pts',(-0.00240467487183354,-0.0176859800881915,
-0.0142837154138948));
#17620=CARTESIAN_POINT('Ctrl Pts',(-0.00307313757901286,-0.017526857790973,
-0.0112919022654047));
#17621=CARTESIAN_POINT('Ctrl Pts',(-0.00091723256157343,-0.0173677354937544,
-0.00911248448497608));
#17622=CARTESIAN_POINT('Ctrl Pts',(0.00208165523015107,-0.0172086131965359,
-0.00974845643188416));
#17623=CARTESIAN_POINT('Ctrl Pts',(0.00316739735457846,-0.0170494908993173,
-0.012615327958209));
#17624=CARTESIAN_POINT('Ctrl Pts',(0.00134214228753273,-0.0168903686020988,
-0.0150783001960814));
#17625=CARTESIAN_POINT('Ctrl Pts',(-0.00171660892348211,-0.0167312463048801,
-0.014873778006371));
#17626=CARTESIAN_POINT('Ctrl Pts',(-0.00319771035325614,-0.0165721240076617,
-0.0121897275436972));
#17627=CARTESIAN_POINT('Ctrl Pts',(-0.0017399554184275,-0.016413001710443,
-0.00949292594985999));
#17628=CARTESIAN_POINT('Ctrl Pts',(0.00131690588948234,-0.0162538794132246,
-0.00926186926186496));
#17629=CARTESIAN_POINT('Ctrl Pts',(0.00316346459286122,-0.016094757116006,
-0.0117089102212872));
#17630=CARTESIAN_POINT('Ctrl Pts',(0.0021026404634441,-0.0159356348187875,
-0.0145850952424985));
#17631=CARTESIAN_POINT('Ctrl Pts',(-0.000890615723146306,-0.0157765125215689,
-0.0152470660630366));
#17632=CARTESIAN_POINT('Ctrl Pts',(-0.00306535152975389,-0.0156173902243503,
-0.0130864379237458));
#17633=CARTESIAN_POINT('Ctrl Pts',(-0.00242287502126856,-0.0154582679271319,
-0.0100889372290884));
#17634=CARTESIAN_POINT('Ctrl Pts',(0.000446344565655069,-0.0152991456299132,
-0.00900941629679401));
#17635=CARTESIAN_POINT('Ctrl Pts',(0.00290535247923465,-0.0151400233326947,
-0.0108400116399476));
#17636=CARTESIAN_POINT('Ctrl Pts',(0.00269419286567144,-0.0149809010354761,
-0.0138983091682443));
#17637=CARTESIAN_POINT('Ctrl Pts',(6.94011231095411E-6,-0.0148217787382576,
-0.0153735898535058));
#17638=CARTESIAN_POINT('Ctrl Pts',(-0.00268670149544254,-0.0146626564410391,
-0.0139099771466985));
#17639=CARTESIAN_POINT('Ctrl Pts',(-0.0029111088345836,-0.0145035341438205,
-0.010852642967861));
#17640=CARTESIAN_POINT('Ctrl Pts',(-0.00046010166778407,-0.014344411846602,
-0.00901135558201923));
#17641=CARTESIAN_POINT('Ctrl Pts',(0.00241384190401448,-0.0141852895493834,
-0.0100784985125909));
#17642=CARTESIAN_POINT('Ctrl Pts',(0.00306918670385278,-0.0140261672521649,
-0.0130730232066427));
#17643=CARTESIAN_POINT('Ctrl Pts',(0.00090410295087455,-0.0138670449549463,
-0.0152433819291725));
#17644=CARTESIAN_POINT('Ctrl Pts',(-0.00209250213393695,-0.0137079226577278,
-0.014593784869784));
#17645=CARTESIAN_POINT('Ctrl Pts',(-0.00316480187508107,-0.0135488003605092,
-0.0117234475938452));
#17646=CARTESIAN_POINT('Ctrl Pts',(-0.00133085030856392,-0.0133896780632907,
-0.00926601323940937));
#17647=CARTESIAN_POINT('Ctrl Pts',(0.00173132963233982,-0.013230543634882,
-0.00948868242014083));
#17648=CARTESIAN_POINT('Ctrl Pts',(0.00270364229945445,-0.0131244499722128,
-0.0112753067108111));
#17649=CARTESIAN_POINT('Ctrl Pts',(0.00270341985263931,-0.0130713970752832,
-0.0121764714721861));
#17650=CARTESIAN_POINT('Ctrl Pts',(-0.00108503852354243,-0.0275018038640655,
-0.00990802990006322));
#17651=CARTESIAN_POINT('Ctrl Pts',(-0.000329170768612048,-0.027448757245193,
-0.00954637735452592));
#17652=CARTESIAN_POINT('Ctrl Pts',(0.00155964501320267,-0.027342669860581,
-0.0096452423055648));
#17653=CARTESIAN_POINT('Ctrl Pts',(0.00297513619154912,-0.0271835417102296,
-0.0121247078048999));
#17654=CARTESIAN_POINT('Ctrl Pts',(0.00164945534146205,-0.027024419413011,
-0.0146493225576553));
#17655=CARTESIAN_POINT('Ctrl Pts',(-0.00118879398834175,-0.0268652971157925,
-0.0149015192416286));
#17656=CARTESIAN_POINT('Ctrl Pts',(-0.00293618486755879,-0.0267061748185738,
-0.0126482790332008));
#17657=CARTESIAN_POINT('Ctrl Pts',(-0.00198420826837562,-0.0265470525213553,
-0.0099610655446497));
#17658=CARTESIAN_POINT('Ctrl Pts',(0.000790914408997691,-0.0263879302241368,
-0.00930924646984662));
#17659=CARTESIAN_POINT('Ctrl Pts',(0.00283937153658315,-0.0262288079269182,
-0.0112920373105569));
#17660=CARTESIAN_POINT('Ctrl Pts',(0.00227818936348208,-0.0260696856296996,
-0.0140870717435024));
#17661=CARTESIAN_POINT('Ctrl Pts',(-0.000376705013506482,-0.0259105633324811,
-0.0151256145447191));
#17662=CARTESIAN_POINT('Ctrl Pts',(-0.00268541820303118,-0.0257514410352626,
-0.0134531714832721));
#17663=CARTESIAN_POINT('Ctrl Pts',(-0.0025260821526076,-0.025592318738044,
-0.0106068125215213));
#17664=CARTESIAN_POINT('Ctrl Pts',(-4.51574619462108E-5,-0.0254331964408255,
-0.00920247893873924));
#17665=CARTESIAN_POINT('Ctrl Pts',(0.00247727311478055,-0.0252740741436069,
-0.0105308266088694));
#17666=CARTESIAN_POINT('Ctrl Pts',(0.00272296333398834,-0.0251149518463884,
-0.01337103590376));
#17667=CARTESIAN_POINT('Ctrl Pts',(0.000466114554639811,-0.0249558295491698,
-0.0151128126137062));
#17668=CARTESIAN_POINT('Ctrl Pts',(-0.00221911741836756,-0.0247967072519513,
-0.014155376124606));
#17669=CARTESIAN_POINT('Ctrl Pts',(-0.00286486880841401,-0.0246375849547327,
-0.0113786588273848));
#17670=CARTESIAN_POINT('Ctrl Pts',(-0.000877662064277731,-0.0244784626575142,
-0.0093346032295564));
#17671=CARTESIAN_POINT('Ctrl Pts',(0.00191616024882105,-0.0243193403602956,
-0.00990179909789713));
#17672=CARTESIAN_POINT('Ctrl Pts',(0.0029489350561568,-0.0241602180630771,
-0.0125589649279788));
#17673=CARTESIAN_POINT('Ctrl Pts',(0.00127149051084408,-0.0240010957658585,
-0.0148640319294356));
#17674=CARTESIAN_POINT('Ctrl Pts',(-0.00157451765915481,-0.02384197346864,
-0.0146985277936943));
#17675=CARTESIAN_POINT('Ctrl Pts',(-0.00297346504585819,-0.0236828511714214,
-0.0122145591340574));
#17676=CARTESIAN_POINT('Ctrl Pts',(-0.00163964877249473,-0.0235237288742029,
-0.00969501785674544));
#17677=CARTESIAN_POINT('Ctrl Pts',(0.0012010870438921,-0.0233646065769843,
-0.00945548889209919));
#17678=CARTESIAN_POINT('Ctrl Pts',(0.00293796356477596,-0.0232054842797658,
-0.0117161113839433));
#17679=CARTESIAN_POINT('Ctrl Pts',(0.00197470406706451,-0.0230463619825472,
-0.0143992597660848));
#17680=CARTESIAN_POINT('Ctrl Pts',(-0.00080340761007565,-0.0228872396853287,
-0.0150389859655547));
#17681=CARTESIAN_POINT('Ctrl Pts',(-0.00284314735773751,-0.0227281173881101,
-0.0130473494871182));
#17682=CARTESIAN_POINT('Ctrl Pts',(-0.00226989194113077,-0.0225689950908916,
-0.0102547642461744));
#17683=CARTESIAN_POINT('Ctrl Pts',(0.000389508131185215,-0.022409872793673,
-0.00922775628320164));
#17684=CARTESIAN_POINT('Ctrl Pts',(0.00269093067535579,-0.0222507504964545,
-0.0109101974779424));
#17685=CARTESIAN_POINT('Ctrl Pts',(0.00251925282849487,-0.0220916281992359,
-0.0137558399040919));
#17686=CARTESIAN_POINT('Ctrl Pts',(3.22551510868797E-5,-0.0219325059020174,
-0.0151493953042011));
#17687=CARTESIAN_POINT('Ctrl Pts',(-0.00248438662956492,-0.0217733836047988,
-0.0138101163009774));
#17688=CARTESIAN_POINT('Ctrl Pts',(-0.00271775236697587,-0.0216142613075803,
-0.0109688675379851));
#17689=CARTESIAN_POINT('Ctrl Pts',(-0.000453367232145684,-0.0214551390103618,
-0.00923689927564244));
#17690=CARTESIAN_POINT('Ctrl Pts',(0.00222768515070049,-0.0212960167131432,
-0.0102059773019314));
#17691=CARTESIAN_POINT('Ctrl Pts',(0.00286138303729019,-0.0211368944159246,
-0.012985470257334));
#17692=CARTESIAN_POINT('Ctrl Pts',(0.000865326254524445,-0.0209777721187061,
-0.0150208845691086));
#17693=CARTESIAN_POINT('Ctrl Pts',(-0.00192600880056463,-0.0208186498214876,
-0.0144415722950867));
#17694=CARTESIAN_POINT('Ctrl Pts',(-0.00294724507108097,-0.020659527524269,
-0.0117799504999432));
#17695=CARTESIAN_POINT('Ctrl Pts',(-0.00125981515241424,-0.0205004052270504,
-0.00948218324232324));
#17696=CARTESIAN_POINT('Ctrl Pts',(0.00158544814137571,-0.0203412829298319,
-0.00966003399327228));
#17697=CARTESIAN_POINT('Ctrl Pts',(0.00297360499451516,-0.0201821606326133,
-0.0121500489835251));
#17698=CARTESIAN_POINT('Ctrl Pts',(0.00162886956541392,-0.0200230383353948,
-0.0146637794237914));
#17699=CARTESIAN_POINT('Ctrl Pts',(-0.00121287877303721,-0.0198639160381762,
-0.0148909808355651));
#17700=CARTESIAN_POINT('Ctrl Pts',(-0.00293993062549207,-0.0197047937409577,
-0.0126228437145923));
#17701=CARTESIAN_POINT('Ctrl Pts',(-0.00196503863148784,-0.0195456714437391,
-0.00994389994873465));
#17702=CARTESIAN_POINT('Ctrl Pts',(0.00081582252123233,-0.0193865491465206,
-0.00931623335738731));
#17703=CARTESIAN_POINT('Ctrl Pts',(0.00284690181790013,-0.0192274268493021,
-0.0113167010505152));
#17704=CARTESIAN_POINT('Ctrl Pts',(0.00226153541287361,-0.0190683045520835,
-0.0141067727830104));
#17705=CARTESIAN_POINT('Ctrl Pts',(-0.000402295578827005,-0.018909182254865,
-0.0151222325548662));
#17706=CARTESIAN_POINT('Ctrl Pts',(-0.00269639673600516,-0.0187500599576464,
-0.013429821853756));
#17707=CARTESIAN_POINT('Ctrl Pts',(-0.00251237391798254,-0.0185909376604278,
-0.0105849510828679));
#17708=CARTESIAN_POINT('Ctrl Pts',(-1.93533335359779E-5,-0.0184318153632094,
-0.00920219930972517));
#17709=CARTESIAN_POINT('Ctrl Pts',(0.00249145393607667,-0.0182726930659907,
-0.010552384836028));
#17710=CARTESIAN_POINT('Ctrl Pts',(0.00271248995295037,-0.0181135707687723,
-0.0133946193759434));
#17711=CARTESIAN_POINT('Ctrl Pts',(0.000440611520263108,-0.0179544484715537,
-0.0151167466905447));
#17712=CARTESIAN_POINT('Ctrl Pts',(-0.00223621102078284,-0.0177953261743351,
-0.0141360453169456));
#17713=CARTESIAN_POINT('Ctrl Pts',(-0.0028578433629701,-0.0176362038771165,
-0.0113538290543058));
#17714=CARTESIAN_POINT('Ctrl Pts',(-0.000852974174112536,-0.017477081579898,
-0.00932709433163266));
#17715=CARTESIAN_POINT('Ctrl Pts',(0.00193582110482348,-0.0173179592826795,
-0.00991851211257368));
#17716=CARTESIAN_POINT('Ctrl Pts',(0.00294549959933089,-0.0171588369854609,
-0.0125845397645564));
#17717=CARTESIAN_POINT('Ctrl Pts',(0.0012481160800549,-0.0169997146882424,
-0.0148749640238712));
#17718=CARTESIAN_POINT('Ctrl Pts',(-0.00159634877796926,-0.0168405923910238,
-0.0146847700063838));
#17719=CARTESIAN_POINT('Ctrl Pts',(-0.00297368896601409,-0.0166814700938053,
-0.0121887555574983));
#17720=CARTESIAN_POINT('Ctrl Pts',(-0.0016180596919498,-0.0165223477965867,
-0.00968088328102499));
#17721=CARTESIAN_POINT('Ctrl Pts',(0.00122464766355246,-0.0163632254993682,
-0.00946601368756258));
#17722=CARTESIAN_POINT('Ctrl Pts',(0.00294184235435476,-0.0162041032021496,
-0.0117416227629777));
#17723=CARTESIAN_POINT('Ctrl Pts',(0.00195533617961103,-0.016044980904931,
-0.0144163114361035));
#17724=CARTESIAN_POINT('Ctrl Pts',(-0.000828222026482802,-0.0158858586077125,
-0.0150319066925196));
#17725=CARTESIAN_POINT('Ctrl Pts',(-0.00285060277948614,-0.015726736310494,
-0.0130226452686618));
#17726=CARTESIAN_POINT('Ctrl Pts',(-0.00225313612580357,-0.0155676140132754,
-0.0102351399111969));
#17727=CARTESIAN_POINT('Ctrl Pts',(0.000415075089142231,-0.0154084917160569,
-0.00923124677194611));
#17728=CARTESIAN_POINT('Ctrl Pts',(0.00270181275207879,-0.0152493694188383,
-0.0109335964446202));
#17729=CARTESIAN_POINT('Ctrl Pts',(0.00250544630748153,-0.0150902471216198,
-0.0137776394034903));
#17730=CARTESIAN_POINT('Ctrl Pts',(6.45391018013059E-6,-0.0149311248244012,
-0.0151495666298162));
#17731=CARTESIAN_POINT('Ctrl Pts',(-0.00249847975875477,-0.0147720025271827,
-0.0137884899605927));
#17732=CARTESIAN_POINT('Ctrl Pts',(-0.0027071658355337,-0.0146128802299641,
-0.0109453428619918));
#17733=CARTESIAN_POINT('Ctrl Pts',(-0.0004278684125787,-0.0144537579327456,
-0.00923305019703428));
#17734=CARTESIAN_POINT('Ctrl Pts',(0.00224473583993033,-0.014294635635527,
-0.0102254324978796));
#17735=CARTESIAN_POINT('Ctrl Pts',(0.00285416927352115,-0.0141355133383085,
-0.0130101703438483));
#17736=CARTESIAN_POINT('Ctrl Pts',(0.000840764382058176,-0.0139763910410899,
-0.0150284806573225));
#17737=CARTESIAN_POINT('Ctrl Pts',(-0.00194590810912974,-0.0138172687438714,
-0.0144243922958196));
#17738=CARTESIAN_POINT('Ctrl Pts',(-0.00294308595084797,-0.0136581464466527,
-0.0117551416935859));
#17739=CARTESIAN_POINT('Ctrl Pts',(-0.0012376151811133,-0.0134990241494343,
-0.00946986735125886));
#17740=CARTESIAN_POINT('Ctrl Pts',(0.00161003820092075,-0.0133398897210256,
-0.00967693703946193));
#17741=CARTESIAN_POINT('Ctrl Pts',(0.00251423374407564,-0.0132337960583565,
-0.0113383961313303));
#17742=CARTESIAN_POINT('Ctrl Pts',(0.00251402688117483,-0.0131807431614265,
-0.0121764281640729));
#17743=CARTESIAN_POINT('Ctrl Pts',(-0.00132619774418405,-0.0271787743898765,
-0.0094032008032357));
#17744=CARTESIAN_POINT('Ctrl Pts',(-0.00123334707548279,-0.0271787743898774,
-0.00936860122999075));
#17745=CARTESIAN_POINT('Ctrl Pts',(-0.00113896878046653,-0.0271787743898777,
-0.00933897076543453));
#17746=CARTESIAN_POINT('Ctrl Pts',(-0.00104343428160282,-0.0271787743898779,
-0.0093141943241909));
#17747=CARTESIAN_POINT('Ctrl Pts',(-0.00076805930112476,-0.0271787743898785,
-0.00924277706545265));
#17748=CARTESIAN_POINT('Ctrl Pts',(-0.000483025747473507,-0.027178774389879,
-0.00921146057988075));
#17749=CARTESIAN_POINT('Ctrl Pts',(-0.000197232514694447,-0.0271787743898794,
-0.00921970998708291));
#17750=CARTESIAN_POINT('Ctrl Pts',(-0.000179613012251587,-0.0271787743898794,
-0.00922021857312932));
#17751=CARTESIAN_POINT('Ctrl Pts',(-0.000161988828498365,-0.0271787743898794,
-0.00922087869898021));
#17752=CARTESIAN_POINT('Ctrl Pts',(-0.000144384552395993,-0.0271787743898794,
-0.00922168930787544));
#17753=CARTESIAN_POINT('Ctrl Pts',(-4.51942574374791E-5,-0.0271787743898796,
-0.0092262566377075));
#17754=CARTESIAN_POINT('Ctrl Pts',(5.35197260388724E-5,-0.0271787743898787,
-0.00923560020302817));
#17755=CARTESIAN_POINT('Ctrl Pts',(0.000151386361355854,-0.0271787743898786,
-0.0092496540195405));
#17756=CARTESIAN_POINT('Ctrl Pts',(0.000344058415070921,-0.0271787743898783,
-0.00927732205657064));
#17757=CARTESIAN_POINT('Ctrl Pts',(0.000533476473635147,-0.027178774389878,
-0.00932320440058446));
#17758=CARTESIAN_POINT('Ctrl Pts',(0.000716581926211375,-0.0271787743898776,
-0.00938734742840202));
#17759=CARTESIAN_POINT('Ctrl Pts',(0.0007556805873622,-0.0271787743898775,
-0.00940104394303083));
#17760=CARTESIAN_POINT('Ctrl Pts',(0.000794489703590543,-0.0271787743898774,
-0.00941557553850965));
#17761=CARTESIAN_POINT('Ctrl Pts',(0.000832976258181437,-0.0271787743898773,
-0.00943094658771291));
#17762=CARTESIAN_POINT('Ctrl Pts',(0.000855095263786809,-0.0271787743898773,
-0.00943978064228344));
#17763=CARTESIAN_POINT('Ctrl Pts',(0.00087710770065419,-0.0271787743898772,
-0.00944889199559381));
#17764=CARTESIAN_POINT('Ctrl Pts',(0.000899007079087444,-0.0271787743898772,
-0.00945828167060659));
#17765=CARTESIAN_POINT('Ctrl Pts',(0.000915403294136593,-0.0271787743898772,
-0.00946531178478176));
#17766=CARTESIAN_POINT('Ctrl Pts',(0.000931738600316675,-0.0271787743898771,
-0.00947249914463924));
#17767=CARTESIAN_POINT('Ctrl Pts',(0.000947988260384964,-0.0271787743898771,
-0.00947983398932806));
#17768=CARTESIAN_POINT('Ctrl Pts',(0.00111836097776595,-0.0271787743898767,
-0.00955673759321582));
#17769=CARTESIAN_POINT('Ctrl Pts',(0.00127987164207508,-0.0271787743898763,
-0.00965001320728162));
#17770=CARTESIAN_POINT('Ctrl Pts',(0.00142972751227199,-0.0271787743898758,
-0.00975968542682677));
#17771=CARTESIAN_POINT('Ctrl Pts',(0.0014442192240037,-0.0271787743898758,
-0.00977029120548955));
#17772=CARTESIAN_POINT('Ctrl Pts',(0.00145860151389945,-0.0271787743898758,
-0.00978105080560855));
#17773=CARTESIAN_POINT('Ctrl Pts',(0.00147287155736277,-0.0271787743898757,
-0.00979196455368879));
#17774=CARTESIAN_POINT('Ctrl Pts',(0.00154855896912941,-0.0271787743898755,
-0.00984985038613137));
#17775=CARTESIAN_POINT('Ctrl Pts',(0.00162109245549692,-0.0271787743898753,
-0.00991207085484757));
#17776=CARTESIAN_POINT('Ctrl Pts',(0.00169026613585085,-0.0271787743898751,
-0.00997826337560861));
#17777=CARTESIAN_POINT('Ctrl Pts',(0.00171603724734808,-0.027178774389875,
-0.0100029238364094));
#17778=CARTESIAN_POINT('Ctrl Pts',(0.00174134154940518,-0.0271787743898749,
-0.0100281358260087));
#17779=CARTESIAN_POINT('Ctrl Pts',(0.00176616664819554,-0.0271787743898748,
-0.0100538811973334));
#17780=CARTESIAN_POINT('Ctrl Pts',(0.00177607355662899,-0.0271787743898748,
-0.0100641553573057));
#17781=CARTESIAN_POINT('Ctrl Pts',(0.00178590413828819,-0.0271787743898747,
-0.01007451446367));
#17782=CARTESIAN_POINT('Ctrl Pts',(0.00179565756092862,-0.0271787743898747,
-0.0100849573712734));
#17783=CARTESIAN_POINT('Ctrl Pts',(0.00180578442604608,-0.0271787743898747,
-0.0100958001205966));
#17784=CARTESIAN_POINT('Ctrl Pts',(0.00181582268481298,-0.0271787743898746,
-0.0101067274469139));
#17785=CARTESIAN_POINT('Ctrl Pts',(0.00182576793439398,-0.0271787743898746,
-0.0101177335422781));
#17786=CARTESIAN_POINT('Ctrl Pts',(0.00201260976483294,-0.027178774389874,
-0.0103245055279476));
#17787=CARTESIAN_POINT('Ctrl Pts',(0.00216737989308834,-0.0271787743898734,
-0.0105594160048695));
#17788=CARTESIAN_POINT('Ctrl Pts',(0.00228510901854104,-0.0271787743898728,
-0.0108129813847881));
#17789=CARTESIAN_POINT('Ctrl Pts',(0.00230305828244781,-0.0271787743898727,
-0.0108516405687774));
#17790=CARTESIAN_POINT('Ctrl Pts',(0.00232013895398843,-0.0271787743898726,
-0.010890735204995));
#17791=CARTESIAN_POINT('Ctrl Pts',(0.00233632486912502,-0.0271787743898725,
-0.0109302325471785));
#17792=CARTESIAN_POINT('Ctrl Pts',(0.00234257114675687,-0.0271787743898725,
-0.0109454748960304));
#17793=CARTESIAN_POINT('Ctrl Pts',(0.0023486848303271,-0.0271787743898725,
-0.0109607789757957));
#17794=CARTESIAN_POINT('Ctrl Pts',(0.00235466215265408,-0.0271787743898725,
-0.0109761373101646));
#17795=CARTESIAN_POINT('Ctrl Pts',(0.00242919330983191,-0.027178774389872,
-0.011167640188915));
#17796=CARTESIAN_POINT('Ctrl Pts',(0.0024822151522778,-0.0271787743898716,
-0.01136648020721));
#17797=CARTESIAN_POINT('Ctrl Pts',(0.00251112044339404,-0.0271787743898712,
-0.0115688122023905));
#17798=CARTESIAN_POINT('Ctrl Pts',(0.00251367237767708,-0.0271787743898712,
-0.0115866752971776));
#17799=CARTESIAN_POINT('Ctrl Pts',(0.00251603423918924,-0.0271787743898712,
-0.0116045574678031));
#17800=CARTESIAN_POINT('Ctrl Pts',(0.00251820375128431,-0.0271787743898711,
-0.0116224513576578));
#17801=CARTESIAN_POINT('Ctrl Pts',(0.00253875013258885,-0.0271787743898708,
-0.0117919155818088));
#17802=CARTESIAN_POINT('Ctrl Pts',(0.00254212787993046,-0.0271787743898705,
-0.011962581473446));
#17803=CARTESIAN_POINT('Ctrl Pts',(0.00252655408384864,-0.0271787743898702,
-0.0121321046600801));
#17804=CARTESIAN_POINT('Ctrl Pts',(0.00252521873542723,-0.0271787743898702,
-0.0121466401348273));
#17805=CARTESIAN_POINT('Ctrl Pts',(0.00252374357338409,-0.0271787743898702,
-0.0121611670509537));
#17806=CARTESIAN_POINT('Ctrl Pts',(0.00252212942997833,-0.0271787743898701,
-0.0121756837992191));
#17807=CARTESIAN_POINT('Origin',(0.,-0.00867877438987209,-0.012175853286558));
#17808=CARTESIAN_POINT('',(-0.0023,-0.00867877438987209,-0.012175853286558));
#17809=CARTESIAN_POINT('Origin',(0.,-0.0261787743898721,-0.0121758532865581));
#17810=CARTESIAN_POINT('',(-0.01115,-0.0261787743898724,-0.0121758532865581));
#17811=CARTESIAN_POINT('Origin',(0.,-0.0261787743898824,-0.0121758532865681));
#17812=CARTESIAN_POINT('',(0.00601982559920929,-0.0261787743898934,-0.012175853286558));
#17813=CARTESIAN_POINT('Origin',(0.,-0.0261787743898824,-0.0121758532865681));
#17814=CARTESIAN_POINT('Origin',(0.,-0.0236787743898721,-0.0121758532865581));
#17815=CARTESIAN_POINT('',(-0.01115,-0.0236787743898724,-0.0121758532865581));
#17816=CARTESIAN_POINT('Origin',(0.,-0.0236787743898824,-0.0121758532865681));
#17817=CARTESIAN_POINT('',(0.00588880615100169,-0.0236787743898934,-0.012175853286558));
#17818=CARTESIAN_POINT('Origin',(0.,-0.0236787743898824,-0.0121758532865681));
#17819=CARTESIAN_POINT('Origin',(0.,-0.0246787743898721,-0.0121758532865581));
#17820=CARTESIAN_POINT('',(-0.01115,-0.0246787743898924,-0.0121758532865581));
#17821=CARTESIAN_POINT('Origin',(0.,-0.0246787743898824,-0.0121758532865681));
#17822=CARTESIAN_POINT('',(0.00594121393028363,-0.0246787743898724,-0.012175853286558));
#17823=CARTESIAN_POINT('Origin',(0.,-0.0246787743898824,-0.0121758532865681));
#17824=CARTESIAN_POINT('Origin',(0.,-0.0211787743898721,-0.012175853286558));
#17825=CARTESIAN_POINT('',(-0.01115,-0.0211787743898724,-0.0121758532865581));
#17826=CARTESIAN_POINT('Origin',(0.,-0.0211787743898824,-0.012175853286568));
#17827=CARTESIAN_POINT('',(0.00575778670279409,-0.0211787743898934,-0.012175853286558));
#17828=CARTESIAN_POINT('Origin',(0.,-0.0211787743898824,-0.012175853286568));
#17829=CARTESIAN_POINT('Origin',(0.,-0.0221787743898721,-0.0121758532865581));
#17830=CARTESIAN_POINT('',(-0.01115,-0.0221787743898924,-0.0121758532865581));
#17831=CARTESIAN_POINT('Origin',(0.,-0.0221787743898824,-0.0121758532865681));
#17832=CARTESIAN_POINT('',(0.00581019448207603,-0.0221787743898724,-0.012175853286558));
#17833=CARTESIAN_POINT('Origin',(0.,-0.0221787743898824,-0.0121758532865681));
#17834=CARTESIAN_POINT('Origin',(0.,-0.0186787743898721,-0.012175853286558));
#17835=CARTESIAN_POINT('',(-0.01115,-0.0186787743898724,-0.012175853286558));
#17836=CARTESIAN_POINT('Origin',(0.,-0.0186787743898824,-0.012175853286568));
#17837=CARTESIAN_POINT('',(0.00562676725458648,-0.0186787743898934,-0.012175853286558));
#17838=CARTESIAN_POINT('Origin',(0.,-0.0186787743898824,-0.012175853286568));
#17839=CARTESIAN_POINT('Origin',(0.,-0.0196787743898721,-0.012175853286558));
#17840=CARTESIAN_POINT('',(-0.01115,-0.0196787743898924,-0.012175853286558));
#17841=CARTESIAN_POINT('Origin',(0.,-0.0196787743898824,-0.012175853286568));
#17842=CARTESIAN_POINT('',(0.00567917503386843,-0.0196787743898724,-0.012175853286558));
#17843=CARTESIAN_POINT('Origin',(0.,-0.0196787743898824,-0.012175853286568));
#17844=CARTESIAN_POINT('Origin',(0.,-0.0161787743898721,-0.012175853286558));
#17845=CARTESIAN_POINT('',(-0.01115,-0.0161787743898724,-0.012175853286558));
#17846=CARTESIAN_POINT('Origin',(0.,-0.0161787743898824,-0.012175853286568));
#17847=CARTESIAN_POINT('',(0.00549574780637888,-0.0161787743898934,-0.012175853286558));
#17848=CARTESIAN_POINT('Origin',(0.,-0.0161787743898824,-0.012175853286568));
#17849=CARTESIAN_POINT('Origin',(0.,-0.0171787743898721,-0.012175853286558));
#17850=CARTESIAN_POINT('',(-0.01115,-0.0171787743898924,-0.012175853286558));
#17851=CARTESIAN_POINT('Origin',(0.,-0.0171787743898824,-0.012175853286568));
#17852=CARTESIAN_POINT('',(0.00554815558566082,-0.0171787743898724,-0.012175853286558));
#17853=CARTESIAN_POINT('Origin',(0.,-0.0171787743898824,-0.012175853286568));
#17854=CARTESIAN_POINT('Origin',(0.,-0.0136787743898721,-0.012175853286558));
#17855=CARTESIAN_POINT('',(-0.01115,-0.0136787743898724,-0.012175853286558));
#17856=CARTESIAN_POINT('Origin',(0.,-0.0136787743898824,-0.012175853286568));
#17857=CARTESIAN_POINT('',(0.00536472835817128,-0.0136787743898934,-0.012175853286558));
#17858=CARTESIAN_POINT('Origin',(0.,-0.0136787743898824,-0.012175853286568));
#17859=CARTESIAN_POINT('Origin',(0.,-0.0146787743898721,-0.012175853286558));
#17860=CARTESIAN_POINT('',(-0.01115,-0.0146787743898924,-0.012175853286558));
#17861=CARTESIAN_POINT('Origin',(0.,-0.0146787743898824,-0.012175853286568));
#17862=CARTESIAN_POINT('',(0.00541713613745322,-0.0146787743898724,-0.012175853286558));
#17863=CARTESIAN_POINT('Origin',(0.,-0.0146787743898824,-0.012175853286568));
#17864=CARTESIAN_POINT('Origin',(0.,-0.0111787743898721,-0.012175853286558));
#17865=CARTESIAN_POINT('',(0.01115,-0.0111787743898724,-0.012175853286558));
#17866=CARTESIAN_POINT('Origin',(0.,-0.0111787743898824,-0.012175853286568));
#17867=CARTESIAN_POINT('',(0.00523370890996368,-0.0111787743898934,-0.012175853286558));
#17868=CARTESIAN_POINT('Origin',(0.,-0.0111787743898824,-0.012175853286568));
#17869=CARTESIAN_POINT('Origin',(0.,-0.0121787743898721,-0.012175853286558));
#17870=CARTESIAN_POINT('',(0.01115,-0.0121787743898924,-0.012175853286558));
#17871=CARTESIAN_POINT('Origin',(0.,-0.0121787743898824,-0.012175853286568));
#17872=CARTESIAN_POINT('',(0.00528611668924562,-0.0121787743898724,-0.012175853286558));
#17873=CARTESIAN_POINT('Origin',(0.,-0.0121787743898824,-0.012175853286568));
#17874=CARTESIAN_POINT('Origin',(0.,-0.00967877438987209,-0.012175853286558));
#17875=CARTESIAN_POINT('',(0.01115,-0.00967877438989238,-0.012175853286558));
#17876=CARTESIAN_POINT('Origin',(0.,-0.00967877438988238,-0.012175853286568));
#17877=CARTESIAN_POINT('',(0.00515509724103801,-0.00967877438987238,-0.012175853286558));
#17878=CARTESIAN_POINT('Origin',(0.,-0.00967877438988238,-0.012175853286568));
#17879=CARTESIAN_POINT('Origin',(0.,-0.00867877438987209,-0.012175853286558));
#17880=CARTESIAN_POINT('',(0.01115,-0.00867877438987238,-0.012175853286558));
#17881=CARTESIAN_POINT('Origin',(0.,-0.00867877438988238,-0.012175853286568));
#17882=CARTESIAN_POINT('',(0.00510268946175607,-0.00867877438989337,-0.012175853286558));
#17883=CARTESIAN_POINT('Origin',(0.,-0.00867877438988238,-0.012175853286568));
#17884=CARTESIAN_POINT('Origin',(0.,-0.0266787743898721,-0.0121758532865581));
#17885=CARTESIAN_POINT('',(-0.01115,-0.0271787743898924,-0.0121758532865581));
#17886=CARTESIAN_POINT('Origin',(0.,-0.0271787743898824,-0.0121758532865681));
#17887=CARTESIAN_POINT('',(-0.01115,-0.0266787743898721,-0.0121758532865581));
#17888=CARTESIAN_POINT('Origin',(0.,-0.0241787743898721,-0.0121758532865581));
#17889=CARTESIAN_POINT('',(-0.01115,-0.0241787743898721,-0.0121758532865581));
#17890=CARTESIAN_POINT('Origin',(0.,-0.0216787743898721,-0.0121758532865581));
#17891=CARTESIAN_POINT('',(-0.01115,-0.0216787743898721,-0.0121758532865581));
#17892=CARTESIAN_POINT('Origin',(0.,-0.0191787743898721,-0.012175853286558));
#17893=CARTESIAN_POINT('',(-0.01115,-0.0191787743898721,-0.012175853286558));
#17894=CARTESIAN_POINT('Origin',(0.,-0.0166787743898721,-0.012175853286558));
#17895=CARTESIAN_POINT('',(-0.01115,-0.0166787743898721,-0.012175853286558));
#17896=CARTESIAN_POINT('Origin',(0.,-0.0141787743898721,-0.012175853286558));
#17897=CARTESIAN_POINT('',(-0.01115,-0.0141787743898721,-0.012175853286558));
#17898=CARTESIAN_POINT('Origin',(0.,-0.0111787743898721,-0.012175853286558));
#17899=CARTESIAN_POINT('',(0.01115,-0.0111787743898721,-0.012175853286558));
#17900=CARTESIAN_POINT('Origin',(0.,-0.00867877438987209,-0.012175853286558));
#17901=CARTESIAN_POINT('',(0.01115,-0.00867877438987209,-0.012175853286558));
#17902=CARTESIAN_POINT('Origin',(0.,0.00282122561012762,-0.012175853286558));
#17903=CARTESIAN_POINT('',(0.00502407779283041,-0.00717877438987238,-0.012175853286558));
#17904=CARTESIAN_POINT('',(0.0045,0.00282122561012762,-0.012175853286558));
#17905=CARTESIAN_POINT('Origin',(0.,-0.00717877438988238,-0.012175853286568));
#17906=CARTESIAN_POINT('Origin',(0.,0.00282122561012762,-0.012175853286558));
#17907=CARTESIAN_POINT('',(0.0045,0.00282122561012762,-0.012175853286558));
#17908=CARTESIAN_POINT('Origin',(0.,0.00282122561012762,-0.012175853286558));
#17909=CARTESIAN_POINT('',(0.0045,0.00282122561012762,-0.012175853286558));
#17910=CARTESIAN_POINT('Origin',(0.,0.00282122561012762,-0.012175853286558));
#17911=CARTESIAN_POINT('',(0.0045,0.00282122561012762,-0.012175853286558));
#17912=CARTESIAN_POINT('Origin',(0.,0.00282122561012762,-0.012175853286558));
#17913=CARTESIAN_POINT('',(0.0045,0.00282122561012762,-0.012175853286558));
#17914=CARTESIAN_POINT('Origin',(0.,0.00282122561012762,-0.012175853286558));
#17915=CARTESIAN_POINT('',(0.0045,0.00282122561012762,-0.012175853286558));
#17916=CARTESIAN_POINT('Origin',(0.,0.00282122561012762,-0.012175853286558));
#17917=CARTESIAN_POINT('',(0.0045,0.00282122561012762,-0.012175853286558));
#17918=CARTESIAN_POINT('Origin',(0.,-0.0271787743898721,-0.0121758532865581));
#17919=CARTESIAN_POINT('Origin',(0.,0.00282122561012762,-0.012175853286558));
#17920=CARTESIAN_POINT('',(0.00470963111713326,-0.00117877438989337,-0.012175853286558));
#17921=CARTESIAN_POINT('Origin',(0.,-0.00117877438988238,-0.012175853286568));
#17922=CARTESIAN_POINT('',(0.0046310194482076,0.000321225610127617,-0.012175853286558));
#17923=CARTESIAN_POINT('',(0.0045,0.00282122561012762,-0.012175853286558));
#17924=CARTESIAN_POINT('Origin',(0.,0.000321225610117618,-0.012175853286568));
#17925=CARTESIAN_POINT('Origin',(0.,0.00282122561012762,-0.012175853286558));
#17926=CARTESIAN_POINT('',(0.00457861166892566,0.00132122561010662,-0.012175853286558));
#17927=CARTESIAN_POINT('Origin',(0.,0.00132122561011761,-0.012175853286568));
#17928=CARTESIAN_POINT('',(0.0045,0.00282122561012761,-0.012175853286558));
#17929=CARTESIAN_POINT('',(0.0045,0.00282122561012762,-0.012175853286558));
#17930=CARTESIAN_POINT('Origin',(0.,0.00282122561011761,-0.012175853286568));
#17931=CARTESIAN_POINT('Origin',(0.,0.00282122561012762,-0.012175853286558));
#17932=CARTESIAN_POINT('',(0.00484065056534087,-0.00367877438989337,-0.012175853286558));
#17933=CARTESIAN_POINT('Origin',(0.,-0.00367877438988238,-0.012175853286568));
#17934=CARTESIAN_POINT('',(0.0047620388964152,-0.00217877438987238,-0.012175853286558));
#17935=CARTESIAN_POINT('',(0.0045,0.00282122561012762,-0.012175853286558));
#17936=CARTESIAN_POINT('Origin',(0.,-0.00217877438988238,-0.012175853286568));
#17937=CARTESIAN_POINT('Origin',(0.,0.00282122561012762,-0.012175853286558));
#17938=CARTESIAN_POINT('',(0.00497167001354847,-0.00617877438989337,-0.012175853286558));
#17939=CARTESIAN_POINT('Origin',(0.,-0.00617877438988238,-0.012175853286568));
#17940=CARTESIAN_POINT('',(0.00489305834462281,-0.00467877438987239,-0.012175853286558));
#17941=CARTESIAN_POINT('',(0.0045,0.00282122561012762,-0.012175853286558));
#17942=CARTESIAN_POINT('Origin',(0.,-0.00467877438988239,-0.012175853286568));
#17943=CARTESIAN_POINT('Origin',(0.,0.00282122561012762,-0.012175853286558));
#17944=CARTESIAN_POINT('',(0.0045,0.00282122561012762,-0.012175853286558));
#17945=CARTESIAN_POINT('Origin',(0.,-0.00617877438987208,-0.012175853286558));
#17946=CARTESIAN_POINT('',(0.01115,-0.00617877438987238,-0.012175853286558));
#17947=CARTESIAN_POINT('Origin',(0.,-0.00617877438988238,-0.012175853286568));
#17948=CARTESIAN_POINT('Origin',(0.,-0.00617877438987208,-0.012175853286558));
#17949=CARTESIAN_POINT('',(0.01115,-0.00717877438989238,-0.012175853286558));
#17950=CARTESIAN_POINT('Origin',(0.,-0.00717877438988238,-0.012175853286568));
#17951=CARTESIAN_POINT('',(0.01115,-0.00617877438987208,-0.012175853286558));
#17952=CARTESIAN_POINT('Origin',(0.,-0.00717877438987209,-0.012175853286558));
#17953=CARTESIAN_POINT('Origin',(0.,-0.00367877438987208,-0.012175853286558));
#17954=CARTESIAN_POINT('',(0.01115,-0.00367877438987238,-0.012175853286558));
#17955=CARTESIAN_POINT('Origin',(0.,-0.00367877438988238,-0.012175853286568));
#17956=CARTESIAN_POINT('Origin',(0.,-0.00367877438987208,-0.012175853286558));
#17957=CARTESIAN_POINT('',(0.01115,-0.00467877438989239,-0.012175853286558));
#17958=CARTESIAN_POINT('Origin',(0.,-0.00467877438988239,-0.012175853286568));
#17959=CARTESIAN_POINT('',(0.01115,-0.00367877438987208,-0.012175853286558));
#17960=CARTESIAN_POINT('Origin',(0.,-0.00467877438987209,-0.012175853286558));
#17961=CARTESIAN_POINT('Origin',(0.,-0.00117877438987208,-0.012175853286558));
#17962=CARTESIAN_POINT('',(0.01115,-0.00117877438987238,-0.012175853286558));
#17963=CARTESIAN_POINT('Origin',(0.,-0.00117877438988238,-0.012175853286568));
#17964=CARTESIAN_POINT('Origin',(0.,-0.00117877438987208,-0.012175853286558));
#17965=CARTESIAN_POINT('',(0.01115,-0.00217877438989238,-0.012175853286558));
#17966=CARTESIAN_POINT('Origin',(0.,-0.00217877438988238,-0.012175853286568));
#17967=CARTESIAN_POINT('',(0.01115,-0.00117877438987208,-0.012175853286558));
#17968=CARTESIAN_POINT('Origin',(0.,-0.00217877438987208,-0.012175853286558));
#17969=CARTESIAN_POINT('Origin',(0.,0.00132122561012792,-0.012175853286558));
#17970=CARTESIAN_POINT('',(0.008,0.00132122561012761,-0.012175853286558));
#17971=CARTESIAN_POINT('Origin',(0.,0.00132122561011761,-0.012175853286568));
#17972=CARTESIAN_POINT('Origin',(0.,0.00132122561012792,-0.012175853286558));
#17973=CARTESIAN_POINT('',(0.008,0.000321225610107618,-0.012175853286558));
#17974=CARTESIAN_POINT('Origin',(0.,0.000321225610117618,-0.012175853286568));
#17975=CARTESIAN_POINT('',(0.008,0.00132122561012792,-0.012175853286558));
#17976=CARTESIAN_POINT('Origin',(0.,0.000321225610127919,-0.012175853286558));
#17977=CARTESIAN_POINT('Origin',(0.,0.00582122561012762,-0.012175853286558));
#17978=CARTESIAN_POINT('',(0.008,0.00582122561012762,-0.012175853286558));
#17979=CARTESIAN_POINT('Origin',(0.,0.00582122561011762,-0.012175853286568));
#17980=CARTESIAN_POINT('',(0.006,0.00582122561010762,-0.012175853286558));
#17981=CARTESIAN_POINT('Origin',(0.,0.00582122561011762,-0.012175853286568));
#17982=CARTESIAN_POINT('Origin',(0.,0.00582122561012762,-0.012175853286558));
#17983=CARTESIAN_POINT('',(0.008,0.00282122561010761,-0.012175853286558));
#17984=CARTESIAN_POINT('Origin',(0.,0.00282122561011761,-0.012175853286568));
#17985=CARTESIAN_POINT('',(0.008,0.00582122561012762,-0.012175853286558));
#17986=CARTESIAN_POINT('Origin',(0.,0.00282122561012762,-0.012175853286558));
#17987=CARTESIAN_POINT('Origin',(0.,0.0118212256101276,-0.012175853286558));
#17988=CARTESIAN_POINT('',(0.006,0.0118212256101276,-0.012175853286558));
#17989=CARTESIAN_POINT('',(0.,0.,0.));
#17990=CARTESIAN_POINT('Origin',(0.00210744426613017,0.0161212256101277,
-0.00934021046660988));
#17991=CARTESIAN_POINT('',(0.00175,0.0163712256101277,-0.00996121046660988));
#17992=CARTESIAN_POINT('',(0.00175,0.0158712256101277,-0.00871921046660988));
#17993=CARTESIAN_POINT('',(0.00175000000001,0.0162735607568884,-0.00971861097112858));
#17994=CARTESIAN_POINT('',(0.00175135530812579,0.0158712256101277,-0.00871921046660988));
#17995=CARTESIAN_POINT('',(0.00210744426614017,0.0158712256101377,-0.00871921046659988));
#17996=CARTESIAN_POINT('',(0.00317977706452068,0.0163712256101277,-0.00996121046660988));
#17997=CARTESIAN_POINT('Origin',(0.,0.017262788742162,-0.0121758532865581));
#17998=CARTESIAN_POINT('',(0.00087500000001,0.0163712256101377,-0.00996121046659988));
#17999=CARTESIAN_POINT('Origin',(0.00246488853226034,0.0158712256101277,
-0.00933986729084157));
#18000=CARTESIAN_POINT('',(0.00175,0.0158712256101277,-0.00871852411507327));
#18001=CARTESIAN_POINT('',(0.00175000000001,0.0158712256101377,-0.00990053887871572));
#18002=CARTESIAN_POINT('Origin',(0.,0.0158712256101377,-0.0121758532865581));
#18003=CARTESIAN_POINT('Origin',(-0.00282233279839051,0.0161212256101277,
-0.00934021046660988));
#18004=CARTESIAN_POINT('',(-0.00317977706452068,0.0163712256101277,-0.00996121046660988));
#18005=CARTESIAN_POINT('',(-0.00175135530812579,0.0158712256101277,-0.00871921046660988));
#18006=CARTESIAN_POINT('Origin',(0.,0.017262788742162,-0.0121758532865581));
#18007=CARTESIAN_POINT('',(-0.00175,0.0158712256101277,-0.00871921046660988));
#18008=CARTESIAN_POINT('',(-0.00282233279840051,0.0158712256101377,-0.00871921046659988));
#18009=CARTESIAN_POINT('',(-0.00175,0.0163712256101277,-0.00996121046660988));
#18010=CARTESIAN_POINT('',(-0.00175000000001,0.0159717003423357,-0.00896878970137986));
#18011=CARTESIAN_POINT('',(-0.00158988853227034,0.0163712256101377,-0.00996121046659988));
#18012=CARTESIAN_POINT('Origin',(-0.00246488853226034,0.0158712256101277,
-0.00933986729084157));
#18013=CARTESIAN_POINT('',(-0.00175,0.0158712256101277,-0.00871852411507327));
#18014=CARTESIAN_POINT('Origin',(0.,0.0158712256101377,-0.0121758532865581));
#18015=CARTESIAN_POINT('',(-0.00175000000001,0.0158712256101377,-0.00902919570294742));
#18016=CARTESIAN_POINT('Origin',(0.,0.0155212256101277,-0.0121758532865581));
#18017=CARTESIAN_POINT('',(0.00175,0.0155212256101277,-0.00871852411507327));
#18018=CARTESIAN_POINT('',(0.00175000000001,0.0155212256101277,-0.00871852411506327));
#18019=CARTESIAN_POINT('',(0.002425,0.0155212256101277,-0.0151982695384996));
#18020=CARTESIAN_POINT('Origin',(0.,0.0155212256101277,-0.0121758532865581));
#18021=CARTESIAN_POINT('',(0.002425,0.0163712256101277,-0.0151982695384996));
#18022=CARTESIAN_POINT('',(0.00242500000001,0.0155212256101277,-0.0151982695385096));
#18023=CARTESIAN_POINT('Origin',(0.,0.0163712256101377,-0.0121758532865581));
#18024=CARTESIAN_POINT('Origin',(0.00175,0.0155212256101277,-0.0104612104666099));
#18025=CARTESIAN_POINT('',(0.00175,0.0163712256101277,-0.0104612104666099));
#18026=CARTESIAN_POINT('',(0.00175000000001,0.0163712256101377,-0.0121758532865581));
#18027=CARTESIAN_POINT('',(0.00175,0.0155212256101277,-0.0104612104666099));
#18028=CARTESIAN_POINT('',(0.00175000000001,0.0155212256101277,-0.0104612104665999));
#18029=CARTESIAN_POINT('',(0.00175000000001,0.0155212256101277,-0.0121758532865581));
#18030=CARTESIAN_POINT('Origin',(-0.00175,0.0155212256101277,-0.00871852411507327));
#18031=CARTESIAN_POINT('',(-0.00175,0.0155212256101277,-0.00871852411507327));
#18032=CARTESIAN_POINT('',(-0.00175000000001,0.0155212256101277,-0.00871852411506327));
#18033=CARTESIAN_POINT('',(-0.00175,0.0155212256101277,-0.0104612104666099));
#18034=CARTESIAN_POINT('',(-0.00175000000001,0.0155212256101277,-0.0121758532865581));
#18035=CARTESIAN_POINT('',(-0.00175,0.0163712256101277,-0.0104612104666099));
#18036=CARTESIAN_POINT('',(-0.00175000000001,0.0155212256101277,-0.0104612104665999));
#18037=CARTESIAN_POINT('',(-0.00175000000001,0.0163712256101377,-0.0121758532865581));
#18038=CARTESIAN_POINT('Origin',(0.002425,0.0155212256101277,-0.0168508532865581));
#18039=CARTESIAN_POINT('',(-0.002425,0.0155212256101277,-0.0168508532865581));
#18040=CARTESIAN_POINT('',(0.002425,0.0155212256101277,-0.0168508532865581));
#18041=CARTESIAN_POINT('',(-0.00242500000001,0.0155212256101277,-0.0168508532865681));
#18042=CARTESIAN_POINT('',(-0.002425,0.0176212256101277,-0.0168508532865581));
#18043=CARTESIAN_POINT('',(-0.00242500000001,0.0155212256101277,-0.0168508532865681));
#18044=CARTESIAN_POINT('',(0.002425,0.0176212256101277,-0.0168508532865581));
#18045=CARTESIAN_POINT('',(-0.00242500000001,0.0176212256101377,-0.0168508532865681));
#18046=CARTESIAN_POINT('',(0.00242500000001,0.0155212256101277,-0.0168508532865681));
#18047=CARTESIAN_POINT('Origin',(-0.002425,0.0155212256101277,-0.0160508532865581));
#18048=CARTESIAN_POINT('',(0.002425,0.0163712256101277,-0.0160508532865581));
#18049=CARTESIAN_POINT('',(-0.002425,0.0163712256101277,-0.0160508532865581));
#18050=CARTESIAN_POINT('',(-0.00242500000001,0.0163712256101377,-0.0160508532865681));
#18051=CARTESIAN_POINT('',(0.002425,0.0176212256101277,-0.0160508532865581));
#18052=CARTESIAN_POINT('',(0.00242500000001,0.0155212256101277,-0.0160508532865681));
#18053=CARTESIAN_POINT('',(-0.002425,0.0176212256101277,-0.0160508532865581));
#18054=CARTESIAN_POINT('',(-0.00242500000001,0.0176212256101377,-0.0160508532865681));
#18055=CARTESIAN_POINT('',(-0.00242500000001,0.0155212256101277,-0.0160508532865681));
#18056=CARTESIAN_POINT('Origin',(0.,0.0176212256101277,-0.0164508532865581));
#18057=CARTESIAN_POINT('',(-0.00242500000001,0.0176212256101377,-0.0160508532865681));
#18058=CARTESIAN_POINT('',(0.00242500000001,0.0176212256101377,-0.0168508532865681));
#18059=CARTESIAN_POINT('Origin',(0.,0.0155212256101277,-0.0121758532865581));
#18060=CARTESIAN_POINT('Origin',(0.,0.0155212256101277,-0.0121758532865581));
#18061=CARTESIAN_POINT('Origin',(0.,0.0163712256101377,-0.0121758532865581));
#18062=CARTESIAN_POINT('Origin',(0.,0.0155212256101277,-0.0121758532865581));
#18063=CARTESIAN_POINT('',(-0.002425,0.0163712256101277,-0.0151982695384996));
#18064=CARTESIAN_POINT('Origin',(0.,0.0163712256101377,-0.0121758532865581));
#18065=CARTESIAN_POINT('',(-0.002425,0.0155212256101277,-0.0151982695384996));
#18066=CARTESIAN_POINT('',(-0.00242500000001,0.0155212256101277,-0.0151982695385096));
#18067=CARTESIAN_POINT('Origin',(0.,0.0155212256101277,-0.0121758532865581));
#18068=CARTESIAN_POINT('Origin',(-0.002425,0.0155212256101277,-0.0160508532865581));
#18069=CARTESIAN_POINT('',(-0.00242500000001,0.0155212256101277,-0.0160508532865681));
#18070=CARTESIAN_POINT('',(-0.00242500000001,0.0163712256101377,-0.0151982695385096));
#18071=CARTESIAN_POINT('Origin',(0.002425,0.0155212256101277,-0.0151982695384996));
#18072=CARTESIAN_POINT('',(0.00242500000001,0.0155212256101277,-0.0160508532865681));
#18073=CARTESIAN_POINT('',(0.00242500000001,0.0163712256101377,-0.0160508532865681));
#18074=CARTESIAN_POINT('Origin',(0.,0.0163712256101277,-0.0123846887008157));
#18075=CARTESIAN_POINT('Origin',(0.,0.0155212256101277,-0.0123846887008157));
#18076=CARTESIAN_POINT('',(0.,0.,0.));
#18077=CARTESIAN_POINT('Origin',(-0.0200268362756705,-0.033370488273017,
0.0038241467581455));
#18078=CARTESIAN_POINT('',(-0.0198966001424301,-0.0326318824582561,0.0038241467581455));
#18079=CARTESIAN_POINT('Origin',(-0.0200268362756803,-0.0333704882730153,
0.0038241467581555));
#18080=CARTESIAN_POINT('Origin',(-0.00623952773349959,-0.035801562760354,
0.000824146758145402));
#18081=CARTESIAN_POINT('',(-0.00610929160024941,-0.0350629569455948,-0.00217585328655807));
#18082=CARTESIAN_POINT('Origin',(-0.00623952773350945,-0.0358015627603522,
-0.00217585328654807));
#18083=CARTESIAN_POINT('',(-0.00610929160024939,-0.0350629569455948,0.000824146758165404));
#18084=CARTESIAN_POINT('',(-0.00610929160024939,-0.0350629569455948,0.000824146758145402));
#18085=CARTESIAN_POINT('',(-0.00697813354827845,-0.0356713266271003,0.000824146758145408));
#18086=CARTESIAN_POINT('Origin',(-0.00623952773350944,-0.0358015627603522,
0.000824146758155403));
#18087=CARTESIAN_POINT('Origin',(-0.00623952773350944,-0.0358015627603522,
0.000824146758155403));
#18088=CARTESIAN_POINT('Origin',(-0.00919395099253621,-0.0352806182273532,
0.000824146758145423));
#18089=CARTESIAN_POINT('',(-0.00919395099254606,-0.0352806182273515,0.00307414675814542));
#18090=CARTESIAN_POINT('Origin',(-0.00919395099253621,-0.0352806182273532,
0.000824146758145423));
#18091=CARTESIAN_POINT('',(-0.00906371485929584,-0.0345420124125923,0.00382414675814543));
#18092=CARTESIAN_POINT('Origin',(-0.00919395099254604,-0.0352806182273514,
0.00382414675815542));
#18093=CARTESIAN_POINT('Origin',(-0.00919395099254604,-0.0352806182273514,
0.00382414675815542));
#18094=CARTESIAN_POINT('Origin',(-0.0239660672877193,-0.0326758955623493,
0.00382414675814553));
#18095=CARTESIAN_POINT('',(-0.0238358311544691,-0.0319372897475901,0.00382414675814553));
#18096=CARTESIAN_POINT('Origin',(-0.00623952773349961,-0.035801562760354,
-0.00217585328655807));
#18097=CARTESIAN_POINT('',(0.,0.,0.));
#18098=CARTESIAN_POINT('Origin',(-0.00676047226650036,-0.0387559860193906,
0.000824146758145397));
#18099=CARTESIAN_POINT('',(-0.00669535419987528,-0.038386683112011,-0.00217585328655808));
#18100=CARTESIAN_POINT('Origin',(-0.00676047226651023,-0.0387559860193889,
-0.00217585328654808));
#18101=CARTESIAN_POINT('',(-0.00669535419987526,-0.038386683112011,0.000824146758165397));
#18102=CARTESIAN_POINT('',(-0.00669535419987526,-0.038386683112011,0.000824146758145397));
#18103=CARTESIAN_POINT('',(-0.00712977517389963,-0.038690867952762,0.000824146758145399));
#18104=CARTESIAN_POINT('Origin',(-0.00676047226651021,-0.0387559860193889,
0.000824146758155397));
#18105=CARTESIAN_POINT('Origin',(-0.00676047226651021,-0.0387559860193889,
0.000824146758155397));
#18106=CARTESIAN_POINT('Origin',(-0.00971489552553699,-0.0382350414863898,
0.000824146758145418));
#18107=CARTESIAN_POINT('',(-0.00971489552554682,-0.0382350414863881,0.00344914675814542));
#18108=CARTESIAN_POINT('Origin',(-0.00971489552553699,-0.0382350414863898,
0.000824146758145418));
#18109=CARTESIAN_POINT('',(-0.0096497774589217,-0.0378657385790085,0.00382414675814542));
#18110=CARTESIAN_POINT('Origin',(-0.00971489552554682,-0.0382350414863881,
0.00382414675815542));
#18111=CARTESIAN_POINT('Origin',(-0.00971489552554682,-0.0382350414863881,
0.00382414675815542));
#18112=CARTESIAN_POINT('Origin',(-0.0244870118207201,-0.0356303188213859,
0.00382414675814552));
#18113=CARTESIAN_POINT('',(-0.0244218937541048,-0.0352610159140046,0.00382414675814552));
#18114=CARTESIAN_POINT('',(-0.024421893754095,-0.0352610159140063,0.00382414675814552));
#18115=CARTESIAN_POINT('Origin',(-0.0244870118207299,-0.0356303188213842,
0.00382414675815552));
#18116=CARTESIAN_POINT('Origin',(-0.00676047226650038,-0.0387559860193906,
-0.00217585328655808));
#18117=CARTESIAN_POINT('Origin',(-0.0244870118207201,-0.0356303188213859,
0.00382414675814552));
#18118=CARTESIAN_POINT('',(0.,0.,0.));
#18119=CARTESIAN_POINT('Origin',(-0.00623952773349959,-0.035801562760354,
0.000824146758145402));
#18120=CARTESIAN_POINT('',(-0.00617440966687451,-0.0354322598529744,-0.00217585328655807));
#18121=CARTESIAN_POINT('Origin',(-0.00623952773350945,-0.0358015627603522,
-0.00217585328654807));
#18122=CARTESIAN_POINT('',(-0.00617440966687449,-0.0354322598529744,0.000824146758165403));
#18123=CARTESIAN_POINT('',(-0.00617440966687449,-0.0354322598529744,0.000824146758145402));
#18124=CARTESIAN_POINT('',(-0.00660883064089887,-0.0357364446937254,0.000824146758145405));
#18125=CARTESIAN_POINT('Origin',(-0.00623952773350944,-0.0358015627603522,
0.000824146758155403));
#18126=CARTESIAN_POINT('Origin',(-0.00623952773350944,-0.0358015627603522,
0.000824146758155403));
#18127=CARTESIAN_POINT('Origin',(-0.00919395099253621,-0.0352806182273532,
0.000824146758145423));
#18128=CARTESIAN_POINT('',(-0.00919395099254605,-0.0352806182273515,0.00344914675814542));
#18129=CARTESIAN_POINT('Origin',(-0.00919395099253621,-0.0352806182273532,
0.000824146758145423));
#18130=CARTESIAN_POINT('',(-0.00912883292592094,-0.0349113153199719,0.00382414675814543));
#18131=CARTESIAN_POINT('Origin',(-0.00919395099254604,-0.0352806182273514,
0.00382414675815542));
#18132=CARTESIAN_POINT('Origin',(-0.00919395099254604,-0.0352806182273514,
0.00382414675815542));
#18133=CARTESIAN_POINT('Origin',(-0.0239660672877193,-0.0326758955623493,
0.00382414675814553));
#18134=CARTESIAN_POINT('',(-0.0239009492211041,-0.032306592654968,0.00382414675814553));
#18135=CARTESIAN_POINT('',(-0.0239009492210942,-0.0323065926549697,0.00382414675814553));
#18136=CARTESIAN_POINT('Origin',(-0.0239660672877292,-0.0326758955623476,
0.00382414675815552));
#18137=CARTESIAN_POINT('Origin',(-0.00623952773349961,-0.035801562760354,
-0.00217585328655807));
#18138=CARTESIAN_POINT('Origin',(-0.0239660672877193,-0.0326758955623493,
0.00382414675814553));
#18139=CARTESIAN_POINT('',(0.,0.,0.));
#18140=CARTESIAN_POINT('Origin',(0.006,-0.0418165664398416,-0.0121758532865581));
#18141=CARTESIAN_POINT('',(0.004457,-0.0371814756795928,-0.0121758532865588));
#18142=CARTESIAN_POINT('',(0.004457,-0.0370665921755392,-0.0121758532865484));
#18143=CARTESIAN_POINT('',(0.004457,-0.0418165664398416,-0.0121758532865581));
#18144=CARTESIAN_POINT('',(0.00445696473503848,-0.0370665033115447,-0.012173946036331));
#18145=CARTESIAN_POINT('Ctrl Pts',(0.004457,-0.0370665921755392,-0.0121758532865387));
#18146=CARTESIAN_POINT('Ctrl Pts',(0.00445700000000001,-0.0370665704100319,
-0.0121754755766259));
#18147=CARTESIAN_POINT('Ctrl Pts',(0.00445700013868904,-0.0370665486443835,
-0.0121750978648529));
#18148=CARTESIAN_POINT('Ctrl Pts',(0.00445700041607119,-0.0370665268786158,
-0.0121747201512957));
#18149=CARTESIAN_POINT('',(0.00543336738605003,-0.0369714897070198,-0.0107406611481222));
#18150=CARTESIAN_POINT('Ctrl Pts',(0.00445696473503848,-0.0370665033115447,
-0.012173946036331));
#18151=CARTESIAN_POINT('Ctrl Pts',(0.00445682508442995,-0.0370607195511547,
-0.0120708997231622));
#18152=CARTESIAN_POINT('Ctrl Pts',(0.00446642871231062,-0.0370552784860267,
-0.0119678729985124));
#18153=CARTESIAN_POINT('Ctrl Pts',(0.00448680026437125,-0.0370500323662534,
-0.0118669686934194));
#18154=CARTESIAN_POINT('Ctrl Pts',(0.0045352522124094,-0.0370375549309602,
-0.0116269766627366));
#18155=CARTESIAN_POINT('Ctrl Pts',(0.00464519561945393,-0.0370261802712467,
-0.0113987962647978));
#18156=CARTESIAN_POINT('Ctrl Pts',(0.00479913627550219,-0.0370139205143147,
-0.0112081339394185));
#18157=CARTESIAN_POINT('Ctrl Pts',(0.00496595972382667,-0.0370006347782426,
-0.0110015157048218));
#18158=CARTESIAN_POINT('Ctrl Pts',(0.00518626704742854,-0.0369851941685886,
-0.0108382129844631));
#18159=CARTESIAN_POINT('Ctrl Pts',(0.00543336738418062,-0.0369714897101142,
-0.010740661146572));
#18160=CARTESIAN_POINT('',(0.00581125245410382,-0.0370677682650875,-0.0106436206577455));
#18161=CARTESIAN_POINT('Ctrl Pts',(0.00581141341884543,-0.0370672590668868,
-0.0106444212438581));
#18162=CARTESIAN_POINT('Ctrl Pts',(0.00576806064819256,-0.0370619449087914,
-0.010649759875004));
#18163=CARTESIAN_POINT('Ctrl Pts',(0.00572496277193653,-0.0370547949103012,
-0.0106569430206965));
#18164=CARTESIAN_POINT('Ctrl Pts',(0.00559660094773692,-0.0370279297986178,
-0.0106839354017503));
#18165=CARTESIAN_POINT('Ctrl Pts',(0.00551294803925241,-0.037002745347212,
-0.0107092416638838));
#18166=CARTESIAN_POINT('Ctrl Pts',(0.00543336738593308,-0.0369714897050595,
-0.010740661145876));
#18167=CARTESIAN_POINT('',(0.00445700028015853,-0.0371814311999794,-0.0121749234644574));
#18168=CARTESIAN_POINT('Ctrl Pts',(0.00581095120124511,-0.0370682602733425,
-0.01064447823397));
#18169=CARTESIAN_POINT('Ctrl Pts',(0.00579234229401333,-0.0370693014592163,
-0.0106467755102331));
#18170=CARTESIAN_POINT('Ctrl Pts',(0.0057737761556256,-0.03707033323956,
-0.0106494118730359));
#18171=CARTESIAN_POINT('Ctrl Pts',(0.00574225603645012,-0.0370720680688304,
-0.0106544754334336));
#18172=CARTESIAN_POINT('Ctrl Pts',(0.00572927689885044,-0.0370727775234059,
-0.0106567313214004));
#18173=CARTESIAN_POINT('Ctrl Pts',(0.00570792885345587,-0.0370739346080628,
-0.0106607240984138));
#18174=CARTESIAN_POINT('Ctrl Pts',(0.00569954283859992,-0.0370743866244655,
-0.0106623647627505));
#18175=CARTESIAN_POINT('Ctrl Pts',(0.00568340492125055,-0.0370752510584431,
-0.0106656614509511));
#18176=CARTESIAN_POINT('Ctrl Pts',(0.00567565122453858,-0.0370756639572011,
-0.0106673077270314));
#18177=CARTESIAN_POINT('Ctrl Pts',(0.00565870685475073,-0.0370765604788409,
-0.010671042067358));
#18178=CARTESIAN_POINT('Ctrl Pts',(0.0056495220206615,-0.0370770427706411,
-0.0106731547103358));
#18179=CARTESIAN_POINT('Ctrl Pts',(0.0056233619690746,-0.0370784073533569,
-0.0106794248005471));
#18180=CARTESIAN_POINT('Ctrl Pts',(0.00560643682090592,-0.0370792792695538,
-0.0106837867698845));
#18181=CARTESIAN_POINT('Ctrl Pts',(0.00552448525263467,-0.0370834631690544,
-0.0107063990048912));
#18182=CARTESIAN_POINT('Ctrl Pts',(0.00546062594759169,-0.0370866084949523,
-0.0107286189551597));
#18183=CARTESIAN_POINT('Ctrl Pts',(0.00532773457379046,-0.0370932706475194,
-0.010784882070171));
#18184=CARTESIAN_POINT('Ctrl Pts',(0.00525937729396276,-0.0370967732312161,
-0.0108200437749403));
#18185=CARTESIAN_POINT('Ctrl Pts',(0.00516528586352355,-0.0371019833621321,
-0.0108776895128799));
#18186=CARTESIAN_POINT('Ctrl Pts',(0.0051372306427446,-0.0371035899557449,
-0.0108961635778762));
#18187=CARTESIAN_POINT('Ctrl Pts',(0.00508780389631469,-0.0371065378973649,
-0.0109310751634043));
#18188=CARTESIAN_POINT('Ctrl Pts',(0.00506621776725708,-0.0371078681862633,
-0.0109471853309022));
#18189=CARTESIAN_POINT('Ctrl Pts',(0.00503252226858799,-0.0371100207712954,
-0.0109737339824954));
#18190=CARTESIAN_POINT('Ctrl Pts',(0.00502013401202563,-0.037110829274222,
-0.0109838102488626));
#18191=CARTESIAN_POINT('Ctrl Pts',(0.00499673714829802,-0.0371123905174636,
-0.0110034517959461));
#18192=CARTESIAN_POINT('Ctrl Pts',(0.00498570335728822,-0.0371131419212072,
-0.0110129844605238));
#18193=CARTESIAN_POINT('Ctrl Pts',(0.00496055713795835,-0.0371148904823943,
-0.0110353397799863));
#18194=CARTESIAN_POINT('Ctrl Pts',(0.00494654418660995,-0.0371158919816601,
-0.0110482703278011));
#18195=CARTESIAN_POINT('Ctrl Pts',(0.00490196780727019,-0.03711916832195,
-0.0110909598345263));
#18196=CARTESIAN_POINT('Ctrl Pts',(0.00487239956716035,-0.0371214845949833,
-0.0111217255363832));
#18197=CARTESIAN_POINT('Ctrl Pts',(0.00479850634010012,-0.0371276564291069,
-0.0112052821974612));
#18198=CARTESIAN_POINT('Ctrl Pts',(0.00475637781415507,-0.0371315784249489,
-0.0112598849892025));
#18199=CARTESIAN_POINT('Ctrl Pts',(0.00467070337278055,-0.0371403937136393,
-0.011387783336617));
#18200=CARTESIAN_POINT('Ctrl Pts',(0.00462928731841433,-0.0371452860467748,
-0.0114622482202439));
#18201=CARTESIAN_POINT('Ctrl Pts',(0.00458722942930083,-0.0371508441390535,
-0.0115551958006175));
#18202=CARTESIAN_POINT('Ctrl Pts',(0.00458049533488884,-0.0371517568163958,
-0.0115707558146567));
#18203=CARTESIAN_POINT('Ctrl Pts',(0.00457043943478568,-0.0371531528710488,
-0.011595083635554));
#18204=CARTESIAN_POINT('Ctrl Pts',(0.00456693893407913,-0.0371536456263738,
-0.0116037756806916));
#18205=CARTESIAN_POINT('Ctrl Pts',(0.00456051083071472,-0.0371545627915118,
-0.0116201665403943));
#18206=CARTESIAN_POINT('Ctrl Pts',(0.00455756539274089,-0.0371549881334905,
-0.0116278576355199));
#18207=CARTESIAN_POINT('Ctrl Pts',(0.00455051208629032,-0.0371560199398415,
-0.0116467260960982));
#18208=CARTESIAN_POINT('Ctrl Pts',(0.00454647170928672,-0.0371566226394305,
-0.0116579282725353));
#18209=CARTESIAN_POINT('Ctrl Pts',(0.00453143623820617,-0.0371589156491401,
-0.0117011772912719));
#18210=CARTESIAN_POINT('Ctrl Pts',(0.00452136746047995,-0.0371605604294028,
-0.0117335378869258));
#18211=CARTESIAN_POINT('Ctrl Pts',(0.00449557653918292,-0.0371651861971653,
-0.0118271971474061));
#18212=CARTESIAN_POINT('Ctrl Pts',(0.00448254734367659,-0.0371680865114223,
-0.0118891666859977));
#18213=CARTESIAN_POINT('Ctrl Pts',(0.00446251211444976,-0.0371744246287094,
-0.0120256592311372));
#18214=CARTESIAN_POINT('Ctrl Pts',(0.00445704528366618,-0.0371778592144949,
-0.0121002420831587));
#18215=CARTESIAN_POINT('Ctrl Pts',(0.00445700028015854,-0.0371814311999789,
-0.0121749234644459));
#18216=CARTESIAN_POINT('Ctrl Pts',(0.004457,-0.0371814756795928,-0.0121758532865595));
#18217=CARTESIAN_POINT('Ctrl Pts',(0.004457,-0.0371814606916064,-0.0121755400169382));
#18218=CARTESIAN_POINT('Ctrl Pts',(0.00445700009137941,-0.0371814461836175,
-0.0121752367352671));
#18219=CARTESIAN_POINT('Ctrl Pts',(0.00445700028015853,-0.0371814311999794,
-0.0121749234644572));
#18220=CARTESIAN_POINT('Origin',(0.006,-0.0418165664398416,-0.0121758532865581));
#18221=CARTESIAN_POINT('',(0.004457,-0.0376822061652104,-0.0121758532865608));
#18222=CARTESIAN_POINT('',(0.004457,-0.037567972222619,-0.0121758532865581));
#18223=CARTESIAN_POINT('',(0.004457,-0.0418165664398416,-0.0121758532865581));
#18224=CARTESIAN_POINT('',(0.00445700000153134,-0.0375679687511446,-0.0121757845426831));
#18225=CARTESIAN_POINT('Ctrl Pts',(0.00445700000200862,-0.0375679682467928,
-0.0121757745554097));
#18226=CARTESIAN_POINT('Ctrl Pts',(0.00445700000083941,-0.0375679695720835,
-0.0121758007991274));
#18227=CARTESIAN_POINT('Ctrl Pts',(0.004457,-0.0375679708973641,-0.0121758270428433));
#18228=CARTESIAN_POINT('Ctrl Pts',(0.004457,-0.037567972222619,-0.0121758532865581));
#18229=CARTESIAN_POINT('Ctrl Pts',(0.00445700000153134,-0.0375679687511446,
-0.0121757845426831));
#18230=CARTESIAN_POINT('Ctrl Pts',(0.00445700036683925,-0.0375675546782457,
-0.0121675849742589));
#18231=CARTESIAN_POINT('Ctrl Pts',(0.004457066091393,-0.0375671386197308,
-0.0121593856361153));
#18232=CARTESIAN_POINT('Ctrl Pts',(0.00445733677550361,-0.037566275221113,
-0.0121424549421407));
#18233=CARTESIAN_POINT('Ctrl Pts',(0.00445755052059262,-0.03756582762505,
-0.0121337240450385));
#18234=CARTESIAN_POINT('Ctrl Pts',(0.00445833751673252,-0.0375645975608631,
-0.0121098599235097));
#18235=CARTESIAN_POINT('Ctrl Pts',(0.00445905944675096,-0.0375638105169478,
-0.0120947328458213));
#18236=CARTESIAN_POINT('Ctrl Pts',(0.00446155134286164,-0.0375617156770453,
-0.0120548560197195));
#18237=CARTESIAN_POINT('Ctrl Pts',(0.0044636957851817,-0.037560396480823,
-0.0120301348115956));
#18238=CARTESIAN_POINT('Ctrl Pts',(0.00447852383692101,-0.0375531609460893,
-0.0118966668724493));
#18239=CARTESIAN_POINT('Ctrl Pts',(0.00450215713675417,-0.0375469090791664,
-0.011789465728744));
#18240=CARTESIAN_POINT('Ctrl Pts',(0.00455415940330839,-0.037537513609922,
-0.011634247692209));
#18241=CARTESIAN_POINT('Ctrl Pts',(0.00457409310536596,-0.0375344053760627,
-0.0115837539491281));
#18242=CARTESIAN_POINT('Ctrl Pts',(0.00460952027265135,-0.0375296448493669,
-0.0115062457089519));
#18243=CARTESIAN_POINT('Ctrl Pts',(0.00462324101949698,-0.0375279415203038,
-0.0114784702343028));
#18244=CARTESIAN_POINT('Ctrl Pts',(0.00464315607613126,-0.037525667984562,
-0.0114410375780365));
#18245=CARTESIAN_POINT('Ctrl Pts',(0.00464863488965225,-0.0375250611632817,
-0.0114310097372368));
#18246=CARTESIAN_POINT('Ctrl Pts',(0.0046581515367496,-0.0375240394412014,
-0.0114140421956841));
#18247=CARTESIAN_POINT('Ctrl Pts',(0.00466213298287001,-0.0375236211993594,
-0.0114070715937107));
#18248=CARTESIAN_POINT('Ctrl Pts',(0.00467079890131458,-0.0375227307038318,
-0.0113921707890997));
#18249=CARTESIAN_POINT('Ctrl Pts',(0.00467550021541715,-0.0375222594936024,
-0.011384251021267));
#18250=CARTESIAN_POINT('Ctrl Pts',(0.00468899872004694,-0.0375209383175919,
-0.0113619685894859));
#18251=CARTESIAN_POINT('Ctrl Pts',(0.00469796076624327,-0.0375200981518808,
-0.0113477068426694));
#18252=CARTESIAN_POINT('Ctrl Pts',(0.0047666831178511,-0.0375139032600975,
-0.0112422198767264));
#18253=CARTESIAN_POINT('Ctrl Pts',(0.00483573667388354,-0.0375090149274492,
-0.0111574046017778));
#18254=CARTESIAN_POINT('Ctrl Pts',(0.00495192617621242,-0.0375014841625381,
-0.011042110701276));
#18255=CARTESIAN_POINT('Ctrl Pts',(0.00499270164061338,-0.0374989480608549,
-0.0110057333950119));
#18256=CARTESIAN_POINT('Ctrl Pts',(0.00506473205692808,-0.037494539477578,
-0.0109480327509385));
#18257=CARTESIAN_POINT('Ctrl Pts',(0.00509499810502276,-0.0374927067697491,
-0.0109255570435091));
#18258=CARTESIAN_POINT('Ctrl Pts',(0.00514059554449525,-0.0374899547927506,
-0.0108942198522462));
#18259=CARTESIAN_POINT('Ctrl Pts',(0.00515530574282756,-0.0374890683793864,
-0.0108844773313338));
#18260=CARTESIAN_POINT('Ctrl Pts',(0.00518189678129539,-0.0374874669049695,
-0.0108675149170964));
#18261=CARTESIAN_POINT('Ctrl Pts',(0.00519371435586635,-0.0374867554790625,
-0.0108601992252512));
#18262=CARTESIAN_POINT('Ctrl Pts',(0.00521942598941529,-0.0374852075702802,
-0.0108447589166292));
#18263=CARTESIAN_POINT('Ctrl Pts',(0.00523335149436794,-0.0374843691820669,
-0.0108366900962038));
#18264=CARTESIAN_POINT('Ctrl Pts',(0.00527208242528318,-0.0374820364000232,
-0.0108150504413171));
#18265=CARTESIAN_POINT('Ctrl Pts',(0.00529713771615109,-0.0374805261187882,
-0.0108019417719247));
#18266=CARTESIAN_POINT('Ctrl Pts',(0.0054368125096652,-0.0374720988443577,
-0.0107336861720272));
#18267=CARTESIAN_POINT('Ctrl Pts',(0.00555754287442518,-0.0374647292666306,
-0.0106921925661276));
#18268=CARTESIAN_POINT('Ctrl Pts',(0.00573757933703765,-0.037454231120333,
-0.0106542704758986));
#18269=CARTESIAN_POINT('Ctrl Pts',(0.00579380023103691,-0.0374510284780135,
-0.0106456371166781));
#18270=CARTESIAN_POINT('Ctrl Pts',(0.00586394308740783,-0.0374472214141527,
-0.010638803056727));
#18271=CARTESIAN_POINT('Ctrl Pts',(0.00587753045972386,-0.0374464927284362,
-0.0106376607989248));
#18272=CARTESIAN_POINT('Ctrl Pts',(0.0058995572969287,-0.0374453275855413,
-0.0106361027838862));
#18273=CARTESIAN_POINT('Ctrl Pts',(0.00590798795073027,-0.0374448854571853,
-0.0106355759940659));
#18274=CARTESIAN_POINT('Ctrl Pts',(0.0059249253774154,-0.0374440054670575,
-0.0106346572222441));
#18275=CARTESIAN_POINT('Ctrl Pts',(0.00593343188448871,-0.0374435676700767,
-0.0106342663768265));
#18276=CARTESIAN_POINT('Ctrl Pts',(0.00595582615989271,-0.0374424250766993,
-0.0106334231480532));
#18277=CARTESIAN_POINT('Ctrl Pts',(0.00596971781879187,-0.0374417263660004,
-0.0106330878880061));
#18278=CARTESIAN_POINT('Ctrl Pts',(0.00604182414024253,-0.0374381433454097,
-0.0106323220389861));
#18279=CARTESIAN_POINT('Ctrl Pts',(0.00610002915600085,-0.0374353979734819,
-0.0106349985707756));
#18280=CARTESIAN_POINT('Ctrl Pts',(0.0062496461293218,-0.037428424753463,
-0.0106503948495736));
#18281=CARTESIAN_POINT('Ctrl Pts',(0.00634031302894067,-0.037424270897813,
-0.010668029077274));
#18282=CARTESIAN_POINT('Ctrl Pts',(0.00647757486073544,-0.0374175503828472,
-0.0107077447724282));
#18283=CARTESIAN_POINT('Ctrl Pts',(0.00652555764722635,-0.0374151173768708,
-0.0107242304229163));
#18284=CARTESIAN_POINT('Ctrl Pts',(0.00659075670370055,-0.0374116442747195,
-0.0107502880731383));
#18285=CARTESIAN_POINT('Ctrl Pts',(0.00660873436705773,-0.0374106685936182,
-0.0107578715912458));
#18286=CARTESIAN_POINT('Ctrl Pts',(0.0066396071801554,-0.0374089593369137,
-0.0107715899906488));
#18287=CARTESIAN_POINT('Ctrl Pts',(0.00665257008243262,-0.0374082311462968,
-0.0107775668284452));
#18288=CARTESIAN_POINT('Ctrl Pts',(0.00667920375237414,-0.0374067123600755,
-0.0107902979029145));
#18289=CARTESIAN_POINT('Ctrl Pts',(0.00669286102072801,-0.0374059209788032,
-0.0107970766395812));
#18290=CARTESIAN_POINT('Ctrl Pts',(0.0067283833117898,-0.0374038286161549,
-0.0108153690640117));
#18291=CARTESIAN_POINT('Ctrl Pts',(0.00675007551911772,-0.0374025164953747,
-0.0108272072281915));
#18292=CARTESIAN_POINT('Ctrl Pts',(0.0068700111172489,-0.0373950642134218,
-0.0108964488881031));
#18293=CARTESIAN_POINT('Ctrl Pts',(0.00696194191788553,-0.0373885570674098,
-0.0109640547249231));
#18294=CARTESIAN_POINT('Ctrl Pts',(0.00708399771578481,-0.0373790338193812,
-0.0110765238618972));
#18295=CARTESIAN_POINT('Ctrl Pts',(0.00712058252476247,-0.0373760456902483,
-0.0111138403540489));
#18296=CARTESIAN_POINT('Ctrl Pts',(0.00717527849721377,-0.0373714413427317,
-0.0111756101955631));
#18297=CARTESIAN_POINT('Ctrl Pts',(0.00719468087906294,-0.0373697775682962,
-0.0111988662842938));
#18298=CARTESIAN_POINT('Ctrl Pts',(0.00722039464420038,-0.0373675464793812,
-0.0112315998325648));
#18299=CARTESIAN_POINT('Ctrl Pts',(0.00722730355542674,-0.0373669442667177,
-0.0112405973479549));
#18300=CARTESIAN_POINT('Ctrl Pts',(0.00723891757216372,-0.0373659283631549,
-0.011256072702156));
#18301=CARTESIAN_POINT('Ctrl Pts',(0.00724367257172003,-0.0373655113977234,
-0.0112625123760226));
#18302=CARTESIAN_POINT('Ctrl Pts',(0.00725377398820771,-0.037364623735917,
-0.0112764178554385));
#18303=CARTESIAN_POINT('Ctrl Pts',(0.00725910419246762,-0.0373641540858661,
-0.0112838947959566));
#18304=CARTESIAN_POINT('Ctrl Pts',(0.0072740536613627,-0.0373628319007741,
-0.011305266223386));
#18305=CARTESIAN_POINT('Ctrl Pts',(0.00728351209778681,-0.0373619893569193,
-0.0113192721142523));
#18306=CARTESIAN_POINT('Ctrl Pts',(0.00734754084555967,-0.0373562226148416,
-0.0114175274206311));
#18307=CARTESIAN_POINT('Ctrl Pts',(0.00739401157649186,-0.0373516961613388,
-0.0115067791373772));
#18308=CARTESIAN_POINT('Ctrl Pts',(0.00746243966882219,-0.0373432940227781,
-0.0116768575188318));
#18309=CARTESIAN_POINT('Ctrl Pts',(0.00748713932881683,-0.0373394561462299,
-0.0117561609103953));
#18310=CARTESIAN_POINT('Ctrl Pts',(0.007511045570467,-0.0373341551442661,
-0.0118623823723639));
#18311=CARTESIAN_POINT('Ctrl Pts',(0.00751610465056322,-0.0373328736306451,
-0.011887844047252));
#18312=CARTESIAN_POINT('Ctrl Pts',(0.00752313988089788,-0.0373307991420372,
-0.0119286057033465));
#18313=CARTESIAN_POINT('Ctrl Pts',(0.00752553309264297,-0.0373300193551603,
-0.0119438290953035));
#18314=CARTESIAN_POINT('Ctrl Pts',(0.00752967067934738,-0.0373285150887994,
-0.0119729892418283));
#18315=CARTESIAN_POINT('Ctrl Pts',(0.00753145356782104,-0.0373277919089775,
-0.0119869190116834));
#18316=CARTESIAN_POINT('Ctrl Pts',(0.00753511882058764,-0.0373261135709884,
-0.0120190308186336));
#18317=CARTESIAN_POINT('Ctrl Pts',(0.00753686870113858,-0.037325154357965,
-0.012037225595434));
#18318=CARTESIAN_POINT('Ctrl Pts',(0.00754143203016847,-0.0373220533324374,
-0.0120955259236818));
#18319=CARTESIAN_POINT('Ctrl Pts',(0.00754300139234045,-0.0373198739337048,
-0.0121357097610633));
#18320=CARTESIAN_POINT('Ctrl Pts',(0.0075429978187607,-0.0373141789562194,
-0.0122388179429579));
#18321=CARTESIAN_POINT('Ctrl Pts',(0.00753914814721549,-0.0373106074087205,
-0.0123016657468015));
#18322=CARTESIAN_POINT('Ctrl Pts',(0.00751960223318753,-0.0373014257575527,
-0.0124606816976951));
#18323=CARTESIAN_POINT('Ctrl Pts',(0.00749862014934309,-0.0372957809931752,
-0.0125559292485683));
#18324=CARTESIAN_POINT('Ctrl Pts',(0.00746391223862542,-0.0372896181361719,
-0.0126637723737436));
#18325=CARTESIAN_POINT('Ctrl Pts',(0.00745878334720777,-0.0372887595169188,
-0.0126788992712031));
#18326=CARTESIAN_POINT('Ctrl Pts',(0.00745043058387969,-0.0372874416061686,
-0.0127023315914479));
#18327=CARTESIAN_POINT('Ctrl Pts',(0.00744736822694468,-0.0372869737693592,
-0.0127106929891292));
#18328=CARTESIAN_POINT('Ctrl Pts',(0.00744137248617305,-0.0372860871171274,
-0.0127266349250464));
#18329=CARTESIAN_POINT('Ctrl Pts',(0.00743845132405704,-0.0372856676704713,
-0.0127342195167429));
#18330=CARTESIAN_POINT('Ctrl Pts',(0.00743105918551647,-0.0372846359532452,
-0.0127529696147484));
#18331=CARTESIAN_POINT('Ctrl Pts',(0.00742651723500039,-0.0372840277243301,
-0.0127641068406663));
#18332=CARTESIAN_POINT('Ctrl Pts',(0.00740791653239397,-0.0372816319761763,
-0.0128082344845304));
#18333=CARTESIAN_POINT('Ctrl Pts',(0.00739283903672585,-0.0372798964208051,
-0.0128407853772031));
#18334=CARTESIAN_POINT('Ctrl Pts',(0.00734493960735212,-0.0372748657479876,
-0.0129354007355388));
#18335=CARTESIAN_POINT('Ctrl Pts',(0.00730900242836076,-0.0372716707543755,
-0.0129957852335895));
#18336=CARTESIAN_POINT('Ctrl Pts',(0.00721956307573803,-0.0372644591299455,
-0.0131251123255407));
#18337=CARTESIAN_POINT('Ctrl Pts',(0.00716408109886085,-0.0372604366230465,
-0.0131923868203658));
#18338=CARTESIAN_POINT('Ctrl Pts',(0.00708503837444482,-0.0372549273831142,
-0.0132732217595692));
#18339=CARTESIAN_POINT('Ctrl Pts',(0.00706638272686283,-0.0372536419645699,
-0.0132913592807271));
#18340=CARTESIAN_POINT('Ctrl Pts',(0.00703586695466366,-0.0372515567934154,
-0.0133195622053423));
#18341=CARTESIAN_POINT('Ctrl Pts',(0.00702429742344623,-0.0372507700642419,
-0.0133299352613626));
#18342=CARTESIAN_POINT('Ctrl Pts',(0.0070018383465379,-0.0372492490353765,
-0.0133494679326557));
#18343=CARTESIAN_POINT('Ctrl Pts',(0.00699097485842589,-0.0372485159869813,
-0.0133586551390801));
#18344=CARTESIAN_POINT('Ctrl Pts',(0.00696534417377876,-0.0372467919535568,
-0.0133797299237081));
#18345=CARTESIAN_POINT('Ctrl Pts',(0.00695048208177023,-0.0372457963723621,
-0.0133914980131092));
#18346=CARTESIAN_POINT('Ctrl Pts',(0.00689872123111179,-0.0372423416385964,
-0.0134309537000006));
#18347=CARTESIAN_POINT('Ctrl Pts',(0.00686080230786232,-0.0372398313314462,
-0.0134572570927065));
#18348=CARTESIAN_POINT('Ctrl Pts',(0.00675704604002398,-0.0372330255087243,
-0.0135225444867078));
#18349=CARTESIAN_POINT('Ctrl Pts',(0.00668939375266912,-0.0372286464948173,
-0.0135583982849544));
#18350=CARTESIAN_POINT('Ctrl Pts',(0.00655178285281245,-0.0372200334028997,
-0.0136187080353799));
#18351=CARTESIAN_POINT('Ctrl Pts',(0.00648215511062513,-0.0372158120649407,
-0.0136434438346568));
#18352=CARTESIAN_POINT('Ctrl Pts',(0.00639425967259434,-0.0372108396799751,
-0.0136677348842645));
#18353=CARTESIAN_POINT('Ctrl Pts',(0.00637742078717573,-0.0372099030030866,
-0.013672083545818));
#18354=CARTESIAN_POINT('Ctrl Pts',(0.0063514911051979,-0.0372084886935629,
-0.0136783142896055));
#18355=CARTESIAN_POINT('Ctrl Pts',(0.00634245128303714,-0.0372080008106931,
-0.0136804004576085));
#18356=CARTESIAN_POINT('Ctrl Pts',(0.00632534517926319,-0.0372070880791505,
-0.0136841859597881));
#18357=CARTESIAN_POINT('Ctrl Pts',(0.00631728325447214,-0.0372066623618087,
-0.01368590238398));
#18358=CARTESIAN_POINT('Ctrl Pts',(0.00629754519214838,-0.0372056301708268,
-0.0136899396669655));
#18359=CARTESIAN_POINT('Ctrl Pts',(0.00628585496735973,-0.0372050274127528,
-0.0136921902090326));
#18360=CARTESIAN_POINT('Ctrl Pts',(0.00624115918010713,-0.0372027515779952,
-0.0137002595339077));
#18361=CARTESIAN_POINT('Ctrl Pts',(0.00620799158463117,-0.0372011221897333,
-0.013705138061047));
#18362=CARTESIAN_POINT('Ctrl Pts',(0.00611278983737598,-0.0371965502406656,
-0.0137159860027831));
#18363=CARTESIAN_POINT('Ctrl Pts',(0.0060505169583431,-0.0371936842479466,
-0.0137192842186365));
#18364=CARTESIAN_POINT('Ctrl Pts',(0.00589621090538066,-0.0371865709334765,
-0.0137181054416812));
#18365=CARTESIAN_POINT('Ctrl Pts',(0.00580445998840567,-0.0371823212708795,
-0.0137091753127247));
#18366=CARTESIAN_POINT('Ctrl Pts',(0.0056888613771523,-0.037176578327035,
-0.0136873754193712));
#18367=CARTESIAN_POINT('Ctrl Pts',(0.00566378896351049,-0.0371753098393779,
-0.0136819968550634));
#18368=CARTESIAN_POINT('Ctrl Pts',(0.00562373997997504,-0.0371732409887976,
-0.0136723556612654));
#18369=CARTESIAN_POINT('Ctrl Pts',(0.00560867323883922,-0.037172452864617,
-0.0136684866320135));
#18370=CARTESIAN_POINT('Ctrl Pts',(0.00557976098804718,-0.03717092042846,
-0.013660594336834));
#18371=CARTESIAN_POINT('Ctrl Pts',(0.00556590828193305,-0.0371701772117645,
-0.0136566034935576));
#18372=CARTESIAN_POINT('Ctrl Pts',(0.00553346071652693,-0.0371684143765495,
-0.0136467611860309));
#18373=CARTESIAN_POINT('Ctrl Pts',(0.00551491710228931,-0.037167389752226,
-0.0136407503779218));
#18374=CARTESIAN_POINT('Ctrl Pts',(0.00544988287782188,-0.0371637337486952,
-0.013618299661399));
#18375=CARTESIAN_POINT('Ctrl Pts',(0.00540407476868716,-0.0371610432282816,
-0.0135999855898826));
#18376=CARTESIAN_POINT('Ctrl Pts',(0.00528113155401764,-0.0371535134887665,
-0.0135438615638305));
#18377=CARTESIAN_POINT('Ctrl Pts',(0.0052061537061278,-0.0371485647664251,
-0.0135017585197347));
#18378=CARTESIAN_POINT('Ctrl Pts',(0.00507860386490017,-0.0371397378488797,
-0.0134154208772557));
#18379=CARTESIAN_POINT('Ctrl Pts',(0.0050247267537187,-0.0371358618188004,
-0.0133734935581902));
#18380=CARTESIAN_POINT('Ctrl Pts',(0.00496327450046798,-0.0371314099478229,
-0.0133187652591531));
#18381=CARTESIAN_POINT('Ctrl Pts',(0.00495288056979588,-0.0371306559439367,
-0.0133092501564194));
#18382=CARTESIAN_POINT('Ctrl Pts',(0.004936401900974,-0.0371294609968974,
-0.0132937445768664));
#18383=CARTESIAN_POINT('Ctrl Pts',(0.00493023420373071,-0.0371290138551249,
-0.0132878438445751));
#18384=CARTESIAN_POINT('Ctrl Pts',(0.00491840823320606,-0.037128157293777,
-0.0132763402911021));
#18385=CARTESIAN_POINT('Ctrl Pts',(0.00491274408740752,-0.0371277474741468,
-0.0132707445970626));
#18386=CARTESIAN_POINT('Ctrl Pts',(0.00489840297896655,-0.0371267107361774,
-0.0132563557584913));
#18387=CARTESIAN_POINT('Ctrl Pts',(0.00488978794184987,-0.0371260886438505,
-0.013247501920157));
#18388=CARTESIAN_POINT('Ctrl Pts',(0.00485110529340055,-0.0371232932042599,
-0.0132067798143143));
#18389=CARTESIAN_POINT('Ctrl Pts',(0.00482229490831655,-0.0371212048971061,
-0.0131737409864193));
#18390=CARTESIAN_POINT('Ctrl Pts',(0.00472690436993282,-0.0371140883404748,
-0.013054454228842));
#18391=CARTESIAN_POINT('Ctrl Pts',(0.0046680773447329,-0.0371093006658215,
-0.0129624256491001));
#18392=CARTESIAN_POINT('Ctrl Pts',(0.0045941558243124,-0.0371016288004911,
-0.0128143310011492));
#18393=CARTESIAN_POINT('Ctrl Pts',(0.00457168820640274,-0.0370989459360733,
-0.0127623481655958));
#18394=CARTESIAN_POINT('Ctrl Pts',(0.00454519485622604,-0.0370951774976147,
-0.0126904338707258));
#18395=CARTESIAN_POINT('Ctrl Pts',(0.00453862997742936,-0.0370941795294457,
-0.012671482979072));
#18396=CARTESIAN_POINT('Ctrl Pts',(0.00452859850786245,-0.0370925425153628,
-0.012640590923695));
#18397=CARTESIAN_POINT('Ctrl Pts',(0.00452490351678714,-0.0370919113836385,
-0.0126287260891729));
#18398=CARTESIAN_POINT('Ctrl Pts',(0.00451742936429641,-0.0370905726751009,
-0.0126036636878704));
#18399=CARTESIAN_POINT('Ctrl Pts',(0.00451368222439348,-0.0370898640717603,
-0.0125904577755391));
#18400=CARTESIAN_POINT('Ctrl Pts',(0.00450500606134507,-0.0370881275338222,
-0.0125582502453487));
#18401=CARTESIAN_POINT('Ctrl Pts',(0.00450026258437286,-0.0370870934650772,
-0.0125392015287696));
#18402=CARTESIAN_POINT('Ctrl Pts',(0.00448311486713233,-0.0370829972426645,
-0.0124642711175056));
#18403=CARTESIAN_POINT('Ctrl Pts',(0.00447346168928386,-0.0370798466612121,
-0.012407812369097));
#18404=CARTESIAN_POINT('Ctrl Pts',(0.0044603274821594,-0.0370733288368832,
-0.012292819406208));
#18405=CARTESIAN_POINT('Ctrl Pts',(0.00445699999999927,-0.0370699635392117,
-0.0122343585838898));
#18406=CARTESIAN_POINT('Ctrl Pts',(0.004457,-0.0370665921755392,-0.0121758532865387));
#18407=CARTESIAN_POINT('Ctrl Pts',(0.004457,-0.0376822061652104,-0.0121758532865636));
#18408=CARTESIAN_POINT('Ctrl Pts',(0.004457,-0.0376821983899012,-0.0121757169191301));
#18409=CARTESIAN_POINT('Ctrl Pts',(0.00445700001808376,-0.0376821906147461,
-0.0121755805512917));
#18410=CARTESIAN_POINT('Ctrl Pts',(0.00445702249714396,-0.037677356706163,
-0.0120907971419327));
#18411=CARTESIAN_POINT('Ctrl Pts',(0.00446401023444583,-0.0376726175689111,
-0.0120062872456995));
#18412=CARTESIAN_POINT('Ctrl Pts',(0.00448164007563339,-0.0376668620486047,
-0.0119002577688501));
#18413=CARTESIAN_POINT('Ctrl Pts',(0.00448588206624491,-0.0376656549327456,
-0.0118778319706476));
#18414=CARTESIAN_POINT('Ctrl Pts',(0.00449377393537067,-0.0376636697411631,
-0.0118406476637458));
#18415=CARTESIAN_POINT('Ctrl Pts',(0.00449714712307352,-0.0376628832558311,
-0.0118258346883064));
#18416=CARTESIAN_POINT('Ctrl Pts',(0.00450429976257569,-0.0376613304500835,
-0.0117964370098263));
#18417=CARTESIAN_POINT('Ctrl Pts',(0.00450807515227078,-0.0376605641009239,
-0.0117818530576273));
#18418=CARTESIAN_POINT('Ctrl Pts',(0.00451792543255403,-0.0376586876087716,
-0.0117459763727549));
#18419=CARTESIAN_POINT('Ctrl Pts',(0.00452424628365089,-0.0376575853155197,
-0.0117247543909254));
#18420=CARTESIAN_POINT('Ctrl Pts',(0.00455468739899603,-0.0376526918995844,
-0.0116300500309386));
#18421=CARTESIAN_POINT('Ctrl Pts',(0.00458385579798844,-0.0376490619789112,
-0.0115583042819736));
#18422=CARTESIAN_POINT('Ctrl Pts',(0.0046677939372941,-0.0376403489136198,
-0.0113894381773857));
#18423=CARTESIAN_POINT('Ctrl Pts',(0.00472792502657949,-0.0376353593281247,
-0.0112954886199944));
#18424=CARTESIAN_POINT('Ctrl Pts',(0.00480845391318702,-0.0376290346887517,
-0.0111953607431604));
#18425=CARTESIAN_POINT('Ctrl Pts',(0.00481951062290811,-0.0376281722933577,
-0.0111820764051238));
#18426=CARTESIAN_POINT('Ctrl Pts',(0.00483690493349415,-0.0376268198088133,
-0.0111618775733889));
#18427=CARTESIAN_POINT('Ctrl Pts',(0.00484308662687585,-0.0376263399447525,
-0.011154830113861));
#18428=CARTESIAN_POINT('Ctrl Pts',(0.0048548997317603,-0.0376254234627615,
-0.0111416075645628));
#18429=CARTESIAN_POINT('Ctrl Pts',(0.00486051769591762,-0.0376249877471595,
-0.0111354212105127));
#18430=CARTESIAN_POINT('Ctrl Pts',(0.00487448403784089,-0.0376239053912461,
-0.0111202906350169));
#18431=CARTESIAN_POINT('Ctrl Pts',(0.00488288899638949,-0.037623254802692,
-0.0111113995863379));
#18432=CARTESIAN_POINT('Ctrl Pts',(0.00491640107119769,-0.03762066720149,
-0.0110767834602418));
#18433=CARTESIAN_POINT('Ctrl Pts',(0.00494229692903798,-0.0376186817512341,
-0.0110518403848605));
#18434=CARTESIAN_POINT('Ctrl Pts',(0.00502136260936218,-0.0376127202419409,
-0.0109808371149455));
#18435=CARTESIAN_POINT('Ctrl Pts',(0.00507683709268155,-0.0376086672246894,
-0.0109374814912981));
#18436=CARTESIAN_POINT('Ctrl Pts',(0.00520453955408694,-0.0375998600917408,
-0.0108510408065051));
#18437=CARTESIAN_POINT('Ctrl Pts',(0.00527773036734072,-0.037595140243852,
-0.0108097585416849));
#18438=CARTESIAN_POINT('Ctrl Pts',(0.00537762056247263,-0.0375892102211124,
-0.0107637010746876));
#18439=CARTESIAN_POINT('Ctrl Pts',(0.00540159361452585,-0.0375878223017475,
-0.0107533765944144));
#18440=CARTESIAN_POINT('Ctrl Pts',(0.0054405152621558,-0.0375856242761721,
-0.0107377724277635));
#18441=CARTESIAN_POINT('Ctrl Pts',(0.00545530267491293,-0.037584801706765,
-0.0107321065716766));
#18442=CARTESIAN_POINT('Ctrl Pts',(0.0054839684975815,-0.0375832304825638,
-0.0107216262827532));
#18443=CARTESIAN_POINT('Ctrl Pts',(0.00549783352443621,-0.0375824808751488,
-0.0107167804508415));
#18444=CARTESIAN_POINT('Ctrl Pts',(0.00553064378375233,-0.0375807303220066,
-0.0107058363596132));
#18445=CARTESIAN_POINT('Ctrl Pts',(0.00554964217272093,-0.0375797347947286,
-0.0106999051521767));
#18446=CARTESIAN_POINT('Ctrl Pts',(0.00561782267326762,-0.0375762213445696,
-0.010680058646221));
#18447=CARTESIAN_POINT('Ctrl Pts',(0.00566757630504001,-0.0375737676418703,
-0.01066822064498));
#18448=CARTESIAN_POINT('Ctrl Pts',(0.00580955004207624,-0.0375669696125143,
-0.0106418123286862));
#18449=CARTESIAN_POINT('Ctrl Pts',(0.00590262687148162,-0.037562759715691,
-0.0106331054044798));
#18450=CARTESIAN_POINT('Ctrl Pts',(0.00605126616104672,-0.0375558433495857,
-0.0106327123118396));
#18451=CARTESIAN_POINT('Ctrl Pts',(0.00610657660049057,-0.0375532233499259,
-0.0106355439827025));
#18452=CARTESIAN_POINT('Ctrl Pts',(0.00617550388538196,-0.0375497776150157,
-0.0106428032046979));
#18453=CARTESIAN_POINT('Ctrl Pts',(0.00618937631668384,-0.0375490748288729,
-0.0106444549867308));
#18454=CARTESIAN_POINT('Ctrl Pts',(0.00621183366259654,-0.0375479193566133,
-0.010647438769779));
#18455=CARTESIAN_POINT('Ctrl Pts',(0.00622043340817816,-0.0375474726396624,
-0.0106486553481972));
#18456=CARTESIAN_POINT('Ctrl Pts',(0.00623775067485377,-0.037546563721024,
-0.0106512544810376));
#18457=CARTESIAN_POINT('Ctrl Pts',(0.00624646747082618,-0.0375461014259477,
-0.0106526393555384));
#18458=CARTESIAN_POINT('Ctrl Pts',(0.00626959841868577,-0.0375448628265635,
-0.0106565180124865));
#18459=CARTESIAN_POINT('Ctrl Pts',(0.00628398951923239,-0.037544079957627,
-0.0106591420728864));
#18460=CARTESIAN_POINT('Ctrl Pts',(0.0063782115717785,-0.037538883224458,
-0.0106777103935569));
#18461=CARTESIAN_POINT('Ctrl Pts',(0.0064567061052238,-0.0375342242950894,
-0.0106997456356024));
#18462=CARTESIAN_POINT('Ctrl Pts',(0.00663120722308047,-0.0375235783645969,
-0.0107639898541918));
#18463=CARTESIAN_POINT('Ctrl Pts',(0.00672541144264658,-0.0375176315463681,
-0.010809996625809));
#18464=CARTESIAN_POINT('Ctrl Pts',(0.00683606850738029,-0.0375106141710772,
-0.0108787416895683));
#18465=CARTESIAN_POINT('Ctrl Pts',(0.00685755023799678,-0.0375092486823873,
-0.0108928424773348));
#18466=CARTESIAN_POINT('Ctrl Pts',(0.00689162378409269,-0.0375070768518482,
-0.0109164469467425));
#18467=CARTESIAN_POINT('Ctrl Pts',(0.0069044389319358,-0.0375062585871621,
-0.0109256182912334));
#18468=CARTESIAN_POINT('Ctrl Pts',(0.00692895281527635,-0.0375046898991506,
-0.0109437362177048));
#18469=CARTESIAN_POINT('Ctrl Pts',(0.0069406683365693,-0.0375039386284311,
-0.0109526571027446));
#18470=CARTESIAN_POINT('Ctrl Pts',(0.00696809069859235,-0.0375021754063024,
-0.0109741651192625));
#18471=CARTESIAN_POINT('Ctrl Pts',(0.00698368265019711,-0.0375011691044739,
-0.0109868946909788));
#18472=CARTESIAN_POINT('Ctrl Pts',(0.00703939594029263,-0.0374975542438987,
-0.0110342265121515));
#18473=CARTESIAN_POINT('Ctrl Pts',(0.00707797878024858,-0.037495015271026,
-0.0110705849951919));
#18474=CARTESIAN_POINT('Ctrl Pts',(0.00718464362119928,-0.0374877673061877,
-0.0111820105473435));
#18475=CARTESIAN_POINT('Ctrl Pts',(0.00724729560961758,-0.0374832203713592,
-0.011261874868321));
#18476=CARTESIAN_POINT('Ctrl Pts',(0.00731674825861279,-0.0374771541419818,
-0.0113709859433026));
#18477=CARTESIAN_POINT('Ctrl Pts',(0.00733117597733396,-0.0374758215376672,
-0.0113950794274066));
#18478=CARTESIAN_POINT('Ctrl Pts',(0.00735686320852034,-0.0374732838909979,
-0.0114407592847954));
#18479=CARTESIAN_POINT('Ctrl Pts',(0.0073682848189581,-0.0374720859029069,
-0.0114622445013686));
#18480=CARTESIAN_POINT('Ctrl Pts',(0.00738392524632726,-0.0374703287901045,
-0.0114934228576332));
#18481=CARTESIAN_POINT('Ctrl Pts',(0.00738856031706123,-0.0374697920364909,
-0.0115029040968448));
#18482=CARTESIAN_POINT('Ctrl Pts',(0.00739661936599757,-0.0374688284443794,
-0.0115198270390851));
#18483=CARTESIAN_POINT('Ctrl Pts',(0.00740008191421842,-0.03746840386379,
-0.0115272496174671));
#18484=CARTESIAN_POINT('Ctrl Pts',(0.00740776482080798,-0.0374674373186778,
-0.0115440674999729));
#18485=CARTESIAN_POINT('Ctrl Pts',(0.00741195032133339,-0.0374668934620033,
-0.0115534777169207));
#18486=CARTESIAN_POINT('Ctrl Pts',(0.0074248586077519,-0.0374651620118918,
-0.0115832997715091));
#18487=CARTESIAN_POINT('Ctrl Pts',(0.00743323501150416,-0.0374639568670845,
-0.0116038576320402));
#18488=CARTESIAN_POINT('Ctrl Pts',(0.00745271016618792,-0.0374609563357964,
-0.0116547712388972));
#18489=CARTESIAN_POINT('Ctrl Pts',(0.00746330411812472,-0.0374591431795591,
-0.0116853084856268));
#18490=CARTESIAN_POINT('Ctrl Pts',(0.00751547155275493,-0.0374492220565311,
-0.0118524592544573));
#18491=CARTESIAN_POINT('Ctrl Pts',(0.00753889408427512,-0.0374409174894126,
-0.0119940415693968));
#18492=CARTESIAN_POINT('Ctrl Pts',(0.00754313739746618,-0.0374318924433555,
-0.0121617693645397));
#18493=CARTESIAN_POINT('Ctrl Pts',(0.00754316342641352,-0.0374305679844783,
-0.0121867215180258));
#18494=CARTESIAN_POINT('Ctrl Pts',(0.00754222236655664,-0.0374284450963234,
-0.0122272582957389));
#18495=CARTESIAN_POINT('Ctrl Pts',(0.00754162390736574,-0.0374276356721985,
-0.0122428462296096));
#18496=CARTESIAN_POINT('Ctrl Pts',(0.00753999875788756,-0.03742607376452,
-0.0122731723482762));
#18497=CARTESIAN_POINT('Ctrl Pts',(0.00753899657698308,-0.0374253206209278,
-0.0122879100999666));
#18498=CARTESIAN_POINT('Ctrl Pts',(0.0075360979178634,-0.0374235369610373,
-0.0123230699858119));
#18499=CARTESIAN_POINT('Ctrl Pts',(0.00753400558251348,-0.0374225125152147,
-0.0123434733669885));
#18500=CARTESIAN_POINT('Ctrl Pts',(0.00752461595810618,-0.0374187055939707,
-0.0124199738385339));
#18501=CARTESIAN_POINT('Ctrl Pts',(0.00751464249878353,-0.037416003759487,
-0.0124756990944652));
#18502=CARTESIAN_POINT('Ctrl Pts',(0.00747376146849427,-0.0374076804308529,
-0.0126486717499723));
#18503=CARTESIAN_POINT('Ctrl Pts',(0.00743210339603019,-0.0374023040266418,
-0.0127628844676466));
#18504=CARTESIAN_POINT('Ctrl Pts',(0.00736568852945161,-0.0373952023856881,
-0.0128944864390118));
#18505=CARTESIAN_POINT('Ctrl Pts',(0.00735325962921836,-0.0373939152317161,
-0.0129176261662842));
#18506=CARTESIAN_POINT('Ctrl Pts',(0.00733517308707057,-0.0373920824533119,
-0.0129493302906303));
#18507=CARTESIAN_POINT('Ctrl Pts',(0.00733001093581626,-0.0373915635584854,
-0.012958173392676));
#18508=CARTESIAN_POINT('Ctrl Pts',(0.00732048177057484,-0.0373906120126245,
-0.0129741305338813));
#18509=CARTESIAN_POINT('Ctrl Pts',(0.00731614425601137,-0.0373901811349147,
-0.0129812618575723));
#18510=CARTESIAN_POINT('Ctrl Pts',(0.00730680647957924,-0.0373892576755227,
-0.0129963372455667));
#18511=CARTESIAN_POINT('Ctrl Pts',(0.00730179132230508,-0.0373887642369093,
-0.0130042713250668));
#18512=CARTESIAN_POINT('Ctrl Pts',(0.00728730396493611,-0.0373873470726835,
-0.0130267341853457));
#18513=CARTESIAN_POINT('Ctrl Pts',(0.00727765900021106,-0.0373864133406789,
-0.0130411493247408));
#18514=CARTESIAN_POINT('Ctrl Pts',(0.00723122073545717,-0.0373819735987214,
-0.0131080853029943));
#18515=CARTESIAN_POINT('Ctrl Pts',(0.00719142141032065,-0.0373783299592346,
-0.0131584391388518));
#18516=CARTESIAN_POINT('Ctrl Pts',(0.00706774521995361,-0.0373677370707179,
-0.0132963150729106));
#18517=CARTESIAN_POINT('Ctrl Pts',(0.00697653680228718,-0.0373608008922294,
-0.0133766441056771));
#18518=CARTESIAN_POINT('Ctrl Pts',(0.00685730558447382,-0.0373530255358731,
-0.0134589904842994));
#18519=CARTESIAN_POINT('Ctrl Pts',(0.00683743810418692,-0.0373517661400594,
-0.0134720444133268));
#18520=CARTESIAN_POINT('Ctrl Pts',(0.00680423192873222,-0.0373497191905715,
-0.013492780205002));
#18521=CARTESIAN_POINT('Ctrl Pts',(0.00679106630928515,-0.0373489221165044,
-0.0135007304960838));
#18522=CARTESIAN_POINT('Ctrl Pts',(0.00676489082328246,-0.0373473650747437,
-0.0135160077100935));
#18523=CARTESIAN_POINT('Ctrl Pts',(0.00675188913838051,-0.0373466047880497,
-0.0135233452508863));
#18524=CARTESIAN_POINT('Ctrl Pts',(0.00672002868750576,-0.0373447722573444,
-0.0135407210505973));
#18525=CARTESIAN_POINT('Ctrl Pts',(0.00670106376593467,-0.0373437069874764,
-0.0135505587004084));
#18526=CARTESIAN_POINT('Ctrl Pts',(0.00662301489153961,-0.0373394185038155,
-0.0135890094989001));
#18527=CARTESIAN_POINT('Ctrl Pts',(0.00656233541584108,-0.0373363073012548,
-0.0136142336127846));
#18528=CARTESIAN_POINT('Ctrl Pts',(0.00644484741048625,-0.0373305308797699,
-0.0136544970020777));
#18529=CARTESIAN_POINT('Ctrl Pts',(0.00638842912809595,-0.0373278576209602,
-0.0136703094792597));
#18530=CARTESIAN_POINT('Ctrl Pts',(0.0062670691292105,-0.0373221238971621,
-0.0136969848319452));
#18531=CARTESIAN_POINT('Ctrl Pts',(0.00620205808420158,-0.0373190617216438,
-0.0137069764978541));
#18532=CARTESIAN_POINT('Ctrl Pts',(0.00611926892202126,-0.0373149718629774,
-0.0137143353811948));
#18533=CARTESIAN_POINT('Ctrl Pts',(0.00610189956618336,-0.037314103176606,
-0.0137155833485041));
#18534=CARTESIAN_POINT('Ctrl Pts',(0.00607511974164655,-0.0373127425987683,
-0.0137170523432732));
#18535=CARTESIAN_POINT('Ctrl Pts',(0.00606572170632952,-0.0373122610971433,
-0.0137174816972722));
#18536=CARTESIAN_POINT('Ctrl Pts',(0.0060479464523563,-0.0373113418328254,
-0.0137181309389245));
#18537=CARTESIAN_POINT('Ctrl Pts',(0.00603957043463689,-0.0373109049846501,
-0.0137183685663306));
#18538=CARTESIAN_POINT('Ctrl Pts',(0.00601894482892701,-0.0373098207476937,
-0.0137187856169297));
#18539=CARTESIAN_POINT('Ctrl Pts',(0.00600669435854373,-0.0373091694244024,
-0.0137188873918589));
#18540=CARTESIAN_POINT('Ctrl Pts',(0.00595857730818526,-0.0373065857307427,
-0.0137187141429715));
#18541=CARTESIAN_POINT('Ctrl Pts',(0.0059227278460709,-0.0373046054110942,
-0.0137173344404372));
#18542=CARTESIAN_POINT('Ctrl Pts',(0.00581708100760184,-0.0372986657796179,
-0.0137095740159387));
#18543=CARTESIAN_POINT('Ctrl Pts',(0.00574763281794559,-0.0372946305970241,
-0.0136996869745772));
#18544=CARTESIAN_POINT('Ctrl Pts',(0.00559739634266737,-0.0372858643966202,
-0.0136677434628822));
#18545=CARTESIAN_POINT('Ctrl Pts',(0.00551723213865605,-0.0372811671372832,
-0.0136437647250388));
#18546=CARTESIAN_POINT('Ctrl Pts',(0.00541510911312887,-0.037275259126433,
-0.0136039398422354));
#18547=CARTESIAN_POINT('Ctrl Pts',(0.00539106518799816,-0.0372738729400698,
-0.0135938543663173));
#18548=CARTESIAN_POINT('Ctrl Pts',(0.00535282918037681,-0.0372716757105772,
-0.0135766638455378));
#18549=CARTESIAN_POINT('Ctrl Pts',(0.00533847170844655,-0.0372708522986791,
-0.0135699410297759));
#18550=CARTESIAN_POINT('Ctrl Pts',(0.00531097887850482,-0.037269278111746,
-0.013556547254839));
#18551=CARTESIAN_POINT('Ctrl Pts',(0.00529783049928252,-0.0372685264072893,
-0.0135499071251397));
#18552=CARTESIAN_POINT('Ctrl Pts',(0.00526705488752359,-0.0372667687060703,
-0.0135338078397885));
#18553=CARTESIAN_POINT('Ctrl Pts',(0.00524951236730342,-0.0372657682020693,
-0.0135241920663343));
#18554=CARTESIAN_POINT('Ctrl Pts',(0.00518729557183864,-0.0372622198401728,
-0.0134884979353156));
#18555=CARTESIAN_POINT('Ctrl Pts',(0.00514375059639078,-0.037259737839284,
-0.0134605174517959));
#18556=CARTESIAN_POINT('Ctrl Pts',(0.00502393807064255,-0.037252804737251,
-0.013374726582427));
#18557=CARTESIAN_POINT('Ctrl Pts',(0.00495153203669132,-0.0372484957539897,
-0.013311946826388));
#18558=CARTESIAN_POINT('Ctrl Pts',(0.00484903587818129,-0.0372415848914354,
-0.0132048802117191));
#18559=CARTESIAN_POINT('Ctrl Pts',(0.00481463671439681,-0.0372390885589735,
-0.0131650589568449));
#18560=CARTESIAN_POINT('Ctrl Pts',(0.00477381281581633,-0.0372357831137204,
-0.0131126065887554));
#18561=CARTESIAN_POINT('Ctrl Pts',(0.00476543393386964,-0.0372350845052494,
-0.0131015359337883));
#18562=CARTESIAN_POINT('Ctrl Pts',(0.00475206850752643,-0.0372339341367546,
-0.0130833725012001));
#18563=CARTESIAN_POINT('Ctrl Pts',(0.00474699020064702,-0.037233488247222,
-0.0130763479121047));
#18564=CARTESIAN_POINT('Ctrl Pts',(0.00473689282366637,-0.0372325829688868,
-0.0130621298761833));
#18565=CARTESIAN_POINT('Ctrl Pts',(0.00473187537859859,-0.0372321234929344,
-0.0130549356882221));
#18566=CARTESIAN_POINT('Ctrl Pts',(0.0047186854282799,-0.0372308905180822,
-0.0130356755597257));
#18567=CARTESIAN_POINT('Ctrl Pts',(0.00471062222018163,-0.0372301104296057,
-0.01302353617799));
#18568=CARTESIAN_POINT('Ctrl Pts',(0.00469288009207113,-0.0372283367042366,
-0.0129959860014368));
#18569=CARTESIAN_POINT('Ctrl Pts',(0.0046832994779795,-0.0372273383517275,
-0.0129805145893346));
#18570=CARTESIAN_POINT('Ctrl Pts',(0.00465298141416091,-0.0372240519919394,
-0.0129295632001459));
#18571=CARTESIAN_POINT('Ctrl Pts',(0.00463338781477493,-0.0372217237235393,
-0.0128934245661015));
#18572=CARTESIAN_POINT('Ctrl Pts',(0.00459310040674032,-0.0372165105822372,
-0.0128114678809438));
#18573=CARTESIAN_POINT('Ctrl Pts',(0.00457315459911803,-0.037213620658179,
-0.0127653315629158));
#18574=CARTESIAN_POINT('Ctrl Pts',(0.00452846728969945,-0.0372063716407419,
-0.0126463326953032));
#18575=CARTESIAN_POINT('Ctrl Pts',(0.00450685428702723,-0.0372020612084549,
-0.0125724356020587));
#18576=CARTESIAN_POINT('Ctrl Pts',(0.00448544923810147,-0.0371965216288206,
-0.0124719185092907));
#18577=CARTESIAN_POINT('Ctrl Pts',(0.00448069691119912,-0.0371951456067359,
-0.0124464763769168));
#18578=CARTESIAN_POINT('Ctrl Pts',(0.00447408887733859,-0.0371929650938438,
-0.0124053996684703));
#18579=CARTESIAN_POINT('Ctrl Pts',(0.00447182863826404,-0.037192148287569,
-0.0123898360169502));
#18580=CARTESIAN_POINT('Ctrl Pts',(0.00446802693702081,-0.0371906263218655,
-0.0123605128143969));
#18581=CARTESIAN_POINT('Ctrl Pts',(0.00446643197969306,-0.0371899195791157,
-0.0123467618879886));
#18582=CARTESIAN_POINT('Ctrl Pts',(0.00446357384110298,-0.0371884980686156,
-0.0123188425726348));
#18583=CARTESIAN_POINT('Ctrl Pts',(0.0044623210995899,-0.0371877836829529,
-0.0123046744556103));
#18584=CARTESIAN_POINT('Ctrl Pts',(0.00446001899905396,-0.0371862397752352,
-0.0122737742227515));
#18585=CARTESIAN_POINT('Ctrl Pts',(0.00445904606366526,-0.037185412584469,
-0.0122570381653969));
#18586=CARTESIAN_POINT('Ctrl Pts',(0.00445744878958926,-0.03718354204134,
-0.0122188227597701));
#18587=CARTESIAN_POINT('Ctrl Pts',(0.004457,-0.0371825036589017,-0.0121973394742422));
#18588=CARTESIAN_POINT('Ctrl Pts',(0.004457,-0.0371814756795928,-0.0121758532865595));
#18589=CARTESIAN_POINT('Origin',(0.006,-0.0418165664398416,-0.0121758532865581));
#18590=CARTESIAN_POINT('',(0.004457,-0.0381835089768636,-0.0121758532865622));
#18591=CARTESIAN_POINT('',(0.004457,-0.0380657947427934,-0.0121758532821831));
#18592=CARTESIAN_POINT('',(0.004457,-0.0418165664398416,-0.0121758532865581));
#18593=CARTESIAN_POINT('Ctrl Pts',(0.004457,-0.037567972222619,-0.0121758532865581));
#18594=CARTESIAN_POINT('Ctrl Pts',(0.004457,-0.037568678241124,-0.0121898344068753));
#18595=CARTESIAN_POINT('Ctrl Pts',(0.00445719002408502,-0.0375693784287243,
-0.0122038151522925));
#18596=CARTESIAN_POINT('Ctrl Pts',(0.00445808151027365,-0.0375710079749599,
-0.0122366026512338));
#18597=CARTESIAN_POINT('Ctrl Pts',(0.0044589370642531,-0.0375719326749006,
-0.0122554031334834));
#18598=CARTESIAN_POINT('Ctrl Pts',(0.00446679404094303,-0.0375779304842151,
-0.0123784440671839));
#18599=CARTESIAN_POINT('Ctrl Pts',(0.00448402264997262,-0.0375826887137011,
-0.0124817582632797));
#18600=CARTESIAN_POINT('Ctrl Pts',(0.00452632927009839,-0.0375900513271768,
-0.0126365952903472));
#18601=CARTESIAN_POINT('Ctrl Pts',(0.00454403035407989,-0.0375926311243432,
-0.0126897992095187));
#18602=CARTESIAN_POINT('Ctrl Pts',(0.00457617451843771,-0.0375968131917808,
-0.0127713094850159));
#18603=CARTESIAN_POINT('Ctrl Pts',(0.00458866380320455,-0.0375983503945804,
-0.0128003346652087));
#18604=CARTESIAN_POINT('Ctrl Pts',(0.00460691311778797,-0.0376005113407886,
-0.012839397407423));
#18605=CARTESIAN_POINT('Ctrl Pts',(0.00461190866022404,-0.0376010951177554,
-0.0128497852408629));
#18606=CARTESIAN_POINT('Ctrl Pts',(0.00462059548986302,-0.0376020989756306,
-0.012867342408065));
#18607=CARTESIAN_POINT('Ctrl Pts',(0.00462422751550074,-0.0376025155503683,
-0.0128745406826348));
#18608=CARTESIAN_POINT('Ctrl Pts',(0.00463213180611988,-0.037603415976494,
-0.0128899054837215));
#18609=CARTESIAN_POINT('Ctrl Pts',(0.00463642100623976,-0.0376039007819443,
-0.0128980625744427));
#18610=CARTESIAN_POINT('Ctrl Pts',(0.00464872682046266,-0.037605280089016,
-0.0129209650098798));
#18611=CARTESIAN_POINT('Ctrl Pts',(0.00465691111621596,-0.037606184003529,
-0.0129356183108848));
#18612=CARTESIAN_POINT('Ctrl Pts',(0.00470799010563829,-0.0376117329409057,
-0.0130236657262171));
#18613=CARTESIAN_POINT('Ctrl Pts',(0.00475664874101791,-0.0376166304450483,
-0.0130935413668386));
#18614=CARTESIAN_POINT('Ctrl Pts',(0.00485525609258224,-0.0376255100341241,
-0.0132128083728953));
#18615=CARTESIAN_POINT('Ctrl Pts',(0.00490329946283619,-0.0376294899279881,
-0.0132634946130268));
#18616=CARTESIAN_POINT('Ctrl Pts',(0.00498686227427952,-0.0376357837459509,
-0.0133404663845039));
#18617=CARTESIAN_POINT('Ctrl Pts',(0.00502036739842618,-0.037638165803492,
-0.0133687875613264));
#18618=CARTESIAN_POINT('Ctrl Pts',(0.00506975900280824,-0.0376414793398714,
-0.0134070508966981));
#18619=CARTESIAN_POINT('Ctrl Pts',(0.00508468789446661,-0.0376424567849377,
-0.013418189657265));
#18620=CARTESIAN_POINT('Ctrl Pts',(0.00511132004003647,-0.0376441593126957,
-0.0134373197278642));
#18621=CARTESIAN_POINT('Ctrl Pts',(0.00512293833039767,-0.0376448887004029,
-0.0134454250644067));
#18622=CARTESIAN_POINT('Ctrl Pts',(0.00514762669966909,-0.0376464114394628,
-0.0134621478777868));
#18623=CARTESIAN_POINT('Ctrl Pts',(0.00516071966444018,-0.0376472033733367,
-0.0134707287863118));
#18624=CARTESIAN_POINT('Ctrl Pts',(0.00519647241119483,-0.0376493256235521,
-0.0134933903903574));
#18625=CARTESIAN_POINT('Ctrl Pts',(0.00521937086139691,-0.0376506419506198,
-0.0135070853690383));
#18626=CARTESIAN_POINT('Ctrl Pts',(0.00535590594848493,-0.0376582659327228,
-0.0135840084654818));
#18627=CARTESIAN_POINT('Ctrl Pts',(0.00547680491045863,-0.0376640665963067,
-0.0136332567900804));
#18628=CARTESIAN_POINT('Ctrl Pts',(0.00565787736508249,-0.0376727574647282,
-0.0136815397652588));
#18629=CARTESIAN_POINT('Ctrl Pts',(0.00571408179197582,-0.0376754648397836,
-0.013693215920058));
#18630=CARTESIAN_POINT('Ctrl Pts',(0.00578433075752823,-0.0376789966041887,
-0.0137037678715674));
#18631=CARTESIAN_POINT('Ctrl Pts',(0.00579788711941135,-0.0376796849322712,
-0.013705620118642));
#18632=CARTESIAN_POINT('Ctrl Pts',(0.00581987325141321,-0.0376808147744672,
-0.0137083268131556));
#18633=CARTESIAN_POINT('Ctrl Pts',(0.00582828882786665,-0.0376812504303419,
-0.0137092925655745));
#18634=CARTESIAN_POINT('Ctrl Pts',(0.00584517407129322,-0.0376821316745481,
-0.0137110895399734));
#18635=CARTESIAN_POINT('Ctrl Pts',(0.00585364350714671,-0.0376825772795396,
-0.0137119200794625));
#18636=CARTESIAN_POINT('Ctrl Pts',(0.00587594096430578,-0.037683759055172,
-0.0137139205591896));
#18637=CARTESIAN_POINT('Ctrl Pts',(0.00588977838890079,-0.0376845011630794,
-0.0137149740582421));
#18638=CARTESIAN_POINT('Ctrl Pts',(0.00596114800471843,-0.0376883670961703,
-0.01371944036544));
#18639=CARTESIAN_POINT('Ctrl Pts',(0.00601882061328578,-0.0376916178401928,
-0.0137198141964576));
#18640=CARTESIAN_POINT('Ctrl Pts',(0.00616936667675947,-0.03770022391967,
-0.0137123534780442));
#18641=CARTESIAN_POINT('Ctrl Pts',(0.00626175900387458,-0.0377056145604786,
-0.0136993368656634));
#18642=CARTESIAN_POINT('Ctrl Pts',(0.00640207921997938,-0.0377136612537982,
-0.0136664181094068));
#18643=CARTESIAN_POINT('Ctrl Pts',(0.00645113740171161,-0.037716450143879,
-0.0136523108727218));
#18644=CARTESIAN_POINT('Ctrl Pts',(0.00651792114498997,-0.0377202034757736,
-0.0136294658315586));
#18645=CARTESIAN_POINT('Ctrl Pts',(0.00653631033396669,-0.0377212325065626,
-0.013622782108565));
#18646=CARTESIAN_POINT('Ctrl Pts',(0.00656790670424053,-0.0377229934939561,
-0.0136106129485017));
#18647=CARTESIAN_POINT('Ctrl Pts',(0.00658117363117577,-0.0377237307151269,
-0.0136052904278226));
#18648=CARTESIAN_POINT('Ctrl Pts',(0.00660843786701875,-0.0377252417939346,
-0.0135939100251527));
#18649=CARTESIAN_POINT('Ctrl Pts',(0.00662242319405501,-0.037726014720564,
-0.0135878274154827));
#18650=CARTESIAN_POINT('Ctrl Pts',(0.00665879454150574,-0.037728020425607,
-0.0135713630699997));
#18651=CARTESIAN_POINT('Ctrl Pts',(0.0066810260937949,-0.0377292418776456,
-0.0135606497865872));
#18652=CARTESIAN_POINT('Ctrl Pts',(0.00680436302976774,-0.0377360095945636,
-0.0134975253247468));
#18653=CARTESIAN_POINT('Ctrl Pts',(0.00689967779314488,-0.0377411731969113,
-0.0134345821810689));
#18654=CARTESIAN_POINT('Ctrl Pts',(0.00702720726955131,-0.0377487958333585,
-0.0133284172286406));
#18655=CARTESIAN_POINT('Ctrl Pts',(0.00706549906044883,-0.0377512020427642,
-0.0132931131728694));
#18656=CARTESIAN_POINT('Ctrl Pts',(0.0071230947291257,-0.0377551384070272,
-0.0132343528247423));
#18657=CARTESIAN_POINT('Ctrl Pts',(0.00714361742761331,-0.0377566124091082,
-0.0132121457233357));
#18658=CARTESIAN_POINT('Ctrl Pts',(0.00717093292913957,-0.0377586983546337,
-0.0131807881359926));
#18659=CARTESIAN_POINT('Ctrl Pts',(0.00717829748583572,-0.0377592739099808,
-0.0131721429013325));
#18660=CARTESIAN_POINT('Ctrl Pts',(0.00719071304813249,-0.0377602685109808,
-0.0131572380816037));
#18661=CARTESIAN_POINT('Ctrl Pts',(0.00719581184136165,-0.0377606842327645,
-0.0131510187687202));
#18662=CARTESIAN_POINT('Ctrl Pts',(0.00720670626839883,-0.0377615887549717,
-0.0131375162254816));
#18663=CARTESIAN_POINT('Ctrl Pts',(0.00721248487748851,-0.0377620786132465,
-0.0131302201130723));
#18664=CARTESIAN_POINT('Ctrl Pts',(0.00722876540335598,-0.0377634866814276,
-0.0131092776757534));
#18665=CARTESIAN_POINT('Ctrl Pts',(0.00723910510481083,-0.0377644148962775,
-0.0130955075687727));
#18666=CARTESIAN_POINT('Ctrl Pts',(0.00728944283900557,-0.0377690947268764,
-0.0130260789757216));
#18667=CARTESIAN_POINT('Ctrl Pts',(0.00732592942432527,-0.0377730072835353,
-0.0129679747726239));
#18668=CARTESIAN_POINT('Ctrl Pts',(0.00738778435969847,-0.0377804887130888,
-0.0128531526162443));
#18669=CARTESIAN_POINT('Ctrl Pts',(0.00741383416331627,-0.0377840476500943,
-0.0127969437031496));
#18670=CARTESIAN_POINT('Ctrl Pts',(0.0074517506613499,-0.0377899019115409,
-0.0127002838079475));
#18671=CARTESIAN_POINT('Ctrl Pts',(0.00746546659798519,-0.0377922329370755,
-0.012660637141102));
#18672=CARTESIAN_POINT('Ctrl Pts',(0.00748662659889514,-0.0377962329342473,
-0.0125903195624184));
#18673=CARTESIAN_POINT('Ctrl Pts',(0.0074947769795301,-0.0377979214700999,
-0.0125598883254413));
#18674=CARTESIAN_POINT('Ctrl Pts',(0.00750578805759868,-0.037800454140006,
-0.012513086548362));
#18675=CARTESIAN_POINT('Ctrl Pts',(0.00750932518532635,-0.0378013193517727,
-0.0124968851553233));
#18676=CARTESIAN_POINT('Ctrl Pts',(0.00751537314918192,-0.0378029017227214,
-0.0124668691815798));
#18677=CARTESIAN_POINT('Ctrl Pts',(0.00751795788826667,-0.0378036211484498,
-0.0124530714297225));
#18678=CARTESIAN_POINT('Ctrl Pts',(0.00752328746026531,-0.037805208272874,
-0.0124223074036548));
#18679=CARTESIAN_POINT('Ctrl Pts',(0.00752593786390774,-0.037806072928249,
-0.0124053265614354));
#18680=CARTESIAN_POINT('Ctrl Pts',(0.00753309967034735,-0.0378086643837219,
-0.0123538068922219));
#18681=CARTESIAN_POINT('Ctrl Pts',(0.00753672599787411,-0.0378103639239807,
-0.0123191554455367));
#18682=CARTESIAN_POINT('Ctrl Pts',(0.00754754436034415,-0.0378177399914758,
-0.012165765757112));
#18683=CARTESIAN_POINT('Ctrl Pts',(0.00754216658919725,-0.0378230494984337,
-0.012046558670885));
#18684=CARTESIAN_POINT('Ctrl Pts',(0.00751432616600706,-0.037831137355823,
-0.0118746698541655));
#18685=CARTESIAN_POINT('Ctrl Pts',(0.00750258559480269,-0.0378337480307295,
-0.01182070438724));
#18686=CARTESIAN_POINT('Ctrl Pts',(0.00748439078673871,-0.0378371672791377,
-0.0117544069527176));
#18687=CARTESIAN_POINT('Ctrl Pts',(0.00748062837626584,-0.0378378499389566,
-0.0117413735887382));
#18688=CARTESIAN_POINT('Ctrl Pts',(0.00747424637304036,-0.0378389726259518,
-0.0117203119464514));
#18689=CARTESIAN_POINT('Ctrl Pts',(0.00747173177866306,-0.0378394069231991,
-0.0117122523297544));
#18690=CARTESIAN_POINT('Ctrl Pts',(0.00746654316091263,-0.0378402880226924,
-0.0116960898452881));
#18691=CARTESIAN_POINT('Ctrl Pts',(0.00746386782332745,-0.0378407348793186,
-0.0116879877400799));
#18692=CARTESIAN_POINT('Ctrl Pts',(0.00745663037210988,-0.0378419237712366,
-0.0116666651588377));
#18693=CARTESIAN_POINT('Ctrl Pts',(0.00745195556074729,-0.0378426718672093,
-0.0116534840557328));
#18694=CARTESIAN_POINT('Ctrl Pts',(0.00742613923800333,-0.0378466948643999,
-0.0115837175882531));
#18695=CARTESIAN_POINT('Ctrl Pts',(0.00740186903369166,-0.0378501091495675,
-0.0115283504884533));
#18696=CARTESIAN_POINT('Ctrl Pts',(0.00733311134558308,-0.0378587566253638,
-0.0113935980992907));
#18697=CARTESIAN_POINT('Ctrl Pts',(0.00728472869940064,-0.0378640122185914,
-0.0113164446414694));
#18698=CARTESIAN_POINT('Ctrl Pts',(0.00719937268103303,-0.0378718984062556,
-0.0112037944775888));
#18699=CARTESIAN_POINT('Ctrl Pts',(0.00716695606857058,-0.0378746546885683,
-0.0111651073072806));
#18700=CARTESIAN_POINT('Ctrl Pts',(0.00711946181833625,-0.0378783732253046,
-0.011113763700785));
#18701=CARTESIAN_POINT('Ctrl Pts',(0.00710595335127584,-0.0378793984694344,
-0.0110997044668799));
#18702=CARTESIAN_POINT('Ctrl Pts',(0.00708209203673046,-0.0378811551263349,
-0.0110757942689379));
#18703=CARTESIAN_POINT('Ctrl Pts',(0.00707186231035027,-0.037881891732357,
-0.0110658243572278));
#18704=CARTESIAN_POINT('Ctrl Pts',(0.00705040906936235,-0.0378834034353072,
-0.0110454891313197));
#18705=CARTESIAN_POINT('Ctrl Pts',(0.00703916707260944,-0.037884177568683,
-0.0110351455443623));
#18706=CARTESIAN_POINT('Ctrl Pts',(0.00700927458838185,-0.0378861906770952,
-0.0110084506570932));
#18707=CARTESIAN_POINT('Ctrl Pts',(0.00699037993875028,-0.037887418163699,
-0.0109923788442991));
#18708=CARTESIAN_POINT('Ctrl Pts',(0.00688347468550523,-0.0378941360026634,
-0.0109057992266374));
#18709=CARTESIAN_POINT('Ctrl Pts',(0.00678833009440698,-0.0378992528980613,
-0.0108446499911663));
#18710=CARTESIAN_POINT('Ctrl Pts',(0.00664026164079196,-0.0379068487433321,
-0.0107709753005912));
#18711=CARTESIAN_POINT('Ctrl Pts',(0.00659199170693112,-0.0379092795551161,
-0.0107499632422185));
#18712=CARTESIAN_POINT('Ctrl Pts',(0.00652311060910942,-0.0379127987398857,
-0.0107240804873457));
#18713=CARTESIAN_POINT('Ctrl Pts',(0.00650332788175168,-0.037913815203053,
-0.0107171038395648));
#18714=CARTESIAN_POINT('Ctrl Pts',(0.00646806335569633,-0.0379156470032412,
-0.01070547005692));
#18715=CARTESIAN_POINT('Ctrl Pts',(0.00645263883063274,-0.0379164548427084,
-0.0107006488269146));
#18716=CARTESIAN_POINT('Ctrl Pts',(0.00642852017037536,-0.0379177322749562,
-0.0106935239416549));
#18717=CARTESIAN_POINT('Ctrl Pts',(0.00641987644180926,-0.037918192906761,
-0.0106910524281609));
#18718=CARTESIAN_POINT('Ctrl Pts',(0.00640344627989107,-0.0379190746638328,
-0.0106865094668853));
#18719=CARTESIAN_POINT('Ctrl Pts',(0.0063956644367984,-0.0379194949737761,
-0.0106844232490246));
#18720=CARTESIAN_POINT('Ctrl Pts',(0.00637814733779928,-0.0379204466583869,
-0.0106798738642972));
#18721=CARTESIAN_POINT('Ctrl Pts',(0.00636840365671405,-0.0379209798323623,
-0.0106774446052178));
#18722=CARTESIAN_POINT('Ctrl Pts',(0.00633315130660186,-0.0379229208119484,
-0.0106690202394396));
#18723=CARTESIAN_POINT('Ctrl Pts',(0.0063075157062571,-0.0379243547835765,
-0.0106635803057966));
#18724=CARTESIAN_POINT('Ctrl Pts',(0.00616290266057789,-0.0379325234067393,
-0.0106367220447446));
#18725=CARTESIAN_POINT('Ctrl Pts',(0.00604186737402234,-0.0379396201874804,
-0.0106286908510281));
#18726=CARTESIAN_POINT('Ctrl Pts',(0.00586260049968923,-0.0379497116860012,
-0.010637865913351));
#18727=CARTESIAN_POINT('Ctrl Pts',(0.00580428414016355,-0.037952935505009,
-0.0106441939824192));
#18728=CARTESIAN_POINT('Ctrl Pts',(0.00572634702991176,-0.0379571461978135,
-0.0106571765669704));
#18729=CARTESIAN_POINT('Ctrl Pts',(0.00570629776553585,-0.0379582208390945,
-0.010660926233141));
#18730=CARTESIAN_POINT('Ctrl Pts',(0.00567219953469682,-0.0379600345408175,
-0.0106680057892819));
#18731=CARTESIAN_POINT('Ctrl Pts',(0.00565811255163312,-0.0379607797348449,
-0.0106711372962689));
#18732=CARTESIAN_POINT('Ctrl Pts',(0.00563122001510145,-0.0379621950272905,
-0.0106775126181763));
#18733=CARTESIAN_POINT('Ctrl Pts',(0.00561840818961115,-0.0379628660787223,
-0.0106807241483264));
#18734=CARTESIAN_POINT('Ctrl Pts',(0.00558462877119288,-0.0379646276962723,
-0.0106896541013495));
#18735=CARTESIAN_POINT('Ctrl Pts',(0.00556373772068329,-0.0379657092751702,
-0.0106956517604971));
#18736=CARTESIAN_POINT('Ctrl Pts',(0.00547676146541318,-0.0379701870165771,
-0.0107226234519438));
#18737=CARTESIAN_POINT('Ctrl Pts',(0.00541199893961501,-0.0379734549048751,
-0.0107475985945882));
#18738=CARTESIAN_POINT('Ctrl Pts',(0.00527735885934287,-0.0379803258465395,
-0.0108102379914169));
#18739=CARTESIAN_POINT('Ctrl Pts',(0.00520826405311605,-0.0379838999420277,
-0.0108491019970386));
#18740=CARTESIAN_POINT('Ctrl Pts',(0.00510125736816331,-0.037989907623262,
-0.0109206374574219));
#18741=CARTESIAN_POINT('Ctrl Pts',(0.00506141083126633,-0.0379922662657697,
-0.0109501474828508));
#18742=CARTESIAN_POINT('Ctrl Pts',(0.00501282020636505,-0.0379953922100594,
-0.0109898937837802));
#18743=CARTESIAN_POINT('Ctrl Pts',(0.00500269240355866,-0.037996058371806,
-0.0109983977998296));
#18744=CARTESIAN_POINT('Ctrl Pts',(0.00498633318825823,-0.0379971608383284,
-0.0110124966360593));
#18745=CARTESIAN_POINT('Ctrl Pts',(0.00498003558507807,-0.0379975918025418,
-0.0110180140534124));
#18746=CARTESIAN_POINT('Ctrl Pts',(0.00496735012263712,-0.0379984740334646,
-0.0110293117730038));
#18747=CARTESIAN_POINT('Ctrl Pts',(0.00496096520631356,-0.0379989254755268,
-0.0110350948099002));
#18748=CARTESIAN_POINT('Ctrl Pts',(0.00494405723907815,-0.0380001399927284,
-0.0110506686455708));
#18749=CARTESIAN_POINT('Ctrl Pts',(0.00493362221799278,-0.0380009095750944,
-0.0110605533323193));
#18750=CARTESIAN_POINT('Ctrl Pts',(0.00486754540254391,-0.0380059039048724,
-0.0111249204354672));
#18751=CARTESIAN_POINT('Ctrl Pts',(0.00481596133795193,-0.0380103590664143,
-0.0111833998149025));
#18752=CARTESIAN_POINT('Ctrl Pts',(0.00472471966667389,-0.0380190431794876,
-0.0113041272069601));
#18753=CARTESIAN_POINT('Ctrl Pts',(0.00468466372013476,-0.038023259303859,
-0.0113658298368658));
#18754=CARTESIAN_POINT('Ctrl Pts',(0.00462507340229277,-0.038030135143714,
-0.0114737786134851));
#18755=CARTESIAN_POINT('Ctrl Pts',(0.00460311759566668,-0.0380328566815838,
-0.0115185464607139));
#18756=CARTESIAN_POINT('Ctrl Pts',(0.00457566874831347,-0.0380365379927172,
-0.011582130636113));
#18757=CARTESIAN_POINT('Ctrl Pts',(0.00456830924681202,-0.038037559075236,
-0.011600103572483));
#18758=CARTESIAN_POINT('Ctrl Pts',(0.0045561331106894,-0.0380393109226003,
-0.0116315178444111));
#18759=CARTESIAN_POINT('Ctrl Pts',(0.00455116022499072,-0.0380400468037795,
-0.0116448956686408));
#18760=CARTESIAN_POINT('Ctrl Pts',(0.00454124135223827,-0.0380415590612276,
-0.0116727565185476));
#18761=CARTESIAN_POINT('Ctrl Pts',(0.00453632378006639,-0.0380423344387303,
-0.0116872480316083));
#18762=CARTESIAN_POINT('Ctrl Pts',(0.00452396119820181,-0.0380443554230636,
-0.0117255419228124));
#18763=CARTESIAN_POINT('Ctrl Pts',(0.0045168761133895,-0.0380455893642825,
-0.0117494561811065));
#18764=CARTESIAN_POINT('Ctrl Pts',(0.00448127997067977,-0.0380522541178259,
-0.0118812538988614));
#18765=CARTESIAN_POINT('Ctrl Pts',(0.00446395646686249,-0.0380573210498084,
-0.0119918116526313));
#18766=CARTESIAN_POINT('Ctrl Pts',(0.00445756920838888,-0.0380635562817696,
-0.0121274568329522));
#18767=CARTESIAN_POINT('Ctrl Pts',(0.00445700000013722,-0.0380646707421583,
-0.0121516556448979));
#18768=CARTESIAN_POINT('Ctrl Pts',(0.004457,-0.0380657947427934,-0.0121758532778082));
#18769=CARTESIAN_POINT('',(0.00445700007887821,-0.0381834855813947,-0.0121753599123031));
#18770=CARTESIAN_POINT('Ctrl Pts',(0.00445700007571663,-0.0381834860550969,
-0.0121753699010766));
#18771=CARTESIAN_POINT('Ctrl Pts',(0.00445700807984317,-0.0381822989275644,
-0.0121503374505815));
#18772=CARTESIAN_POINT('Ctrl Pts',(0.00445762492030033,-0.0381810959311471,
-0.012125309835296));
#18773=CARTESIAN_POINT('Ctrl Pts',(0.00445962253413835,-0.0381790958161663,
-0.0120845571132157));
#18774=CARTESIAN_POINT('Ctrl Pts',(0.00446063611188745,-0.0381783132920324,
-0.0120688181718112));
#18775=CARTESIAN_POINT('Ctrl Pts',(0.00446257170777129,-0.0381770882764331,
-0.0120445653706469));
#18776=CARTESIAN_POINT('Ctrl Pts',(0.00446332367190949,-0.0381766539205719,
-0.0120360386694657));
#18777=CARTESIAN_POINT('Ctrl Pts',(0.00446489085249986,-0.0381758196083426,
-0.0120198120955244));
#18778=CARTESIAN_POINT('Ctrl Pts',(0.00446569316761004,-0.0381754203257101,
-0.0120121111393718));
#18779=CARTESIAN_POINT('Ctrl Pts',(0.00446756295966174,-0.0381745453786827,
-0.0119953864492878));
#18780=CARTESIAN_POINT('Ctrl Pts',(0.00446865223033783,-0.0381740685839721,
-0.0119863656554562));
#18781=CARTESIAN_POINT('Ctrl Pts',(0.00447186392729497,-0.0381727475633907,
-0.0119616073729424));
#18782=CARTESIAN_POINT('Ctrl Pts',(0.00447414968119314,-0.0381718952545135,
-0.0119458925604982));
#18783=CARTESIAN_POINT('Ctrl Pts',(0.00449016356999372,-0.0381664331563208,
-0.0118465820682879));
#18784=CARTESIAN_POINT('Ctrl Pts',(0.00451051349907191,-0.0381615687160591,
-0.0117642056823892));
#18785=CARTESIAN_POINT('Ctrl Pts',(0.0045559364556698,-0.0381534125390411,
-0.0116291661022431));
#18786=CARTESIAN_POINT('Ctrl Pts',(0.00457741581831107,-0.0381501169455277,
-0.0115754857057749));
#18787=CARTESIAN_POINT('Ctrl Pts',(0.00462431818260893,-0.0381439220813868,
-0.0114750194002862));
#18788=CARTESIAN_POINT('Ctrl Pts',(0.00464925060196407,-0.0381410161507218,
-0.0114280929604154));
#18789=CARTESIAN_POINT('Ctrl Pts',(0.0046869077234412,-0.0381371196432484,
-0.0113652713226151));
#18790=CARTESIAN_POINT('Ctrl Pts',(0.00469759758237722,-0.0381360601704495,
-0.011348204544784));
#18791=CARTESIAN_POINT('Ctrl Pts',(0.00471667604155027,-0.038134246788412,
-0.0113190304687672));
#18792=CARTESIAN_POINT('Ctrl Pts',(0.00472490939227096,-0.0381334874138191,
-0.011306825274943));
#18793=CARTESIAN_POINT('Ctrl Pts',(0.00474230745449342,-0.0381319290747664,
-0.0112818139298716));
#18794=CARTESIAN_POINT('Ctrl Pts',(0.00475149607945117,-0.0381311311216071,
-0.0112690264597757));
#18795=CARTESIAN_POINT('Ctrl Pts',(0.00477616232250487,-0.038129052077859,
-0.0112357851344111));
#18796=CARTESIAN_POINT('Ctrl Pts',(0.00479195722761334,-0.0381277831069042,
-0.0112155723157098));
#18797=CARTESIAN_POINT('Ctrl Pts',(0.00487507652800483,-0.0381213955429583,
-0.0111145026714802));
#18798=CARTESIAN_POINT('Ctrl Pts',(0.00495003877684577,-0.0381165867220101,
-0.0110402912785554));
#18799=CARTESIAN_POINT('Ctrl Pts',(0.00507519223321637,-0.0381091917841313,
-0.0109394634943782));
#18800=CARTESIAN_POINT('Ctrl Pts',(0.00512025569620734,-0.0381066292231524,
-0.0109070039961268));
#18801=CARTESIAN_POINT('Ctrl Pts',(0.00519348889081106,-0.0381024700344351,
-0.0108600335463647));
#18802=CARTESIAN_POINT('Ctrl Pts',(0.00522052391392337,-0.0381009353425285,
-0.010843840312821));
#18803=CARTESIAN_POINT('Ctrl Pts',(0.0052582563208355,-0.0380987688325838,
-0.0108227818329828));
#18804=CARTESIAN_POINT('Ctrl Pts',(0.00526854295633942,-0.0380981757596999,
-0.0108171934241297));
#18805=CARTESIAN_POINT('Ctrl Pts',(0.00528621188648847,-0.0380971512637479,
-0.0108078532556764));
#18806=CARTESIAN_POINT('Ctrl Pts',(0.00529356246781917,-0.0380967233298339,
-0.0108040429618428));
#18807=CARTESIAN_POINT('Ctrl Pts',(0.00530953191190565,-0.038095789429608,
-0.0107959273373983));
#18808=CARTESIAN_POINT('Ctrl Pts',(0.00531816057534008,-0.0380952823298245,
-0.0107916434775061));
#18809=CARTESIAN_POINT('Ctrl Pts',(0.00534354809358269,-0.0380937843119392,
-0.0107793343458034));
#18810=CARTESIAN_POINT('Ctrl Pts',(0.00536041201016674,-0.0380927816436721,
-0.0107715308865477));
#18811=CARTESIAN_POINT('Ctrl Pts',(0.00549805625916409,-0.0380845608367445,
-0.0107108321336211));
#18812=CARTESIAN_POINT('Ctrl Pts',(0.00562502124387916,-0.0380768048646116,
-0.0106733128717973));
#18813=CARTESIAN_POINT('Ctrl Pts',(0.00581244822232353,-0.038066152985259,
-0.0106431975338362));
#18814=CARTESIAN_POINT('Ctrl Pts',(0.00587015912738619,-0.0380629684097801,
-0.0106372332057918));
#18815=CARTESIAN_POINT('Ctrl Pts',(0.00594871316956669,-0.0380587791022423,
-0.0106335674585809));
#18816=CARTESIAN_POINT('Ctrl Pts',(0.00596937048082932,-0.0380576907119355,
-0.0106330189464952));
#18817=CARTESIAN_POINT('Ctrl Pts',(0.00600483799414925,-0.038055844035549,
-0.0106327898455211));
#18818=CARTESIAN_POINT('Ctrl Pts',(0.00601964365291815,-0.038055079730333,
-0.0106329072939921));
#18819=CARTESIAN_POINT('Ctrl Pts',(0.00605000969443451,-0.0380535249906304,
-0.0106335853494047));
#18820=CARTESIAN_POINT('Ctrl Pts',(0.00606556790175287,-0.0380527353294816,
-0.0106341684185913));
#18821=CARTESIAN_POINT('Ctrl Pts',(0.00610583294606137,-0.0380507081970563,
-0.0106362880693841));
#18822=CARTESIAN_POINT('Ctrl Pts',(0.00613051676522877,-0.0380494816953564,
-0.0106381839049589));
#18823=CARTESIAN_POINT('Ctrl Pts',(0.00626824397463171,-0.0380427120303106,
-0.0106521026018443));
#18824=CARTESIAN_POINT('Ctrl Pts',(0.00637973157732812,-0.038037543715466,
-0.0106759944487953));
#18825=CARTESIAN_POINT('Ctrl Pts',(0.00653586664681331,-0.0380299597710212,
-0.0107279978777897));
#18826=CARTESIAN_POINT('Ctrl Pts',(0.00658331775017463,-0.0380275997335011,
-0.0107464554153444));
#18827=CARTESIAN_POINT('Ctrl Pts',(0.00664864808128062,-0.0380241697618877,
-0.010775663163989));
#18828=CARTESIAN_POINT('Ctrl Pts',(0.0066673560474783,-0.038023165755405,
-0.0107844825387745));
#18829=CARTESIAN_POINT('Ctrl Pts',(0.00670026979723398,-0.0380213509544965,
-0.0108008153773835));
#18830=CARTESIAN_POINT('Ctrl Pts',(0.00671454628657624,-0.0380205471693319,
-0.0108081798577217));
#18831=CARTESIAN_POINT('Ctrl Pts',(0.00673674766594897,-0.0380192670276144,
-0.0108200748621562));
#18832=CARTESIAN_POINT('Ctrl Pts',(0.00674475208108348,-0.0380187992270411,
-0.0108244552737066));
#18833=CARTESIAN_POINT('Ctrl Pts',(0.00676002458251343,-0.0380178937080423,
-0.0108329900352291));
#18834=CARTESIAN_POINT('Ctrl Pts',(0.00676729850016675,-0.0380174566531655,
-0.0108371329728309));
#18835=CARTESIAN_POINT('Ctrl Pts',(0.00678560906360607,-0.0380163424112395,
-0.0108477601980334));
#18836=CARTESIAN_POINT('Ctrl Pts',(0.00679659929907176,-0.0380156606040953,
-0.0108543229657534));
#18837=CARTESIAN_POINT('Ctrl Pts',(0.00684014445618043,-0.0380129107379959,
-0.0108810663006635));
#18838=CARTESIAN_POINT('Ctrl Pts',(0.00687202293689719,-0.038010788414809,
-0.0109023181837307));
#18839=CARTESIAN_POINT('Ctrl Pts',(0.00698681436741511,-0.0380028234465747,
-0.0109851761497589));
#18840=CARTESIAN_POINT('Ctrl Pts',(0.00706427446941344,-0.0379968177445107,
-0.0110538746208163));
#18841=CARTESIAN_POINT('Ctrl Pts',(0.0071740077331866,-0.0379877305783903,
-0.0111728644334368));
#18842=CARTESIAN_POINT('Ctrl Pts',(0.0072112402895965,-0.0379845108065972,
-0.0112181587267912));
#18843=CARTESIAN_POINT('Ctrl Pts',(0.00725803680560202,-0.0379802848797113,
-0.0112821968320577));
#18844=CARTESIAN_POINT('Ctrl Pts',(0.00726992594912318,-0.0379791931046738,
-0.0112991739829865));
#18845=CARTESIAN_POINT('Ctrl Pts',(0.00728972215826971,-0.0379773425095217,
-0.011328690228237));
#18846=CARTESIAN_POINT('Ctrl Pts',(0.00729779697143078,-0.0379765776049487,
-0.0113411128875556));
#18847=CARTESIAN_POINT('Ctrl Pts',(0.00731397731524256,-0.0379750231675733,
-0.0113668079291437));
#18848=CARTESIAN_POINT('Ctrl Pts',(0.00732206364079725,-0.0379742343817509,
-0.0113800904278613));
#18849=CARTESIAN_POINT('Ctrl Pts',(0.00734244984074504,-0.0379722127824101,
-0.0114147452965651));
#18850=CARTESIAN_POINT('Ctrl Pts',(0.00735444086040068,-0.0379709908180102,
-0.0114362946446358));
#18851=CARTESIAN_POINT('Ctrl Pts',(0.00741913772724974,-0.0379641875599236,
-0.0115594190686797));
#18852=CARTESIAN_POINT('Ctrl Pts',(0.00746093124990526,-0.0379589873458232,
-0.0116663196475656));
#18853=CARTESIAN_POINT('Ctrl Pts',(0.00750812729823622,-0.0379505746811456,
-0.01184263198142));
#18854=CARTESIAN_POINT('Ctrl Pts',(0.00752135881475362,-0.0379474105157327,
-0.0119094883294143));
#18855=CARTESIAN_POINT('Ctrl Pts',(0.00753242208193721,-0.0379431907103036,
-0.0119946149908679));
#18856=CARTESIAN_POINT('Ctrl Pts',(0.00753440754080903,-0.0379423049753607,
-0.0120122739264848));
#18857=CARTESIAN_POINT('Ctrl Pts',(0.00753698319781072,-0.037940923684118,
-0.0120393930815286));
#18858=CARTESIAN_POINT('Ctrl Pts',(0.00753779198449694,-0.0379404390503911,
-0.0120488314712813));
#18859=CARTESIAN_POINT('Ctrl Pts',(0.00753914811192466,-0.0379395196003125,
-0.0120665766436435));
#18860=CARTESIAN_POINT('Ctrl Pts',(0.00753971521668366,-0.0379390858087027,
-0.0120748813337784));
#18861=CARTESIAN_POINT('Ctrl Pts',(0.00754082247524485,-0.037938117140808,
-0.0120932857777353));
#18862=CARTESIAN_POINT('Ctrl Pts',(0.00754133056990211,-0.0379375806535036,
-0.0121033870347872));
#18863=CARTESIAN_POINT('Ctrl Pts',(0.00754276521091481,-0.0379356816540669,
-0.0121388554005697));
#18864=CARTESIAN_POINT('Ctrl Pts',(0.00754316502977748,-0.0379342953127187,
-0.0121642387069013));
#18865=CARTESIAN_POINT('Ctrl Pts',(0.00754184859055401,-0.0379261207809339,
-0.0123117932454939));
#18866=CARTESIAN_POINT('Ctrl Pts',(0.00752625215587118,-0.0379189639945425,
-0.01243340616555));
#18867=CARTESIAN_POINT('Ctrl Pts',(0.00748264940151215,-0.0379089356998104,
-0.0126069178101067));
#18868=CARTESIAN_POINT('Ctrl Pts',(0.0074658030157952,-0.0379058228519004,
-0.0126611247624748));
#18869=CARTESIAN_POINT('Ctrl Pts',(0.00743884320527958,-0.0379017084221201,
-0.0127335277771436));
#18870=CARTESIAN_POINT('Ctrl Pts',(0.00743129457268651,-0.0379006271128298,
-0.0127526257774028));
#18871=CARTESIAN_POINT('Ctrl Pts',(0.00741765903974918,-0.037898788619515,
-0.0127852057392401));
#18872=CARTESIAN_POINT('Ctrl Pts',(0.00741175549746775,-0.0378980255527028,
-0.0127987609841155));
#18873=CARTESIAN_POINT('Ctrl Pts',(0.0073992205315759,-0.0378964700999605,
-0.0128264488057111));
#18874=CARTESIAN_POINT('Ctrl Pts',(0.00739256762208163,-0.0378956785434963,
-0.0128405698170947));
#18875=CARTESIAN_POINT('Ctrl Pts',(0.00737472283245302,-0.0378936394780892,
-0.012877001662737));
#18876=CARTESIAN_POINT('Ctrl Pts',(0.00736320168852828,-0.0378924031998277,
-0.0128991465552474));
#18877=CARTESIAN_POINT('Ctrl Pts',(0.00728918753461557,-0.037884911346354,
-0.0130333532422099));
#18878=CARTESIAN_POINT('Ctrl Pts',(0.00721346018153639,-0.0378791503089205,
-0.0131375318015117));
#18879=CARTESIAN_POINT('Ctrl Pts',(0.00709762948768706,-0.0378712948858956,
-0.0132610925740447));
#18880=CARTESIAN_POINT('Ctrl Pts',(0.00706836561876731,-0.0378693693736668,
-0.013289913160092));
#18881=CARTESIAN_POINT('Ctrl Pts',(0.00702451332050914,-0.0378665094785237,
-0.0133297827250322));
#18882=CARTESIAN_POINT('Ctrl Pts',(0.00701082237679593,-0.0378656199006003,
-0.0133417944391915));
#18883=CARTESIAN_POINT('Ctrl Pts',(0.00698577913624491,-0.037863992055212,
-0.0133629933991921));
#18884=CARTESIAN_POINT('Ctrl Pts',(0.00697450281609892,-0.0378632588495482,
-0.0133722672556405));
#18885=CARTESIAN_POINT('Ctrl Pts',(0.00695620831328639,-0.0378620659213311,
-0.0133868827670183));
#18886=CARTESIAN_POINT('Ctrl Pts',(0.00694927275554217,-0.0378616129127327,
-0.0133923268659148));
#18887=CARTESIAN_POINT('Ctrl Pts',(0.00693541194317428,-0.0378607052369154,
-0.0134030162602077));
#18888=CARTESIAN_POINT('Ctrl Pts',(0.00692848831584314,-0.0378602506931865,
-0.0134082630829192));
#18889=CARTESIAN_POINT('Ctrl Pts',(0.00691030559669374,-0.0378590548142371,
-0.0134218020190708));
#18890=CARTESIAN_POINT('Ctrl Pts',(0.00689897761272639,-0.0378583076407613,
-0.013429999908378));
#18891=CARTESIAN_POINT('Ctrl Pts',(0.0068420288953634,-0.0378545472819169,
-0.0134700448371934));
#18892=CARTESIAN_POINT('Ctrl Pts',(0.00679482326411402,-0.0378514185731017,
-0.0134995600040748));
#18893=CARTESIAN_POINT('Ctrl Pts',(0.00666467282035146,-0.037842953753567,
-0.01357146054196));
#18894=CARTESIAN_POINT('Ctrl Pts',(0.00657930379798323,-0.0378375769561464,
-0.0136090031920098));
#18895=CARTESIAN_POINT('Ctrl Pts',(0.00644267103213172,-0.0378295399490264,
-0.0136548725091541));
#18896=CARTESIAN_POINT('Ctrl Pts',(0.00639349207595639,-0.0378267506887686,
-0.0136687096907971));
#18897=CARTESIAN_POINT('Ctrl Pts',(0.00632431982629685,-0.0378229783734204,
-0.0136845154129562));
#18898=CARTESIAN_POINT('Ctrl Pts',(0.00630484148510345,-0.0378219321949302,
-0.0136885715282358));
#18899=CARTESIAN_POINT('Ctrl Pts',(0.00627085742960144,-0.0378201340227966,
-0.0136949651687964));
#18900=CARTESIAN_POINT('Ctrl Pts',(0.00625638699410977,-0.0378193768152442,
-0.0136974742598952));
#18901=CARTESIAN_POINT('Ctrl Pts',(0.00622624169192059,-0.0378178162303741,
-0.0137022590315536));
#18902=CARTESIAN_POINT('Ctrl Pts',(0.00621056313719906,-0.0378170139817988,
-0.0137045007247273));
#18903=CARTESIAN_POINT('Ctrl Pts',(0.00616895240852485,-0.0378149081547002,
-0.0137097977991449));
#18904=CARTESIAN_POINT('Ctrl Pts',(0.00614297201513083,-0.0378136173055151,
-0.0137124370893317));
#18905=CARTESIAN_POINT('Ctrl Pts',(0.00603102321530504,-0.0378081421068277,
-0.0137209455930713));
#18906=CARTESIAN_POINT('Ctrl Pts',(0.0059447099690384,-0.0378041511837471,
-0.0137202681247507));
#18907=CARTESIAN_POINT('Ctrl Pts',(0.00579060372199138,-0.037797032614861,
-0.0137061167025053));
#18908=CARTESIAN_POINT('Ctrl Pts',(0.0057228030738379,-0.0377938993302986,
-0.0136952985722337));
#18909=CARTESIAN_POINT('Ctrl Pts',(0.00562136959709282,-0.0377889543294175,
-0.0136720973882863));
#18910=CARTESIAN_POINT('Ctrl Pts',(0.00558707394227576,-0.0377872356323674,
-0.0136629979180245));
#18911=CARTESIAN_POINT('Ctrl Pts',(0.00554146382910192,-0.0377848510823236,
-0.0136491971031509));
#18912=CARTESIAN_POINT('Ctrl Pts',(0.00552984562799984,-0.0377842348900536,
-0.0136455308944181));
#18913=CARTESIAN_POINT('Ctrl Pts',(0.00551034065796981,-0.0377831837102982,
-0.0136391210117759));
#18914=CARTESIAN_POINT('Ctrl Pts',(0.00550243034242742,-0.0377827527039749,
-0.0136364501308802));
#18915=CARTESIAN_POINT('Ctrl Pts',(0.00548566071650898,-0.0377818283889091,
-0.0136306359028756));
#18916=CARTESIAN_POINT('Ctrl Pts',(0.00547680795746787,-0.0377813342124315,
-0.0136274756331677));
#18917=CARTESIAN_POINT('Ctrl Pts',(0.00545164789698164,-0.0377799130550043,
-0.013618233914956));
#18918=CARTESIAN_POINT('Ctrl Pts',(0.00543541427619001,-0.0377789759911882,
-0.0136119573282488));
#18919=CARTESIAN_POINT('Ctrl Pts',(0.00535849093638101,-0.0377744508016309,
-0.0135807097756336));
#18920=CARTESIAN_POINT('Ctrl Pts',(0.00529933233094438,-0.0377707186420423,
-0.0135521596877642));
#18921=CARTESIAN_POINT('Ctrl Pts',(0.00518747121469487,-0.0377633730753424,
-0.013489089675816));
#18922=CARTESIAN_POINT('Ctrl Pts',(0.00513469924815449,-0.0377597683981727,
-0.0134549341945922));
#18923=CARTESIAN_POINT('Ctrl Pts',(0.00503405821432215,-0.0377527278115195,
-0.0133807101955868));
#18924=CARTESIAN_POINT('Ctrl Pts',(0.00498623977971189,-0.037749297188404,
-0.0133407632566839));
#18925=CARTESIAN_POINT('Ctrl Pts',(0.00492563777726345,-0.0377448535662062,
-0.0132835711065105));
#18926=CARTESIAN_POINT('Ctrl Pts',(0.00491061137684016,-0.037743742731776,
-0.0132687967615019));
#18927=CARTESIAN_POINT('Ctrl Pts',(0.0048855013686708,-0.0377418700184975,
-0.0132430754017576));
#18928=CARTESIAN_POINT('Ctrl Pts',(0.00487526517504037,-0.0377411016846315,
-0.0132322820991348));
#18929=CARTESIAN_POINT('Ctrl Pts',(0.00485471834755247,-0.0377395486010616,
-0.0132099797883413));
#18930=CARTESIAN_POINT('Ctrl Pts',(0.00484442130313724,-0.0377387644546698,
-0.0131984605339193));
#18931=CARTESIAN_POINT('Ctrl Pts',(0.00481847798327455,-0.0377367723073857,
-0.0131685454950425));
#18932=CARTESIAN_POINT('Ctrl Pts',(0.00480308715622287,-0.0377355745219901,
-0.0131499332721656));
#18933=CARTESIAN_POINT('Ctrl Pts',(0.00471495254004244,-0.0377286024367416,
-0.0130381068754308));
#18934=CARTESIAN_POINT('Ctrl Pts',(0.00465268274694993,-0.0377232417255833,
-0.0129371455930511));
#18935=CARTESIAN_POINT('Ctrl Pts',(0.00457468299869719,-0.0377147545366238,
-0.0127705302791683));
#18936=CARTESIAN_POINT('Ctrl Pts',(0.00455064934321615,-0.0377116925299048,
-0.0127092861449259));
#18937=CARTESIAN_POINT('Ctrl Pts',(0.00452524934850776,-0.0377075980442318,
-0.0126300189172918));
#18938=CARTESIAN_POINT('Ctrl Pts',(0.00452018820768795,-0.037706724340247,
-0.0126132466069257));
#18939=CARTESIAN_POINT('Ctrl Pts',(0.00451284577453923,-0.0377053578740374,
-0.0125873263699636));
#18940=CARTESIAN_POINT('Ctrl Pts',(0.00451036079410119,-0.0377048756710023,
-0.0125782372030808));
#18941=CARTESIAN_POINT('Ctrl Pts',(0.00450583351982344,-0.0377039577637918,
-0.0125610611414061));
#18942=CARTESIAN_POINT('Ctrl Pts',(0.00450377330456181,-0.0377035230221076,
-0.012552979560188));
#18943=CARTESIAN_POINT('Ctrl Pts',(0.00449934107489913,-0.0377025491341382,
-0.0125349851270053));
#18944=CARTESIAN_POINT('Ctrl Pts',(0.00449700157425229,-0.0377020083096759,
-0.0125250646980416));
#18945=CARTESIAN_POINT('Ctrl Pts',(0.0044901785992861,-0.0377003476516746,
-0.0124947930931023));
#18946=CARTESIAN_POINT('Ctrl Pts',(0.00448600910315711,-0.0376992133191691,
-0.0124743742259443));
#18947=CARTESIAN_POINT('Ctrl Pts',(0.00446545223544528,-0.0376929243330159,
-0.0123621537026758));
#18948=CARTESIAN_POINT('Ctrl Pts',(0.004457,-0.0376875227620494,-0.0122690985381315));
#18949=CARTESIAN_POINT('Ctrl Pts',(0.004457,-0.0376822061652104,-0.0121758532865636));
#18950=CARTESIAN_POINT('Ctrl Pts',(0.004457,-0.0381835089768636,-0.0121758532865662));
#18951=CARTESIAN_POINT('Ctrl Pts',(0.004457,-0.0381835010212319,-0.0121756854996429));
#18952=CARTESIAN_POINT('Ctrl Pts',(0.00445700002522786,-0.0381834935385169,
-0.012175527700736));
#18953=CARTESIAN_POINT('Ctrl Pts',(0.00445700007887821,-0.0381834855813947,
-0.0121753599123022));
#18954=CARTESIAN_POINT('Origin',(0.006,-0.0418165664398416,-0.0121758532865581));
#18955=CARTESIAN_POINT('',(0.004457,-0.0386811151660051,-0.0121758532865589));
#18956=CARTESIAN_POINT('',(0.004457,-0.0385661060144854,-0.0121758532811924));
#18957=CARTESIAN_POINT('',(0.004457,-0.0418165664398416,-0.0121758532865581));
#18958=CARTESIAN_POINT('Ctrl Pts',(0.004457,-0.0380657947427934,-0.0121758532778082));
#18959=CARTESIAN_POINT('Ctrl Pts',(0.00445699999983535,-0.0380671435044447,
-0.0122048895953197));
#18960=CARTESIAN_POINT('Ctrl Pts',(0.00445781961298393,-0.038068505989213,
-0.0122339242157708));
#18961=CARTESIAN_POINT('Ctrl Pts',(0.00446118822220695,-0.0380713599617527,
-0.0122935261098348));
#18962=CARTESIAN_POINT('Ctrl Pts',(0.0044638293621826,-0.0380728535150145,
-0.0123240698070411));
#18963=CARTESIAN_POINT('Ctrl Pts',(0.00446869948897067,-0.0380749627659856,
-0.0123658479666247));
#18964=CARTESIAN_POINT('Ctrl Pts',(0.00447014652476572,-0.0380755410043585,
-0.0123771678740451));
#18965=CARTESIAN_POINT('Ctrl Pts',(0.00447282823197034,-0.0380765386945114,
-0.0123964438528787));
#18966=CARTESIAN_POINT('Ctrl Pts',(0.00447399987108635,-0.0380769547654142,
-0.0124044083395628));
#18967=CARTESIAN_POINT('Ctrl Pts',(0.00447665618908617,-0.0380778581390544,
-0.0124215334582408));
#18968=CARTESIAN_POINT('Ctrl Pts',(0.00447816123761015,-0.0380783464666718,
-0.0124306902653564));
#18969=CARTESIAN_POINT('Ctrl Pts',(0.00448267182002354,-0.0380797457356139,
-0.0124566666027664));
#18970=CARTESIAN_POINT('Ctrl Pts',(0.00448587418102869,-0.0380806664982276,
-0.012473450131933));
#18971=CARTESIAN_POINT('Ctrl Pts',(0.00450278334738427,-0.0380851947666801,
-0.012554716069166));
#18972=CARTESIAN_POINT('Ctrl Pts',(0.00452033361440335,-0.0380889513892934,
-0.012618324651428));
#18973=CARTESIAN_POINT('Ctrl Pts',(0.00456054257561717,-0.0380959989429903,
-0.0127344771135427));
#18974=CARTESIAN_POINT('Ctrl Pts',(0.00458216071951842,-0.0380992791774221,
-0.0127872699712157));
#18975=CARTESIAN_POINT('Ctrl Pts',(0.00463618295554917,-0.0381064019535798,
-0.0129008204621711));
#18976=CARTESIAN_POINT('Ctrl Pts',(0.00466983246931066,-0.0381102115358557,
-0.0129608567631454));
#18977=CARTESIAN_POINT('Ctrl Pts',(0.00471898888154054,-0.0381150191045294,
-0.0130362669221104));
#18978=CARTESIAN_POINT('Ctrl Pts',(0.00473096741426037,-0.0381161414827133,
-0.0130538381760918));
#18979=CARTESIAN_POINT('Ctrl Pts',(0.00475176843359826,-0.0381180109082736,
-0.0130830355604993));
#18980=CARTESIAN_POINT('Ctrl Pts',(0.00476039933485078,-0.03811876502757,
-0.0130947939439439));
#18981=CARTESIAN_POINT('Ctrl Pts',(0.00477810579649577,-0.0381202701655854,
-0.0131182129936916));
#18982=CARTESIAN_POINT('Ctrl Pts',(0.00478718471451662,-0.0381210209387773,
-0.0131298692010061));
#18983=CARTESIAN_POINT('Ctrl Pts',(0.00481036138111931,-0.0381228870031466,
-0.0131587594989513));
#18984=CARTESIAN_POINT('Ctrl Pts',(0.00482466753772719,-0.038123993898954,
-0.0131758224517869));
#18985=CARTESIAN_POINT('Ctrl Pts',(0.00489444620257537,-0.0381291945185664,
-0.013255480219889));
#18986=CARTESIAN_POINT('Ctrl Pts',(0.00495458055196259,-0.0381330928762353,
-0.0133138090911115));
#18987=CARTESIAN_POINT('Ctrl Pts',(0.00506820173835038,-0.0381398592891376,
-0.013407372142183));
#18988=CARTESIAN_POINT('Ctrl Pts',(0.00511970096203076,-0.0381427464205802,
-0.0134446952507317));
#18989=CARTESIAN_POINT('Ctrl Pts',(0.00521532228253025,-0.0381480312710724,
-0.0135053646154909));
#18990=CARTESIAN_POINT('Ctrl Pts',(0.00525855063894455,-0.0381503964402284,
-0.0135299476637632));
#18991=CARTESIAN_POINT('Ctrl Pts',(0.00531469273167647,-0.0381535299917057,
-0.0135583792707786));
#18992=CARTESIAN_POINT('Ctrl Pts',(0.00532657551026155,-0.0381541966332639,
-0.0135642061176475));
#18993=CARTESIAN_POINT('Ctrl Pts',(0.00534609763065624,-0.0381552996934874,
-0.0135734694101563));
#18994=CARTESIAN_POINT('Ctrl Pts',(0.00535369286322768,-0.0381557307606498,
-0.0135769978966976));
#18995=CARTESIAN_POINT('Ctrl Pts',(0.00536915626440788,-0.0381566129714147,
-0.013584029182476));
#18996=CARTESIAN_POINT('Ctrl Pts',(0.0053770257148027,-0.0381570642868594,
-0.013587528251132));
#18997=CARTESIAN_POINT('Ctrl Pts',(0.00539809565114217,-0.0381582780774296,
-0.0135966862915016));
#18998=CARTESIAN_POINT('Ctrl Pts',(0.00541134628720841,-0.0381590470467546,
-0.0136022270281897));
#18999=CARTESIAN_POINT('Ctrl Pts',(0.00549674573701938,-0.0381640298882131,
-0.013636544083683));
#19000=CARTESIAN_POINT('Ctrl Pts',(0.00557089842790941,-0.0381684730869033,
-0.01366002055429));
#19001=CARTESIAN_POINT('Ctrl Pts',(0.00571773034744465,-0.0381771292662065,
-0.0136945791371872));
#19002=CARTESIAN_POINT('Ctrl Pts',(0.00579007104340357,-0.038181329476216,
-0.0137062569606283));
#19003=CARTESIAN_POINT('Ctrl Pts',(0.00591298706225166,-0.0381882135544161,
-0.0137172160909405));
#19004=CARTESIAN_POINT('Ctrl Pts',(0.00596319466645026,-0.0381909570406077,
-0.0137192316097876));
#19005=CARTESIAN_POINT('Ctrl Pts',(0.0060328811100179,-0.0381946618576342,
-0.0137186257219291));
#19006=CARTESIAN_POINT('Ctrl Pts',(0.00605234274003579,-0.0381956855584709,
-0.0137180881060579));
#19007=CARTESIAN_POINT('Ctrl Pts',(0.00608605273259973,-0.0381974404138359,
-0.0137165180149759));
#19008=CARTESIAN_POINT('Ctrl Pts',(0.00610030625282324,-0.0381981767334831,
-0.0137156557258019));
#19009=CARTESIAN_POINT('Ctrl Pts',(0.00612978837194869,-0.0381996885863862,
-0.0137134610367704));
#19010=CARTESIAN_POINT('Ctrl Pts',(0.00614501329676942,-0.0382004631434111,
-0.0137120999400151));
#19011=CARTESIAN_POINT('Ctrl Pts',(0.00618493078721593,-0.0382024790188276,
-0.0137079326218436));
#19012=CARTESIAN_POINT('Ctrl Pts',(0.00620958055973648,-0.0382037087855468,
-0.0137047556901279));
#19013=CARTESIAN_POINT('Ctrl Pts',(0.00634520183711845,-0.0382104084754807,
-0.0136839346158737));
#19014=CARTESIAN_POINT('Ctrl Pts',(0.0064540638989913,-0.0382155082278199,
-0.0136548060586707));
#19015=CARTESIAN_POINT('Ctrl Pts',(0.0066080527406302,-0.0382230949450686,
-0.0135949771448086));
#19016=CARTESIAN_POINT('Ctrl Pts',(0.00665628472931976,-0.0382255354925383,
-0.0135733261791716));
#19017=CARTESIAN_POINT('Ctrl Pts',(0.00673046276573406,-0.0382295206826934,
-0.013535339902022));
#19018=CARTESIAN_POINT('Ctrl Pts',(0.00675719700238102,-0.0382310074785839,
-0.0135206328955101));
#19019=CARTESIAN_POINT('Ctrl Pts',(0.00679329132080773,-0.03823310868262,
-0.0134993591171764));
#19020=CARTESIAN_POINT('Ctrl Pts',(0.00680304182349797,-0.038233686004875,
-0.0134934657555407));
#19021=CARTESIAN_POINT('Ctrl Pts',(0.0068195667804657,-0.0382346826484039,
-0.0134832262472041));
#19022=CARTESIAN_POINT('Ctrl Pts',(0.00682637422978806,-0.0382350986085255,
-0.0134789340196165));
#19023=CARTESIAN_POINT('Ctrl Pts',(0.0068409668984029,-0.038236002406832,
-0.0134695727199938));
#19024=CARTESIAN_POINT('Ctrl Pts',(0.00684874025884699,-0.0382364912814053,
-0.0134644863845009));
#19025=CARTESIAN_POINT('Ctrl Pts',(0.00687071813542158,-0.0382378936499025,
-0.0134498204993014));
#19026=CARTESIAN_POINT('Ctrl Pts',(0.00688480931842805,-0.0382388170290535,
-0.0134400743724093));
#19027=CARTESIAN_POINT('Ctrl Pts',(0.00695318541922314,-0.0382434064491255,
-0.0133910790917609));
#19028=CARTESIAN_POINT('Ctrl Pts',(0.00700503398884929,-0.0382472264109391,
-0.0133485602651859));
#19029=CARTESIAN_POINT('Ctrl Pts',(0.00711364808810536,-0.0382557546904811,
-0.0132469823122669));
#19030=CARTESIAN_POINT('Ctrl Pts',(0.00716881789551368,-0.0382604558362534,
-0.0131864946073077));
#19031=CARTESIAN_POINT('Ctrl Pts',(0.00724827278224507,-0.0382676670690895,
-0.0130841225701488));
#19032=CARTESIAN_POINT('Ctrl Pts',(0.00727583545307731,-0.0382702756367614,
-0.0130449807613799));
#19033=CARTESIAN_POINT('Ctrl Pts',(0.00731183127054694,-0.0382738354530292,
-0.0129884510230028));
#19034=CARTESIAN_POINT('Ctrl Pts',(0.00732182412396684,-0.0382748426814859,
-0.0129720928190118));
#19035=CARTESIAN_POINT('Ctrl Pts',(0.00733870259558942,-0.038276578704659,
-0.0129432690603765));
#19036=CARTESIAN_POINT('Ctrl Pts',(0.00734572511522204,-0.0382773123576638,
-0.0129308867570101));
#19037=CARTESIAN_POINT('Ctrl Pts',(0.0073599870690814,-0.0382788271658381,
-0.0129049084037625));
#19038=CARTESIAN_POINT('Ctrl Pts',(0.00736719630766292,-0.0382796071984416,
-0.012891297533345));
#19039=CARTESIAN_POINT('Ctrl Pts',(0.00738576650746705,-0.0382816569149313,
-0.0128549313001057));
#19040=CARTESIAN_POINT('Ctrl Pts',(0.00739677092433287,-0.0382829142872373,
-0.0128319987257191));
#19041=CARTESIAN_POINT('Ctrl Pts',(0.00745910568851641,-0.0382903251724763,
-0.0126934132851662));
#19042=CARTESIAN_POINT('Ctrl Pts',(0.00749661634607974,-0.038295995319929,
-0.0125720829410429));
#19043=CARTESIAN_POINT('Ctrl Pts',(0.00752641323578653,-0.0383038150650187,
-0.0124054948146707));
#19044=CARTESIAN_POINT('Ctrl Pts',(0.00753218344960865,-0.0383058100427304,
-0.0123631662121021));
#19045=CARTESIAN_POINT('Ctrl Pts',(0.00753869538771927,-0.0383091507532485,
-0.0122940815738798));
#19046=CARTESIAN_POINT('Ctrl Pts',(0.00754051014702595,-0.0383104590097946,
-0.0122674489309357));
#19047=CARTESIAN_POINT('Ctrl Pts',(0.00754209023758461,-0.0383123466062829,
-0.0122299332980799));
#19048=CARTESIAN_POINT('Ctrl Pts',(0.00754243266808351,-0.0383128980394328,
-0.0122190782802948));
#19049=CARTESIAN_POINT('Ctrl Pts',(0.00754282799913165,-0.0383138656868881,
-0.0122002365298423));
#19050=CARTESIAN_POINT('Ctrl Pts',(0.00754293352804778,-0.0383142790835482,
-0.0121922515437699));
#19051=CARTESIAN_POINT('Ctrl Pts',(0.00754302945416275,-0.0383151975917776,
-0.012174657195347));
#19052=CARTESIAN_POINT('Ctrl Pts',(0.00754299208568446,-0.0383157040914283,
-0.0121650486037614));
#19053=CARTESIAN_POINT('Ctrl Pts',(0.0075426099839195,-0.0383172399311027,
-0.0121361670637015));
#19054=CARTESIAN_POINT('Ctrl Pts',(0.00754199384730864,-0.0383182824232954,
-0.0121169001787294));
#19055=CARTESIAN_POINT('Ctrl Pts',(0.00753429929071721,-0.0383266015347025,
-0.0119652753631933));
#19056=CARTESIAN_POINT('Ctrl Pts',(0.00751055399220591,-0.0383344211604439,
-0.0118343176925457));
#19057=CARTESIAN_POINT('Ctrl Pts',(0.0074527409386233,-0.0383451361653055,
-0.0116526227619363));
#19058=CARTESIAN_POINT('Ctrl Pts',(0.00743200395649937,-0.0383483317346125,
-0.0115982788779986));
#19059=CARTESIAN_POINT('Ctrl Pts',(0.00739993305659684,-0.0383525131053811,
-0.011526661191722));
#19060=CARTESIAN_POINT('Ctrl Pts',(0.00739125117212372,-0.0383535850660717,
-0.0115082582238994));
#19061=CARTESIAN_POINT('Ctrl Pts',(0.00737579762136287,-0.0383553956542925,
-0.0114771130742473));
#19062=CARTESIAN_POINT('Ctrl Pts',(0.00736920672792558,-0.0383561403636114,
-0.0114642846432739));
#19063=CARTESIAN_POINT('Ctrl Pts',(0.00735623250052009,-0.0383575556329396,
-0.0114398797149205));
#19064=CARTESIAN_POINT('Ctrl Pts',(0.00734987838464185,-0.0383582271308845,
-0.0114282892061757));
#19065=CARTESIAN_POINT('Ctrl Pts',(0.0073326569759924,-0.0383599919828613,
-0.0113978114194754));
#19066=CARTESIAN_POINT('Ctrl Pts',(0.00732153703285888,-0.0383610762836326,
-0.0113790699458166));
#19067=CARTESIAN_POINT('Ctrl Pts',(0.00727277703884525,-0.0383656134123758,
-0.0113007208444145));
#19068=CARTESIAN_POINT('Ctrl Pts',(0.0072314710588288,-0.0383689330870022,
-0.0112434915260968));
#19069=CARTESIAN_POINT('Ctrl Pts',(0.00713666224147379,-0.038375789466167,
-0.0111294796788135));
#19070=CARTESIAN_POINT('Ctrl Pts',(0.0070824815473084,-0.0383793031862586,
-0.0110735230549431));
#19071=CARTESIAN_POINT('Ctrl Pts',(0.00698719408205497,-0.0383852496005133,
-0.010988941121996));
#19072=CARTESIAN_POINT('Ctrl Pts',(0.00694850794566672,-0.0383876116666768,
-0.0109578037945299));
#19073=CARTESIAN_POINT('Ctrl Pts',(0.0068976980667432,-0.03839074160144,
-0.0109207986240512));
#19074=CARTESIAN_POINT('Ctrl Pts',(0.00688690460279309,-0.0383914080155726,
-0.0109131481632644));
#19075=CARTESIAN_POINT('Ctrl Pts',(0.0068691210274355,-0.0383925107951502,
-0.0109008835769566));
#19076=CARTESIAN_POINT('Ctrl Pts',(0.006862189125193,-0.0383929418143081,
-0.0108961857402235));
#19077=CARTESIAN_POINT('Ctrl Pts',(0.00684805002197483,-0.0383938240390514,
-0.0108867705303029));
#19078=CARTESIAN_POINT('Ctrl Pts',(0.00684084093976675,-0.0383942754181773,
-0.0108820566644812));
#19079=CARTESIAN_POINT('Ctrl Pts',(0.00682150244178063,-0.0383954895661715,
-0.0108696415247008));
#19080=CARTESIAN_POINT('Ctrl Pts',(0.0068093045319716,-0.0383962588355577,
-0.010862049049065));
#19081=CARTESIAN_POINT('Ctrl Pts',(0.00673041054715641,-0.0384012471820097,
-0.0108144578151061));
#19082=CARTESIAN_POINT('Ctrl Pts',(0.00666088142703747,-0.0384056961038836,
-0.0107793823368367));
#19083=CARTESIAN_POINT('Ctrl Pts',(0.00652124517955258,-0.0384143657152724,
-0.0107217116003165));
#19084=CARTESIAN_POINT('Ctrl Pts',(0.00645156624148771,-0.0384185736073102,
-0.010698587660835));
#19085=CARTESIAN_POINT('Ctrl Pts',(0.00633201987255703,-0.0384254537258592,
-0.010668168063386));
#19086=CARTESIAN_POINT('Ctrl Pts',(0.00628296127953114,-0.0384281866313684,
-0.0106581953640873));
#19087=CARTESIAN_POINT('Ctrl Pts',(0.00621428101686512,-0.0384318801254271,
-0.010647680943186));
#19088=CARTESIAN_POINT('Ctrl Pts',(0.00619500659929544,-0.0384329025710778,
-0.0106451019881817));
#19089=CARTESIAN_POINT('Ctrl Pts',(0.00616150568970234,-0.0384346559878718,
-0.0106412625622064));
#19090=CARTESIAN_POINT('Ctrl Pts',(0.00614730123415734,-0.0384353921006449,
-0.0106398340342204));
#19091=CARTESIAN_POINT('Ctrl Pts',(0.00611784268506092,-0.038436904156625,
-0.0106372838287038));
#19092=CARTESIAN_POINT('Ctrl Pts',(0.00610258759797816,-0.0384376791127551,
-0.0106361914141553));
#19093=CARTESIAN_POINT('Ctrl Pts',(0.00606246660066957,-0.0384396974558967,
-0.010633917321175));
#19094=CARTESIAN_POINT('Ctrl Pts',(0.00603758355311282,-0.0384409292364718,
-0.0106331102232206));
#19095=CARTESIAN_POINT('Ctrl Pts',(0.00590070773605617,-0.0384476122290726,
-0.0106319844003105));
#19096=CARTESIAN_POINT('Ctrl Pts',(0.00578895855843419,-0.0384526962910275,
-0.0106432563634802));
#19097=CARTESIAN_POINT('Ctrl Pts',(0.00562753024324628,-0.0384602744794229,
-0.0106775449104602));
#19098=CARTESIAN_POINT('Ctrl Pts',(0.00557625759070285,-0.0384627237239554,
-0.0106912309280556));
#19099=CARTESIAN_POINT('Ctrl Pts',(0.0054966971565738,-0.0384667212688756,
-0.0107169255354325));
#19100=CARTESIAN_POINT('Ctrl Pts',(0.0054678876145529,-0.0384682112883679,
-0.0107271848874768));
#19101=CARTESIAN_POINT('Ctrl Pts',(0.00542878057143002,-0.0384703163332968,
-0.0107424352128361));
#19102=CARTESIAN_POINT('Ctrl Pts',(0.00541820409357194,-0.0384708940952837,
-0.0107466953113026));
#19103=CARTESIAN_POINT('Ctrl Pts',(0.00540024381031434,-0.0384718912423945,
-0.0107541619350641));
#19104=CARTESIAN_POINT('Ctrl Pts',(0.00539283599439193,-0.0384723072569423,
-0.0107573097888319));
#19105=CARTESIAN_POINT('Ctrl Pts',(0.00537693635652429,-0.0384732108542385,
-0.0107642134935593));
#19106=CARTESIAN_POINT('Ctrl Pts',(0.00536845343464775,-0.0384736994678609,
-0.0107679881878198));
#19107=CARTESIAN_POINT('Ctrl Pts',(0.00534443616982334,-0.0384751003586363,
-0.01077893602743));
#19108=CARTESIAN_POINT('Ctrl Pts',(0.00532898675762177,-0.0384760224905309,
-0.0107862911445877));
#19109=CARTESIAN_POINT('Ctrl Pts',(0.00525410389899635,-0.0384805839235611,
-0.0108234811789877));
#19110=CARTESIAN_POINT('Ctrl Pts',(0.00519652276539376,-0.0384843749496947,
-0.0108568785200506));
#19111=CARTESIAN_POINT('Ctrl Pts',(0.00509244026825954,-0.0384915585975431,
-0.010926597552579));
#19112=CARTESIAN_POINT('Ctrl Pts',(0.00504550866506663,-0.0384949409309736,
-0.0109620776735448));
#19113=CARTESIAN_POINT('Ctrl Pts',(0.0049665555155074,-0.0385008022567649,
-0.0110291836133958));
#19114=CARTESIAN_POINT('Ctrl Pts',(0.00493367576372713,-0.0385033029436651,
-0.0110596938369025));
#19115=CARTESIAN_POINT('Ctrl Pts',(0.00487897702943803,-0.0385075531204408,
-0.0111150772351447));
#19116=CARTESIAN_POINT('Ctrl Pts',(0.00485654292742318,-0.0385093258457484,
-0.0111392991518396));
#19117=CARTESIAN_POINT('Ctrl Pts',(0.00482384759768811,-0.0385119554977753,
-0.0111769544901834));
#19118=CARTESIAN_POINT('Ctrl Pts',(0.00481300252016924,-0.0385128360635772,
-0.011189866323279));
#19119=CARTESIAN_POINT('Ctrl Pts',(0.00479352285001517,-0.0385144338525416,
-0.011213845589403));
#19120=CARTESIAN_POINT('Ctrl Pts',(0.00478482356381312,-0.0385151536248163,
-0.0112248579296845));
#19121=CARTESIAN_POINT('Ctrl Pts',(0.00476598893787307,-0.0385167266465979,
-0.0112493810020078));
#19122=CARTESIAN_POINT('Ctrl Pts',(0.00475592268616921,-0.0385175771543972,
-0.0112629426330942));
#19123=CARTESIAN_POINT('Ctrl Pts',(0.0047273722585249,-0.0385200206908794,
-0.0113027563338989));
#19124=CARTESIAN_POINT('Ctrl Pts',(0.00470948177230987,-0.0385215915557718,
-0.0113294240021196));
#19125=CARTESIAN_POINT('Ctrl Pts',(0.00462769671452698,-0.0385290080137881,
-0.0114599616109227));
#19126=CARTESIAN_POINT('Ctrl Pts',(0.00457543705715437,-0.0385344496172467,
-0.0115705952591806));
#19127=CARTESIAN_POINT('Ctrl Pts',(0.00451903842397314,-0.038542701158159,
-0.0117391434862632));
#19128=CARTESIAN_POINT('Ctrl Pts',(0.00450421677859805,-0.0385453389011639,
-0.0117929770926619));
#19129=CARTESIAN_POINT('Ctrl Pts',(0.00448945009426728,-0.038548789645804,
-0.0118607772532303));
#19130=CARTESIAN_POINT('Ctrl Pts',(0.00448673205127474,-0.0385494739204851,
-0.0118741017065303));
#19131=CARTESIAN_POINT('Ctrl Pts',(0.00448261115053832,-0.0385505986238379,
-0.0118957613584947));
#19132=CARTESIAN_POINT('Ctrl Pts',(0.0044810999946702,-0.0385510332852672,
-0.0119040754788661));
#19133=CARTESIAN_POINT('Ctrl Pts',(0.00447820165603089,-0.0385519143533416,
-0.0119208013739311));
#19134=CARTESIAN_POINT('Ctrl Pts',(0.00447681574874125,-0.0385523608031171,
-0.0119292130469584));
#19135=CARTESIAN_POINT('Ctrl Pts',(0.00447334572397001,-0.038553547455177,
-0.0119514198506197));
#19136=CARTESIAN_POINT('Ctrl Pts',(0.00447137892316355,-0.0385542936799903,
-0.0119652322461774));
#19137=CARTESIAN_POINT('Ctrl Pts',(0.00446201690499842,-0.0385582632002159,
-0.0120380410557255));
#19138=CARTESIAN_POINT('Ctrl Pts',(0.00445784960596041,-0.0385616215559427,
-0.012097397814629));
#19139=CARTESIAN_POINT('Ctrl Pts',(0.00445703903398348,-0.0385653806389522,
-0.0121631792977559));
#19140=CARTESIAN_POINT('Ctrl Pts',(0.00445700000004407,-0.0385657431904327,
-0.012169516646089));
#19141=CARTESIAN_POINT('Ctrl Pts',(0.004457,-0.0385661060144854,-0.0121758532758267));
#19142=CARTESIAN_POINT('Ctrl Pts',(0.004457,-0.0386811151660051,-0.0121758532865598));
#19143=CARTESIAN_POINT('Ctrl Pts',(0.004457,-0.0386810906944945,-0.0121753703966079));
#19144=CARTESIAN_POINT('Ctrl Pts',(0.00445700022668442,-0.038681066229755,
-0.0121748875055352));
#19145=CARTESIAN_POINT('Ctrl Pts',(0.00445701898307565,-0.0386800543821255,
-0.0121549098447703));
#19146=CARTESIAN_POINT('Ctrl Pts',(0.00445740673902861,-0.0386790782088258,
-0.0121354166724654));
#19147=CARTESIAN_POINT('Ctrl Pts',(0.00446002368905376,-0.0386757399764894,
-0.0120680759099084));
#19148=CARTESIAN_POINT('Ctrl Pts',(0.0044641110029321,-0.0386734334027347,
-0.0120203268189988));
#19149=CARTESIAN_POINT('Ctrl Pts',(0.0044811533560549,-0.0386673151593163,
-0.0118919211402397));
#19150=CARTESIAN_POINT('Ctrl Pts',(0.00449829838744569,-0.038663602515764,
-0.0118119780953627));
#19151=CARTESIAN_POINT('Ctrl Pts',(0.00454032753398168,-0.0386568328281487,
-0.0116714346343537));
#19152=CARTESIAN_POINT('Ctrl Pts',(0.0045628904833326,-0.0386537995783954,
-0.0116103474851028));
#19153=CARTESIAN_POINT('Ctrl Pts',(0.00459627983317719,-0.038649743129664,
-0.0115349781969822));
#19154=CARTESIAN_POINT('Ctrl Pts',(0.00460358873369526,-0.0386488759106765,
-0.0115192051946177));
#19155=CARTESIAN_POINT('Ctrl Pts',(0.00461525587475696,-0.0386475174485943,
-0.0114951029794756));
#19156=CARTESIAN_POINT('Ctrl Pts',(0.00461942654438151,-0.0386470365716885,
-0.0114866840779813));
#19157=CARTESIAN_POINT('Ctrl Pts',(0.00462744876830709,-0.0386461194342514,
-0.0114708555227298));
#19158=CARTESIAN_POINT('Ctrl Pts',(0.00463128399556532,-0.0386456841013622,
-0.0114634382261798));
#19159=CARTESIAN_POINT('Ctrl Pts',(0.0046408662321122,-0.0386446044985353,
-0.0114452692562471));
#19160=CARTESIAN_POINT('Ctrl Pts',(0.00464668076766474,-0.0386439563275059,
-0.0114345539800513));
#19161=CARTESIAN_POINT('Ctrl Pts',(0.00466994530470803,-0.0386413928391975,
-0.011392867194935));
#19162=CARTESIAN_POINT('Ctrl Pts',(0.00468833565358654,-0.0386394301784478,
-0.0113624351703959));
#19163=CARTESIAN_POINT('Ctrl Pts',(0.00474538677056307,-0.0386335759106839,
-0.0112750003716201));
#19164=CARTESIAN_POINT('Ctrl Pts',(0.00478683149534427,-0.0386296099623235,
-0.0112199180655523));
#19165=CARTESIAN_POINT('Ctrl Pts',(0.00488786551499036,-0.0386207736175767,
-0.0111028358377403));
#19166=CARTESIAN_POINT('Ctrl Pts',(0.0049492407491786,-0.0386159412703069,
-0.0110426641657795));
#19167=CARTESIAN_POINT('Ctrl Pts',(0.00503540683196787,-0.0386099075370377,
-0.0109712410551507));
#19168=CARTESIAN_POINT('Ctrl Pts',(0.00505592735877954,-0.0386085190153877,
-0.0109550922271287));
#19169=CARTESIAN_POINT('Ctrl Pts',(0.0050895381809652,-0.0386063202886948,
-0.0109299965250387));
#19170=CARTESIAN_POINT('Ctrl Pts',(0.00510237311183476,-0.03860549760612,
-0.0109207175217214));
#19171=CARTESIAN_POINT('Ctrl Pts',(0.00512738109421129,-0.0386039263137975,
-0.0109032178680065));
#19172=CARTESIAN_POINT('Ctrl Pts',(0.0051395330868172,-0.0386031767486838,
-0.0108949702420811));
#19173=CARTESIAN_POINT('Ctrl Pts',(0.00516842038676475,-0.0386014265189701,
-0.0108759609279524));
#19174=CARTESIAN_POINT('Ctrl Pts',(0.00518524991377004,-0.0386004312670951,
-0.0108653468429247));
#19175=CARTESIAN_POINT('Ctrl Pts',(0.00524598884131841,-0.0385969203903979,
-0.0108286623292766));
#19176=CARTESIAN_POINT('Ctrl Pts',(0.00529098249205345,-0.0385944688565585,
-0.0108044485123423));
#19177=CARTESIAN_POINT('Ctrl Pts',(0.00542116620066221,-0.0385876819934572,
-0.0107425117863365));
#19178=CARTESIAN_POINT('Ctrl Pts',(0.00550868046125469,-0.0385834804678757,
-0.0107102062432397));
#19179=CARTESIAN_POINT('Ctrl Pts',(0.0056522537860829,-0.0385765629595163,
-0.0106715220432754));
#19180=CARTESIAN_POINT('Ctrl Pts',(0.00570667387554513,-0.0385739318653432,
-0.0106599711247281));
#19181=CARTESIAN_POINT('Ctrl Pts',(0.00577540714706734,-0.0385704733419115,
-0.0106492221815898));
#19182=CARTESIAN_POINT('Ctrl Pts',(0.00578924895542135,-0.0385697700165762,
-0.0106472498546131));
#19183=CARTESIAN_POINT('Ctrl Pts',(0.00581173107477527,-0.0385686139221144,
-0.0106443575230082));
#19184=CARTESIAN_POINT('Ctrl Pts',(0.00582035599972359,-0.0385681671369668,
-0.0106433218873311));
#19185=CARTESIAN_POINT('Ctrl Pts',(0.00583775238339277,-0.0385672585985931,
-0.0106413818916083));
#19186=CARTESIAN_POINT('Ctrl Pts',(0.00584652372553353,-0.038566796758713,
-0.0106404797890516));
#19187=CARTESIAN_POINT('Ctrl Pts',(0.00586983984868978,-0.038565560010558,
-0.0106382835951181));
#19188=CARTESIAN_POINT('Ctrl Pts',(0.00588439580153568,-0.0385647785615512,
-0.0106371207364495));
#19189=CARTESIAN_POINT('Ctrl Pts',(0.00598057757042034,-0.0385595628500035,
-0.0106308092832336));
#19190=CARTESIAN_POINT('Ctrl Pts',(0.00606248057391231,-0.0385548808666727,
-0.0106319515709773));
#19191=CARTESIAN_POINT('Ctrl Pts',(0.00624770547829795,-0.0385442291220978,
-0.0106493012700618));
#19192=CARTESIAN_POINT('Ctrl Pts',(0.00635027096222377,-0.0385382996144999,
-0.0106695218005934));
#19193=CARTESIAN_POINT('Ctrl Pts',(0.00647462339648171,-0.0385312961124019,
-0.0107074381061901));
#19194=CARTESIAN_POINT('Ctrl Pts',(0.00649903452250175,-0.0385299290253567,
-0.0107155536052064));
#19195=CARTESIAN_POINT('Ctrl Pts',(0.00653805816088472,-0.0385277555103609,
-0.0107296199793372));
#19196=CARTESIAN_POINT('Ctrl Pts',(0.00655280155367318,-0.0385269371140008,
-0.0107351909979931));
#19197=CARTESIAN_POINT('Ctrl Pts',(0.00658114169539628,-0.0385253687222763,
-0.0107463988877147));
#19198=CARTESIAN_POINT('Ctrl Pts',(0.0065947481774895,-0.0385246178696821,
-0.0107520063239256));
#19199=CARTESIAN_POINT('Ctrl Pts',(0.00662674181885426,-0.0385228565068216,
-0.0107657300416678));
#19200=CARTESIAN_POINT('Ctrl Pts',(0.00664505491347601,-0.0385218516205357,
-0.0107740126829648));
#19201=CARTESIAN_POINT('Ctrl Pts',(0.00671084148448894,-0.0385182486334197,
-0.0108053288480932));
#19202=CARTESIAN_POINT('Ctrl Pts',(0.00675728896990039,-0.0385157195077449,
-0.010830436289441));
#19203=CARTESIAN_POINT('Ctrl Pts',(0.00688804394130476,-0.0385085251748819,
-0.0109100376374027));
#19204=CARTESIAN_POINT('Ctrl Pts',(0.00696843179801197,-0.0385040185832347,
-0.0109704279504564));
#19205=CARTESIAN_POINT('Ctrl Pts',(0.00707706949285719,-0.038497115150683,
-0.0110699677334163));
#19206=CARTESIAN_POINT('Ctrl Pts',(0.00711027709992211,-0.0384948693345765,
-0.0111033115976393));
#19207=CARTESIAN_POINT('Ctrl Pts',(0.00715102546269945,-0.0384918528828708,
-0.0111481504177021));
#19208=CARTESIAN_POINT('Ctrl Pts',(0.00716001048437217,-0.0384911700730022,
-0.0111583030640487));
#19209=CARTESIAN_POINT('Ctrl Pts',(0.00717392051151227,-0.0384900824173775,
-0.0111744444197034));
#19210=CARTESIAN_POINT('Ctrl Pts',(0.00717893632777092,-0.038489683762633,
-0.0111803543081208));
#19211=CARTESIAN_POINT('Ctrl Pts',(0.00718946695720243,-0.0384888323939499,
-0.0111929532348859));
#19212=CARTESIAN_POINT('Ctrl Pts',(0.00719497029626112,-0.0384883788651668,
-0.0111996513934755));
#19213=CARTESIAN_POINT('Ctrl Pts',(0.00720914705712648,-0.0384871887567263,
-0.0112172055552576));
#19214=CARTESIAN_POINT('Ctrl Pts',(0.00721773066450816,-0.0384864464365653,
-0.0112281328206827));
#19215=CARTESIAN_POINT('Ctrl Pts',(0.0072610648383999,-0.0384825917041162,
-0.0112848596707859));
#19216=CARTESIAN_POINT('Ctrl Pts',(0.00729338135720757,-0.0384793551753168,
-0.0113324566991023));
#19217=CARTESIAN_POINT('Ctrl Pts',(0.00739175791517952,-0.0384684656206931,
-0.0114963488249175));
#19218=CARTESIAN_POINT('Ctrl Pts',(0.00744538020307464,-0.0384607488976567,
-0.0116194331818831));
#19219=CARTESIAN_POINT('Ctrl Pts',(0.00748907988097694,-0.03845229313773,
-0.0117708114008163));
#19220=CARTESIAN_POINT('Ctrl Pts',(0.0074951628086487,-0.0384510292650615,
-0.0117938767432119));
#19221=CARTESIAN_POINT('Ctrl Pts',(0.00750428745822559,-0.0384489772655672,
-0.0118320435767394));
#19222=CARTESIAN_POINT('Ctrl Pts',(0.00750764202389111,-0.0384481795149103,
-0.0118470654770381));
#19223=CARTESIAN_POINT('Ctrl Pts',(0.00751380297430129,-0.0384466226588566,
-0.0118767347703391));
#19224=CARTESIAN_POINT('Ctrl Pts',(0.00751662287294446,-0.0384458632078929,
-0.0118913776059936));
#19225=CARTESIAN_POINT('Ctrl Pts',(0.00752295184845898,-0.0384440352975894,
-0.0119270165481736));
#19226=CARTESIAN_POINT('Ctrl Pts',(0.00752623961227817,-0.0384429737349884,
-0.0119480490830947));
#19227=CARTESIAN_POINT('Ctrl Pts',(0.00753776449116768,-0.0384387328826291,
-0.0120333019281696));
#19228=CARTESIAN_POINT('Ctrl Pts',(0.00754239164164807,-0.0384356623039623,
-0.0120979459014267));
#19229=CARTESIAN_POINT('Ctrl Pts',(0.00754363468893113,-0.0384288801778244,
-0.0122436876370925));
#19230=CARTESIAN_POINT('Ctrl Pts',(0.00753794702050676,-0.0384252136974585,
-0.0123246083203443));
#19231=CARTESIAN_POINT('Ctrl Pts',(0.00751836782412125,-0.0384190508880638,
-0.0124551570964609));
#19232=CARTESIAN_POINT('Ctrl Pts',(0.00750830472959757,-0.0384166255455801,
-0.0125051973739129));
#19233=CARTESIAN_POINT('Ctrl Pts',(0.00749239341269471,-0.0384134014665868,
-0.0125680287095958));
#19234=CARTESIAN_POINT('Ctrl Pts',(0.00748882428324351,-0.038412706529619,
-0.0125813676387868));
#19235=CARTESIAN_POINT('Ctrl Pts',(0.00748296028901683,-0.0384116042684971,
-0.0126021613730741));
#19236=CARTESIAN_POINT('Ctrl Pts',(0.0074807870229216,-0.0384112034259478,
-0.0126096500029412));
#19237=CARTESIAN_POINT('Ctrl Pts',(0.00747609314404917,-0.0384103527857387,
-0.0126253777735206));
#19238=CARTESIAN_POINT('Ctrl Pts',(0.0074735601277721,-0.0384099022510064,
-0.0126336128024261));
#19239=CARTESIAN_POINT('Ctrl Pts',(0.00746684072127418,-0.0384087292471139,
-0.0126548242779768));
#19240=CARTESIAN_POINT('Ctrl Pts',(0.00746255110138742,-0.0384080013250164,
-0.0126677670631409));
#19241=CARTESIAN_POINT('Ctrl Pts',(0.0074408399556796,-0.0384044205694814,
-0.0127304789707125));
#19242=CARTESIAN_POINT('Ctrl Pts',(0.00742104758291845,-0.0384014631435197,
-0.0127793865148959));
#19243=CARTESIAN_POINT('Ctrl Pts',(0.00736529235336711,-0.0383939560477157,
-0.0128991265612218));
#19244=CARTESIAN_POINT('Ctrl Pts',(0.00732628962771408,-0.0383893728985182,
-0.0129683833886149));
#19245=CARTESIAN_POINT('Ctrl Pts',(0.00724634686018956,-0.0383812672313015,
-0.0130877773319307));
#19246=CARTESIAN_POINT('Ctrl Pts',(0.00720725222068425,-0.0383777145492173,
-0.0131389366030628));
#19247=CARTESIAN_POINT('Ctrl Pts',(0.00715092324530721,-0.038373127256583,
-0.0132038078279602));
#19248=CARTESIAN_POINT('Ctrl Pts',(0.00713643122051977,-0.0383719881826513,
-0.0132198068288556));
#19249=CARTESIAN_POINT('Ctrl Pts',(0.00711143400935017,-0.0383700903919216,
-0.0132462657837207));
#19250=CARTESIAN_POINT('Ctrl Pts',(0.00710110544148126,-0.0383693245276794,
-0.0132568876513459));
#19251=CARTESIAN_POINT('Ctrl Pts',(0.00707981369716824,-0.038367781699566,
-0.0132781622136346));
#19252=CARTESIAN_POINT('Ctrl Pts',(0.00706884199125089,-0.0383670052388432,
-0.0132888040537846));
#19253=CARTESIAN_POINT('Ctrl Pts',(0.00704075054521407,-0.0383650621557736,
-0.0133152523047962));
#19254=CARTESIAN_POINT('Ctrl Pts',(0.00702342731511748,-0.0383639047241738,
-0.0133308374512071));
#19255=CARTESIAN_POINT('Ctrl Pts',(0.0069334747876976,-0.0383580856871029,
-0.0134081512445624));
#19256=CARTESIAN_POINT('Ctrl Pts',(0.00685558748736433,-0.0383536792434703,
-0.0134634500480332));
#19257=CARTESIAN_POINT('Ctrl Pts',(0.00669340759837118,-0.038345062373516,
-0.0135573426541664));
#19258=CARTESIAN_POINT('Ctrl Pts',(0.00660976051664869,-0.0383408620440565,
-0.013596246142168));
#19259=CARTESIAN_POINT('Ctrl Pts',(0.00650761428110306,-0.0383355062967678,
-0.0136330593876282));
#19260=CARTESIAN_POINT('Ctrl Pts',(0.00649198529757305,-0.0383346806024656,
-0.0136384100568866));
#19261=CARTESIAN_POINT('Ctrl Pts',(0.00646750524636395,-0.0383333733942934,
-0.0136463541649019));
#19262=CARTESIAN_POINT('Ctrl Pts',(0.00645871136508243,-0.0383329010449012,
-0.0136491210368244));
#19263=CARTESIAN_POINT('Ctrl Pts',(0.00644183622826642,-0.0383319884338862,
-0.0136542648319799));
#19264=CARTESIAN_POINT('Ctrl Pts',(0.00643375944569259,-0.0383315488717997,
-0.0136566546513163));
#19265=CARTESIAN_POINT('Ctrl Pts',(0.00641352915153954,-0.0383304415807624,
-0.0136624608403344));
#19266=CARTESIAN_POINT('Ctrl Pts',(0.00640135261775309,-0.038329769491082,
-0.0136657943708276));
#19267=CARTESIAN_POINT('Ctrl Pts',(0.00635071716163203,-0.038326955377435,
-0.013678990941803));
#19268=CARTESIAN_POINT('Ctrl Pts',(0.00631192769250872,-0.0383247540837484,
-0.013687516617592));
#19269=CARTESIAN_POINT('Ctrl Pts',(0.00618803528889515,-0.0383176665934017,
-0.0137097758541176));
#19270=CARTESIAN_POINT('Ctrl Pts',(0.00610208777855087,-0.0383126754488808,
-0.0137178825066896));
#19271=CARTESIAN_POINT('Ctrl Pts',(0.00594452091180687,-0.0383037460751729,
-0.0137195074967112));
#19272=CARTESIAN_POINT('Ctrl Pts',(0.00587315880430296,-0.0382997829439983,
-0.0137152880800327));
#19273=CARTESIAN_POINT('Ctrl Pts',(0.00578037711294673,-0.0382947811978246,
-0.0137033038236897));
#19274=CARTESIAN_POINT('Ctrl Pts',(0.00575847849812121,-0.0382936112973411,
-0.0136999946141831));
#19275=CARTESIAN_POINT('Ctrl Pts',(0.00572329557706447,-0.0382917481804231,
-0.0136939005755142));
#19276=CARTESIAN_POINT('Ctrl Pts',(0.00570996406048768,-0.038291046040352,
-0.0136914099757818));
#19277=CARTESIAN_POINT('Ctrl Pts',(0.00568203656896372,-0.0382895827504961,
-0.0136858105394262));
#19278=CARTESIAN_POINT('Ctrl Pts',(0.00566744932395982,-0.0382888228225961,
-0.0136826650587088));
#19279=CARTESIAN_POINT('Ctrl Pts',(0.00563211085905527,-0.0382869914718425,
-0.0136745067575425));
#19280=CARTESIAN_POINT('Ctrl Pts',(0.00561141336080147,-0.0382859270123157,
-0.0136692738986096));
#19281=CARTESIAN_POINT('Ctrl Pts',(0.00552769350396161,-0.038281647378967,
-0.0136462489348721));
#19282=CARTESIAN_POINT('Ctrl Pts',(0.00546572260379649,-0.0382785436854398,
-0.0136248824427185));
#19283=CARTESIAN_POINT('Ctrl Pts',(0.00535108239995343,-0.0382727653424974,
-0.013576997988481));
#19284=CARTESIAN_POINT('Ctrl Pts',(0.00529820874002883,-0.0382700832500512,
-0.0135512767123211));
#19285=CARTESIAN_POINT('Ctrl Pts',(0.00518950682885686,-0.0382643374613907,
-0.0134904933150084));
#19286=CARTESIAN_POINT('Ctrl Pts',(0.00513419949053004,-0.0382612721988115,
-0.0134547456652044));
#19287=CARTESIAN_POINT('Ctrl Pts',(0.00506735007849969,-0.0382571783445711,
-0.0134052094641428));
#19288=CARTESIAN_POINT('Ctrl Pts',(0.00505353039273019,-0.0382563093329121,
-0.0133946017117112));
#19289=CARTESIAN_POINT('Ctrl Pts',(0.0050325329023907,-0.0382549486598804,
-0.0133779118666027));
#19290=CARTESIAN_POINT('Ctrl Pts',(0.0050252258157321,-0.0382544674180131,
-0.0133719940374326));
#19291=CARTESIAN_POINT('Ctrl Pts',(0.00501153456004873,-0.0382535500630858,
-0.0133606970568774));
#19292=CARTESIAN_POINT('Ctrl Pts',(0.00500513924416309,-0.0382531148871735,
-0.0133553323033181));
#19293=CARTESIAN_POINT('Ctrl Pts',(0.00498952463037424,-0.0382520363580196,
-0.0133420165423097));
#19294=CARTESIAN_POINT('Ctrl Pts',(0.0049803554012407,-0.03825138912159,
-0.0133340078902502));
#19295=CARTESIAN_POINT('Ctrl Pts',(0.00494489936074645,-0.0382488348100471,
-0.0133022922047216));
#19296=CARTESIAN_POINT('Ctrl Pts',(0.00491933805006229,-0.0382468808018378,
-0.0132777931333543));
#19297=CARTESIAN_POINT('Ctrl Pts',(0.00484698483815757,-0.038241066856399,
-0.0132035063153651));
#19298=CARTESIAN_POINT('Ctrl Pts',(0.00480262915094476,-0.0382371335511976,
-0.0131514645767921));
#19299=CARTESIAN_POINT('Ctrl Pts',(0.00471023087156845,-0.0382282851740607,
-0.0130272239135652));
#19300=CARTESIAN_POINT('Ctrl Pts',(0.00466452036365229,-0.0382234094264812,
-0.0129535637667349));
#19301=CARTESIAN_POINT('Ctrl Pts',(0.00461336822153091,-0.0382173358446065,
-0.0128531885450019));
#19302=CARTESIAN_POINT('Ctrl Pts',(0.00460210486739035,-0.0382159471816289,
-0.01282962698433));
#19303=CARTESIAN_POINT('Ctrl Pts',(0.00458497889799723,-0.0382137482881738,
-0.0127913328487209));
#19304=CARTESIAN_POINT('Ctrl Pts',(0.00457873618313873,-0.038212925576805,
-0.0127767767407702));
#19305=CARTESIAN_POINT('Ctrl Pts',(0.00456713872999419,-0.0382113542634237,
-0.0127485427654217));
#19306=CARTESIAN_POINT('Ctrl Pts',(0.00456175303948874,-0.0382106047054126,
-0.012734879545228));
#19307=CARTESIAN_POINT('Ctrl Pts',(0.00454953288070422,-0.0382088545437266,
-0.0127025314455793));
#19308=CARTESIAN_POINT('Ctrl Pts',(0.00454286302742768,-0.038207859351457,
-0.0126837869783028));
#19309=CARTESIAN_POINT('Ctrl Pts',(0.00452037622361846,-0.0382043490389647,
-0.0126164990860643));
#19310=CARTESIAN_POINT('Ctrl Pts',(0.00450660734237072,-0.0382018979803378,
-0.0125673046738582));
#19311=CARTESIAN_POINT('Ctrl Pts',(0.00446984551504731,-0.0381940821302627,
-0.0124054034729965));
#19312=CARTESIAN_POINT('Ctrl Pts',(0.00445700000000001,-0.0381889595111803,
-0.0122908068720926));
#19313=CARTESIAN_POINT('Ctrl Pts',(0.00445700000000001,-0.0381835089768636,
-0.0121758532865662));
#19314=CARTESIAN_POINT('Origin',(0.006,-0.0418165664398416,-0.0121758532865581));
#19315=CARTESIAN_POINT('',(0.004457,-0.0391830969990905,-0.0121758532988723));
#19316=CARTESIAN_POINT('',(0.004457,-0.0390679979850714,-0.0121758532865563));
#19317=CARTESIAN_POINT('',(0.004457,-0.0418165664398416,-0.0121758532865581));
#19318=CARTESIAN_POINT('Ctrl Pts',(0.004457,-0.0385661060144854,-0.0121758532758267));
#19319=CARTESIAN_POINT('Ctrl Pts',(0.00445699999940689,-0.0385709890096937,
-0.0122611335443476));
#19320=CARTESIAN_POINT('Ctrl Pts',(0.00446407020437146,-0.0385759100486242,
-0.0123462843053963));
#19321=CARTESIAN_POINT('Ctrl Pts',(0.00448649972637195,-0.0385834971460825,
-0.0124803692373493));
#19322=CARTESIAN_POINT('Ctrl Pts',(0.0044973078821122,-0.0385862646457588,
-0.0125298733343161));
#19323=CARTESIAN_POINT('Ctrl Pts',(0.00451562854401043,-0.0385899951329252,
-0.0125976012485272));
#19324=CARTESIAN_POINT('Ctrl Pts',(0.00452108232020828,-0.0385910216618756,
-0.0126163444961434));
#19325=CARTESIAN_POINT('Ctrl Pts',(0.00453114143214295,-0.0385927797623273,
-0.0126486192027317));
#19326=CARTESIAN_POINT('Ctrl Pts',(0.00453558175434474,-0.0385935165519015,
-0.0126621991755757));
#19327=CARTESIAN_POINT('Ctrl Pts',(0.00454515550583596,-0.0385950279652326,
-0.0126901581924258));
#19328=CARTESIAN_POINT('Ctrl Pts',(0.00455031503315732,-0.0385958016369882,
-0.0127045266798043));
#19329=CARTESIAN_POINT('Ctrl Pts',(0.00456439801452056,-0.0385978120297865,
-0.0127419882036284));
#19330=CARTESIAN_POINT('Ctrl Pts',(0.00457366560029978,-0.0385990373205938,
-0.0127649475653962));
#19331=CARTESIAN_POINT('Ctrl Pts',(0.00462835386203875,-0.038605773129083,
-0.0128915644051006));
#19332=CARTESIAN_POINT('Ctrl Pts',(0.00468451717056739,-0.0386109068707634,
-0.0129902009822645));
#19333=CARTESIAN_POINT('Ctrl Pts',(0.00478173699898775,-0.0386185122447016,
-0.0131242365729653));
#19334=CARTESIAN_POINT('Ctrl Pts',(0.00481464792204486,-0.038620934059732,
-0.0131650628337481));
#19335=CARTESIAN_POINT('Ctrl Pts',(0.00486980110266417,-0.038624892609201,
-0.0132267676745674));
#19336=CARTESIAN_POINT('Ctrl Pts',(0.00489069450856048,-0.038626372428177,
-0.0132487986324183));
#19337=CARTESIAN_POINT('Ctrl Pts',(0.00492028925441706,-0.0386284653192406,
-0.0132782157780816));
#19338=CARTESIAN_POINT('Ctrl Pts',(0.00492844389039881,-0.0386290416886927,
-0.0132861441701766));
#19339=CARTESIAN_POINT('Ctrl Pts',(0.00494251502703814,-0.0386300372444446,
-0.0132995255053569));
#19340=CARTESIAN_POINT('Ctrl Pts',(0.00494838797927676,-0.0386304530900695,
-0.013305023725347));
#19341=CARTESIAN_POINT('Ctrl Pts',(0.00496114237755294,-0.0386313573372578,
-0.0133167784946628));
#19342=CARTESIAN_POINT('Ctrl Pts',(0.00496803767863141,-0.0386318467872882,
-0.0133230190326023));
#19343=CARTESIAN_POINT('Ctrl Pts',(0.00498783179428647,-0.0386332524102091,
-0.0133406106623483));
#19344=CARTESIAN_POINT('Ctrl Pts',(0.00500086404683463,-0.0386341785355146,
-0.0133518088644727));
#19345=CARTESIAN_POINT('Ctrl Pts',(0.00506632977434108,-0.0386388223371126,
-0.013406187627188));
#19346=CARTESIAN_POINT('Ctrl Pts',(0.00512138492249497,-0.0386426981688242,
-0.0134460882935113));
#19347=CARTESIAN_POINT('Ctrl Pts',(0.00523284927792429,-0.0386502494071937,
-0.0135161485649029));
#19348=CARTESIAN_POINT('Ctrl Pts',(0.0052888657804517,-0.0386539152291565,
-0.0135466925845617));
#19349=CARTESIAN_POINT('Ctrl Pts',(0.00538403385103367,-0.0386598338242587,
-0.0135911769380323));
#19350=CARTESIAN_POINT('Ctrl Pts',(0.00542214445899041,-0.0386621283351545,
-0.0136071599186868));
#19351=CARTESIAN_POINT('Ctrl Pts',(0.00549005124991666,-0.0386660740632042,
-0.0136324837790437));
#19352=CARTESIAN_POINT('Ctrl Pts',(0.0055195742016699,-0.0386677440908403,
-0.0136424859457626));
#19353=CARTESIAN_POINT('Ctrl Pts',(0.00556518152021704,-0.0386702554322559,
-0.013656412239432));
#19354=CARTESIAN_POINT('Ctrl Pts',(0.00558105856779777,-0.0386711172737177,
-0.0136609829199271));
#19355=CARTESIAN_POINT('Ctrl Pts',(0.00561056007057306,-0.0386726964271143,
-0.013668965034545));
#19356=CARTESIAN_POINT('Ctrl Pts',(0.0056241634606518,-0.0386734159411043,
-0.0136724471069856));
#19357=CARTESIAN_POINT('Ctrl Pts',(0.00565459118928566,-0.0386750068497171,
-0.0136797946695633));
#19358=CARTESIAN_POINT('Ctrl Pts',(0.00567143679205483,-0.0386758751263171,
-0.0136835645250743));
#19359=CARTESIAN_POINT('Ctrl Pts',(0.00571508025521172,-0.0386780946783948,
-0.0136925652071506));
#19360=CARTESIAN_POINT('Ctrl Pts',(0.00574196045330526,-0.0386794326957031,
-0.0136973689817397));
#19361=CARTESIAN_POINT('Ctrl Pts',(0.00588340840946179,-0.0386863462829957,
-0.0137187905608759));
#19362=CARTESIAN_POINT('Ctrl Pts',(0.00599944489334954,-0.0386915492269238,
-0.0137231895023478));
#19363=CARTESIAN_POINT('Ctrl Pts',(0.00615886669417164,-0.0386989277351179,
-0.0137112866322648));
#19364=CARTESIAN_POINT('Ctrl Pts',(0.00620268554574487,-0.0387009846113517,
-0.0137061187499411));
#19365=CARTESIAN_POINT('Ctrl Pts',(0.00627312582169957,-0.0387044162589633,
-0.0136947325092945));
#19366=CARTESIAN_POINT('Ctrl Pts',(0.00629990974056779,-0.0387057509541106,
-0.013689671570812));
#19367=CARTESIAN_POINT('Ctrl Pts',(0.00633723965334561,-0.0387076703018036,
-0.0136815883810114));
#19368=CARTESIAN_POINT('Ctrl Pts',(0.00634790997282678,-0.0387082257699806,
-0.0136791587765198));
#19369=CARTESIAN_POINT('Ctrl Pts',(0.00636632852791285,-0.0387091978497788,
-0.0136747583253562));
#19370=CARTESIAN_POINT('Ctrl Pts',(0.00637408875552441,-0.038709611556863,
-0.0136728404295587));
#19371=CARTESIAN_POINT('Ctrl Pts',(0.0063910902895269,-0.0387105273822365,
-0.0136684981377507));
#19372=CARTESIAN_POINT('Ctrl Pts',(0.00640032411273534,-0.038711030826235,
-0.0136660481939017));
#19373=CARTESIAN_POINT('Ctrl Pts',(0.00642783914953927,-0.0387125478352314,
-0.0136584736425784));
#19374=CARTESIAN_POINT('Ctrl Pts',(0.00644604861426834,-0.0387135741067202,
-0.0136530973522419));
#19375=CARTESIAN_POINT('Ctrl Pts',(0.0065909449017571,-0.0387218942948715,
-0.0136073939328253));
#19376=CARTESIAN_POINT('Ctrl Pts',(0.00671203570948084,-0.0387297391216645,
-0.0135511831346742));
#19377=CARTESIAN_POINT('Ctrl Pts',(0.00687358936273519,-0.0387404798493248,
-0.0134490671235244));
#19378=CARTESIAN_POINT('Ctrl Pts',(0.00692096071345067,-0.0387436781036921,
-0.0134152339094243));
#19379=CARTESIAN_POINT('Ctrl Pts',(0.00698217785597301,-0.0387478622631298,
-0.0133660590619536));
#19380=CARTESIAN_POINT('Ctrl Pts',(0.00699778998668464,-0.0387489344797945,
-0.0133530016730107));
#19381=CARTESIAN_POINT('Ctrl Pts',(0.00702401756165004,-0.0387507453647904,
-0.0133301691165515));
#19382=CARTESIAN_POINT('Ctrl Pts',(0.00703476228085287,-0.038751490119866,
-0.0133205471507517));
#19383=CARTESIAN_POINT('Ctrl Pts',(0.00705509168999932,-0.0387529053898367,
-0.0133018218447952));
#19384=CARTESIAN_POINT('Ctrl Pts',(0.00706469735771112,-0.0387535768441155,
-0.0132927432627463));
#19385=CARTESIAN_POINT('Ctrl Pts',(0.00708982335245743,-0.0387553413827213,
-0.01326837723697));
#19386=CARTESIAN_POINT('Ctrl Pts',(0.00710513885758565,-0.0387564254201723,
-0.0132528823882556));
#19387=CARTESIAN_POINT('Ctrl Pts',(0.00716852236978042,-0.0387609565345682,
-0.0131859805195332));
#19388=CARTESIAN_POINT('Ctrl Pts',(0.00721337401237781,-0.0387642709580579,
-0.0131316389823852));
#19389=CARTESIAN_POINT('Ctrl Pts',(0.00730015746286802,-0.0387711620494802,
-0.0130104931506991));
#19390=CARTESIAN_POINT('Ctrl Pts',(0.00734099756007175,-0.0387747134378307,
-0.0129431590276437));
#19391=CARTESIAN_POINT('Ctrl Pts',(0.0073915657781781,-0.0387799400909755,
-0.0128433123926883));
#19392=CARTESIAN_POINT('Ctrl Pts',(0.00740563960438962,-0.0387815157303427,
-0.0128131397834844));
#19393=CARTESIAN_POINT('Ctrl Pts',(0.00742760053641603,-0.0387842272089786,
-0.0127617842941983));
#19394=CARTESIAN_POINT('Ctrl Pts',(0.00743601816660517,-0.0387853410720547,
-0.0127408401603902));
#19395=CARTESIAN_POINT('Ctrl Pts',(0.00744756924535867,-0.0387869937780881,
-0.0127101718977647));
#19396=CARTESIAN_POINT('Ctrl Pts',(0.00745107059966241,-0.038787513246508,
-0.0127005886506733));
#19397=CARTESIAN_POINT('Ctrl Pts',(0.00745713106761091,-0.0387884473550531,
-0.0126834764499495));
#19398=CARTESIAN_POINT('Ctrl Pts',(0.00745972741642108,-0.0387888598714829,
-0.0126759613633439));
#19399=CARTESIAN_POINT('Ctrl Pts',(0.00746550480500243,-0.0387898065931268,
-0.0126588104529277));
#19400=CARTESIAN_POINT('Ctrl Pts',(0.00746864896773013,-0.0387903427754529,
-0.0126491630759093));
#19401=CARTESIAN_POINT('Ctrl Pts',(0.00747838156524733,-0.038792069818363,
-0.0126182691130563));
#19402=CARTESIAN_POINT('Ctrl Pts',(0.00748460556736955,-0.0387932787701087,
-0.012596911512547));
#19403=CARTESIAN_POINT('Ctrl Pts',(0.00749827381271102,-0.0387961878758144,
-0.0125459305990151));
#19404=CARTESIAN_POINT('Ctrl Pts',(0.00750530440886435,-0.0387979023701727,
-0.0125162062061284));
#19405=CARTESIAN_POINT('Ctrl Pts',(0.0075322339012315,-0.0388054921279668,
-0.0123850942017186));
#19406=CARTESIAN_POINT('Ctrl Pts',(0.00754280473558756,-0.0388115056641097,
-0.0122820531008686));
#19407=CARTESIAN_POINT('Ctrl Pts',(0.00754309520517498,-0.0388202263478965,
-0.0121262124846427));
#19408=CARTESIAN_POINT('Ctrl Pts',(0.00754051191508808,-0.0388231043212167,
-0.0120737215490195));
#19409=CARTESIAN_POINT('Ctrl Pts',(0.00753323443262685,-0.0388269784654415,
-0.0120013555296904));
#19410=CARTESIAN_POINT('Ctrl Pts',(0.00753081780543674,-0.0388280427772368,
-0.0119812917520572));
#19411=CARTESIAN_POINT('Ctrl Pts',(0.00752602536084484,-0.0388298370575668,
-0.0119471639639889));
#19412=CARTESIAN_POINT('Ctrl Pts',(0.00752384744410326,-0.0388305730851583,
-0.0119330752123572));
#19413=CARTESIAN_POINT('Ctrl Pts',(0.00751897683311214,-0.038832071375265,
-0.0119042220097796));
#19414=CARTESIAN_POINT('Ctrl Pts',(0.00751626335299476,-0.0388328328978096,
-0.0118894625834476));
#19415=CARTESIAN_POINT('Ctrl Pts',(0.00750875871866872,-0.0388347675688254,
-0.0118517452036579));
#19416=CARTESIAN_POINT('Ctrl Pts',(0.0075036586387808,-0.0388359309165052,
-0.0118288522911677));
#19417=CARTESIAN_POINT('Ctrl Pts',(0.00749131984209509,-0.0388384525972845,
-0.0117788644196382));
#19418=CARTESIAN_POINT('Ctrl Pts',(0.00748386033510217,-0.0388398040659622,
-0.0117518324829939));
#19419=CARTESIAN_POINT('Ctrl Pts',(0.00745785475387192,-0.0388440394432382,
-0.0116667113819958));
#19420=CARTESIAN_POINT('Ctrl Pts',(0.00743660076830057,-0.0388468529650445,
-0.01160951001503));
#19421=CARTESIAN_POINT('Ctrl Pts',(0.00737129899910049,-0.0388542840793461,
-0.0114612999156701));
#19422=CARTESIAN_POINT('Ctrl Pts',(0.00732161082864321,-0.0388588484769401,
-0.0113731154636837));
#19423=CARTESIAN_POINT('Ctrl Pts',(0.00725472005643039,-0.0388646081950955,
-0.0112776495257963));
#19424=CARTESIAN_POINT('Ctrl Pts',(0.0072455742501692,-0.0388653891644274,
-0.0112650090800789));
#19425=CARTESIAN_POINT('Ctrl Pts',(0.00723092857219079,-0.0388666333593654,
-0.0112454003897197));
#19426=CARTESIAN_POINT('Ctrl Pts',(0.00722555735664718,-0.0388670883651384,
-0.0112383369393916));
#19427=CARTESIAN_POINT('Ctrl Pts',(0.00721510315753404,-0.0388679723195448,
-0.011224832448114));
#19428=CARTESIAN_POINT('Ctrl Pts',(0.00721002923548567,-0.038868400688288,
-0.0112183849804889));
#19429=CARTESIAN_POINT('Ctrl Pts',(0.00719718326573156,-0.0388694830023113,
-0.0112023267076361));
#19430=CARTESIAN_POINT('Ctrl Pts',(0.00718934676330783,-0.0388701412416195,
-0.0111927683312699));
#19431=CARTESIAN_POINT('Ctrl Pts',(0.00715630001500794,-0.0388729050837193,
-0.0111534338916031));
#19432=CARTESIAN_POINT('Ctrl Pts',(0.00713008121286506,-0.0388750693167788,
-0.0111245268969704));
#19433=CARTESIAN_POINT('Ctrl Pts',(0.00704457501190154,-0.0388819596506758,
-0.0110371516006546));
#19434=CARTESIAN_POINT('Ctrl Pts',(0.00698163427724544,-0.0388867894521148,
-0.0109824662078976));
#19435=CARTESIAN_POINT('Ctrl Pts',(0.00685258671293617,-0.0388959108445775,
-0.0108874932903238));
#19436=CARTESIAN_POINT('Ctrl Pts',(0.00678725015290552,-0.0389002032558147,
-0.0108465620415681));
#19437=CARTESIAN_POINT('Ctrl Pts',(0.00669965041806136,-0.0389055004582567,
-0.0108004178163234));
#19438=CARTESIAN_POINT('Ctrl Pts',(0.0066799590767812,-0.0389066639305614,
-0.0107905774437305));
#19439=CARTESIAN_POINT('Ctrl Pts',(0.00664675351842411,-0.0389085815847088,
-0.0107748623111406));
#19440=CARTESIAN_POINT('Ctrl Pts',(0.00663335402512636,-0.0389093436730812,
-0.0107687539561798));
#19441=CARTESIAN_POINT('Ctrl Pts',(0.00660647325525143,-0.0389108498348272,
-0.010756961759837));
#19442=CARTESIAN_POINT('Ctrl Pts',(0.00659299451386712,-0.0389115939160566,
-0.0107512759810167));
#19443=CARTESIAN_POINT('Ctrl Pts',(0.00655951499615744,-0.0389134158038965,
-0.0107377107357966));
#19444=CARTESIAN_POINT('Ctrl Pts',(0.00653942629226251,-0.0389144860878995,
-0.0107300558045623));
#19445=CARTESIAN_POINT('Ctrl Pts',(0.0064513003136744,-0.0389190904362821,
-0.0106985674348875));
#19446=CARTESIAN_POINT('Ctrl Pts',(0.00638179704600105,-0.038922483575283,
-0.0106790975315336));
#19447=CARTESIAN_POINT('Ctrl Pts',(0.0062520640856359,-0.0389286052075918,
-0.0106523849084008));
#19448=CARTESIAN_POINT('Ctrl Pts',(0.00619228260851654,-0.0389313482334985,
-0.0106436915670871));
#19449=CARTESIAN_POINT('Ctrl Pts',(0.00606794946760325,-0.038937108598694,
-0.0106330041327398));
#19450=CARTESIAN_POINT('Ctrl Pts',(0.0060034756409791,-0.0389401268100573,
-0.0106315129379326));
#19451=CARTESIAN_POINT('Ctrl Pts',(0.00592503700849566,-0.038944024268265,
-0.0106346110166826));
#19452=CARTESIAN_POINT('Ctrl Pts',(0.00591097889688837,-0.0389447317114968,
-0.010635359079631));
#19453=CARTESIAN_POINT('Ctrl Pts',(0.00588840061015893,-0.0389458850020985,
-0.0106368705991773));
#19454=CARTESIAN_POINT('Ctrl Pts',(0.00587987285156877,-0.0389463245241815,
-0.0106375127529518));
#19455=CARTESIAN_POINT('Ctrl Pts',(0.00586295445886242,-0.0389472050622727,
-0.0106389282668313));
#19456=CARTESIAN_POINT('Ctrl Pts',(0.0058545639783542,-0.0389476459604111,
-0.010639699533745));
#19457=CARTESIAN_POINT('Ctrl Pts',(0.00583276589652524,-0.0389488015840366,
-0.0106418834329746));
#19458=CARTESIAN_POINT('Ctrl Pts',(0.00581936994960617,-0.0389495218091572,
-0.0106434031184022));
#19459=CARTESIAN_POINT('Ctrl Pts',(0.00575274247265542,-0.038953148285221,
-0.0106518473104672));
#19460=CARTESIAN_POINT('Ctrl Pts',(0.00569988123357391,-0.0389561655704196,
-0.0106613704280882));
#19461=CARTESIAN_POINT('Ctrl Pts',(0.00557050287408348,-0.0389637370750815,
-0.010691718242654));
#19462=CARTESIAN_POINT('Ctrl Pts',(0.00549488185313838,-0.0389683233525499,
-0.010715722821767));
#19463=CARTESIAN_POINT('Ctrl Pts',(0.00536096561215517,-0.0389764913960077,
-0.0107698876742696));
#19464=CARTESIAN_POINT('Ctrl Pts',(0.00530209980568882,-0.0389801009721952,
-0.0107981591621908));
#19465=CARTESIAN_POINT('Ctrl Pts',(0.00522648360428544,-0.0389847333876129,
-0.0108405699293108));
#19466=CARTESIAN_POINT('Ctrl Pts',(0.00520799244010336,-0.0389858662553892,
-0.010851454047159));
#19467=CARTESIAN_POINT('Ctrl Pts',(0.00517853376536709,-0.0389876718274265,
-0.0108696314746269));
#19468=CARTESIAN_POINT('Ctrl Pts',(0.00516742256588606,-0.038988353046932,
-0.0108766854655964));
#19469=CARTESIAN_POINT('Ctrl Pts',(0.00514428430888205,-0.0389897724943307,
-0.0108917936601608));
#19470=CARTESIAN_POINT('Ctrl Pts',(0.00513227755707597,-0.0389905095610062,
-0.0108998767003045));
#19471=CARTESIAN_POINT('Ctrl Pts',(0.00510342650426437,-0.0389922828515013,
-0.0109198950610698));
#19472=CARTESIAN_POINT('Ctrl Pts',(0.00508670435504932,-0.0389933124888055,
-0.0109320019237646));
#19473=CARTESIAN_POINT('Ctrl Pts',(0.00502138082295572,-0.0389973484134285,
-0.0109813240610443));
#19474=CARTESIAN_POINT('Ctrl Pts',(0.00497476735735055,-0.0390002565183952,
-0.0110210829587258));
#19475=CARTESIAN_POINT('Ctrl Pts',(0.00488459170877782,-0.0390060806618378,
-0.0111077742178553));
#19476=CARTESIAN_POINT('Ctrl Pts',(0.00484133941089523,-0.0390089860105933,
-0.0111548565688351));
#19477=CARTESIAN_POINT('Ctrl Pts',(0.00475842328701149,-0.0390150419102517,
-0.0112571921418074));
#19478=CARTESIAN_POINT('Ctrl Pts',(0.00471924262128473,-0.0390181905573429,
-0.0113126556948978));
#19479=CARTESIAN_POINT('Ctrl Pts',(0.00467487551045286,-0.0390223694568305,
-0.0113851642352669));
#19480=CARTESIAN_POINT('Ctrl Pts',(0.0046661553351829,-0.0390232256846494,
-0.0113999651156102));
#19481=CARTESIAN_POINT('Ctrl Pts',(0.00465309842247589,-0.039024567756405,
-0.0114229976459652));
#19482=CARTESIAN_POINT('Ctrl Pts',(0.00464858576922245,-0.0390250433452285,
-0.0114311284759502));
#19483=CARTESIAN_POINT('Ctrl Pts',(0.00464030643252561,-0.0390259390929451,
-0.0114463691307259));
#19484=CARTESIAN_POINT('Ctrl Pts',(0.0046365214503827,-0.0390263581373064,
-0.0114534683714704));
#19485=CARTESIAN_POINT('Ctrl Pts',(0.00462751933855483,-0.0390273778066005,
-0.0114706758439578));
#19486=CARTESIAN_POINT('Ctrl Pts',(0.00462235821297537,-0.039027981696368,
-0.0114808126523283));
#19487=CARTESIAN_POINT('Ctrl Pts',(0.00460383053979049,-0.0390302193007762,
-0.0115182195407626));
#19488=CARTESIAN_POINT('Ctrl Pts',(0.00459115845480351,-0.0390318881039376,
-0.0115458242508556));
#19489=CARTESIAN_POINT('Ctrl Pts',(0.00455884783413799,-0.0390365098941275,
-0.0116220668213418));
#19490=CARTESIAN_POINT('Ctrl Pts',(0.00454086135863688,-0.0390395107402695,
-0.011671360465195));
#19491=CARTESIAN_POINT('Ctrl Pts',(0.00449211747054077,-0.0390490085595601,
-0.0118295464053845));
#19492=CARTESIAN_POINT('Ctrl Pts',(0.00447079264704203,-0.039055476574419,
-0.011940970585443));
#19493=CARTESIAN_POINT('Ctrl Pts',(0.00445988021919386,-0.0390628973623372,
-0.0120784200213759));
#19494=CARTESIAN_POINT('Ctrl Pts',(0.00445851487053123,-0.0390642125355577,
-0.0121031492952596));
#19495=CARTESIAN_POINT('Ctrl Pts',(0.0044572708178302,-0.039066308995255,
-0.0121431614622513));
#19496=CARTESIAN_POINT('Ctrl Pts',(0.00445702285893838,-0.0390671015028244,
-0.0121584277511109));
#19497=CARTESIAN_POINT('Ctrl Pts',(0.00445700050288177,-0.0390679240239845,
-0.0121744148175062));
#19498=CARTESIAN_POINT('Ctrl Pts',(0.004457,-0.0390679610123587,-0.01217513405244));
#19499=CARTESIAN_POINT('Ctrl Pts',(0.004457,-0.0390679979850714,-0.0121758532865546));
#19500=CARTESIAN_POINT('Ctrl Pts',(0.004457,-0.0391830969983919,-0.012175853298912));
#19501=CARTESIAN_POINT('Ctrl Pts',(0.00445699999984581,-0.0391820009249089,
-0.0121565951193162));
#19502=CARTESIAN_POINT('Ctrl Pts',(0.00445736054188219,-0.0391809001479444,
-0.0121373347547961));
#19503=CARTESIAN_POINT('Ctrl Pts',(0.00446239454806474,-0.0391732063147042,
-0.0120029760760998));
#19504=CARTESIAN_POINT('Ctrl Pts',(0.0044795837213134,-0.0391666246906011,
-0.0118886974964195));
#19505=CARTESIAN_POINT('Ctrl Pts',(0.0045156791125824,-0.0391591123637734,
-0.0117536643135762));
#19506=CARTESIAN_POINT('Ctrl Pts',(0.00452258626844821,-0.0391578095147989,
-0.0117300946277315));
#19507=CARTESIAN_POINT('Ctrl Pts',(0.00453477508548926,-0.0391557116223949,
-0.0116919048285094));
#19508=CARTESIAN_POINT('Ctrl Pts',(0.00453972000796917,-0.0391549060903489,
-0.0116771825254363));
#19509=CARTESIAN_POINT('Ctrl Pts',(0.00454981867969974,-0.0391533454327335,
-0.0116485555076253));
#19510=CARTESIAN_POINT('Ctrl Pts',(0.00455495225722688,-0.0391525897598165,
-0.0116346455168089));
#19511=CARTESIAN_POINT('Ctrl Pts',(0.00456776353850457,-0.0391507898485505,
-0.0116014145397136));
#19512=CARTESIAN_POINT('Ctrl Pts',(0.00457563287013562,-0.039149751968433,
-0.011582170302556));
#19513=CARTESIAN_POINT('Ctrl Pts',(0.00460741506568473,-0.0391458017171191,
-0.0115087208196458));
#19514=CARTESIAN_POINT('Ctrl Pts',(0.00463405400797084,-0.0391429786223235,
-0.0114557484994959));
#19515=CARTESIAN_POINT('Ctrl Pts',(0.00469533770478568,-0.0391372507995682,
-0.0113495868195775));
#19516=CARTESIAN_POINT('Ctrl Pts',(0.00473034776672741,-0.0391343594094087,
-0.0112967382120021));
#19517=CARTESIAN_POINT('Ctrl Pts',(0.00480979671359546,-0.0391282816728232,
-0.0111914947650657));
#19518=CARTESIAN_POINT('Ctrl Pts',(0.00485468212687263,-0.0391250968055734,
-0.0111396143930974));
#19519=CARTESIAN_POINT('Ctrl Pts',(0.0049152018054228,-0.0391208633551922,
-0.0110784154353194));
#19520=CARTESIAN_POINT('Ctrl Pts',(0.00492775274226097,-0.0391199882071065,
-0.0110661493929499));
#19521=CARTESIAN_POINT('Ctrl Pts',(0.00494736425702434,-0.0391186199671835,
-0.011047626406524));
#19522=CARTESIAN_POINT('Ctrl Pts',(0.00495427789611805,-0.0391181374782679,
-0.0110412153826375));
#19523=CARTESIAN_POINT('Ctrl Pts',(0.00496741595444978,-0.0391172193693551,
-0.0110292545223772));
#19524=CARTESIAN_POINT('Ctrl Pts',(0.00497362728416082,-0.0391167847188831,
-0.0110236911565518));
#19525=CARTESIAN_POINT('Ctrl Pts',(0.00498897441833383,-0.0391157098047501,
-0.0110101676093));
#19526=CARTESIAN_POINT('Ctrl Pts',(0.00499815938510211,-0.0391150657181805,
-0.0110022642657901));
#19527=CARTESIAN_POINT('Ctrl Pts',(0.00503415283220102,-0.0391125420106734,
-0.0109720236165643));
#19528=CARTESIAN_POINT('Ctrl Pts',(0.00506162160770138,-0.039110616811391,
-0.0109504911723559));
#19529=CARTESIAN_POINT('Ctrl Pts',(0.00514349392865255,-0.039104935298988,
-0.0108906805803855));
#19530=CARTESIAN_POINT('Ctrl Pts',(0.00519967173071391,-0.0391011087929687,
-0.0108549650247));
#19531=CARTESIAN_POINT('Ctrl Pts',(0.00533598222954914,-0.0390922196205954,
-0.0107802011851357));
#19532=CARTESIAN_POINT('Ctrl Pts',(0.00541754982499925,-0.0390871998052542,
-0.010744238977239));
#19533=CARTESIAN_POINT('Ctrl Pts',(0.00552648109427711,-0.0390809947467151,
-0.0107070746997244));
#19534=CARTESIAN_POINT('Ctrl Pts',(0.00555140264478281,-0.0390796061368119,
-0.0106992723668724));
#19535=CARTESIAN_POINT('Ctrl Pts',(0.0055917398879053,-0.0390774073063466,
-0.0106877593765357));
#19536=CARTESIAN_POINT('Ctrl Pts',(0.00560703490154429,-0.0390765846061403,
-0.0106836474495651));
#19537=CARTESIAN_POINT('Ctrl Pts',(0.00563662971341949,-0.0390750133015953,
-0.0106761777567649));
#19538=CARTESIAN_POINT('Ctrl Pts',(0.00565091941109882,-0.0390742637414912,
-0.0106727872795905));
#19539=CARTESIAN_POINT('Ctrl Pts',(0.00568467571391375,-0.0390725135560467,
-0.0106652853934554));
#19540=CARTESIAN_POINT('Ctrl Pts',(0.00570417792533073,-0.0390715183425913,
-0.0106613454094218));
#19541=CARTESIAN_POINT('Ctrl Pts',(0.00577398167263248,-0.0390680078261219,
-0.0106486429732906));
#19542=CARTESIAN_POINT('Ctrl Pts',(0.00582463675819904,-0.0390655565953935,
-0.0106420006414148));
#19543=CARTESIAN_POINT('Ctrl Pts',(0.00596830037744303,-0.0390587712443476,
-0.0106303738679852));
#19544=CARTESIAN_POINT('Ctrl Pts',(0.00606155604019374,-0.0390545708411053,
-0.0106312750022569));
#19545=CARTESIAN_POINT('Ctrl Pts',(0.00620951113169414,-0.0390476532338127,
-0.010646131558299));
#19546=CARTESIAN_POINT('Ctrl Pts',(0.00626451565654233,-0.0390450207102955,
-0.0106546780924168));
#19547=CARTESIAN_POINT('Ctrl Pts',(0.00633261484030529,-0.0390415605365138,
-0.0106690646844277));
#19548=CARTESIAN_POINT('Ctrl Pts',(0.00634625548939901,-0.0390408571363762,
-0.0106721406696479));
#19549=CARTESIAN_POINT('Ctrl Pts',(0.00636829965813915,-0.0390397009499894,
-0.0106774275028167));
#19550=CARTESIAN_POINT('Ctrl Pts',(0.0063767298984555,-0.0390392541495181,
-0.0106795247645937));
#19551=CARTESIAN_POINT('Ctrl Pts',(0.00639368003088043,-0.0390383456153133,
-0.010683893911116));
#19552=CARTESIAN_POINT('Ctrl Pts',(0.00640219901486224,-0.0390378837954673,
-0.0106861678533931));
#19553=CARTESIAN_POINT('Ctrl Pts',(0.00642477154092618,-0.0390366471595487,
-0.0106924007900493));
#19554=CARTESIAN_POINT('Ctrl Pts',(0.00643878889834325,-0.0390358658047163,
-0.0106964863798978));
#19555=CARTESIAN_POINT('Ctrl Pts',(0.00647015743340303,-0.0390340902693345,
-0.0107061142901487));
#19556=CARTESIAN_POINT('Ctrl Pts',(0.0064874726165753,-0.0390330914216456,
-0.0107117661541405));
#19557=CARTESIAN_POINT('Ctrl Pts',(0.00654348641183271,-0.0390298075669738,
-0.0107311534569095));
#19558=CARTESIAN_POINT('Ctrl Pts',(0.00658173657543491,-0.0390274828010913,
-0.0107461269699083));
#19559=CARTESIAN_POINT('Ctrl Pts',(0.00673682752679571,-0.0390178249452355,
-0.010814094167959));
#19560=CARTESIAN_POINT('Ctrl Pts',(0.00684745537657086,-0.0390104331868801,
-0.010880040212544));
#19561=CARTESIAN_POINT('Ctrl Pts',(0.00696833479990033,-0.039002188831304,
-0.0109742711152271));
#19562=CARTESIAN_POINT('Ctrl Pts',(0.00698764556277352,-0.0390008637178099,
-0.0109900926292969));
#19563=CARTESIAN_POINT('Ctrl Pts',(0.00701839517662821,-0.0389987396081037,
-0.0110165587146165));
#19564=CARTESIAN_POINT('Ctrl Pts',(0.00703007067967821,-0.0389979296181438,
-0.0110269202778433));
#19565=CARTESIAN_POINT('Ctrl Pts',(0.00705249455834346,-0.0389963664630501,
-0.0110474372418153));
#19566=CARTESIAN_POINT('Ctrl Pts',(0.00706325811453892,-0.0389956126402495,
-0.0110575734617343));
#19567=CARTESIAN_POINT('Ctrl Pts',(0.00708861841509724,-0.0389938270572344,
-0.0110821529038121));
#19568=CARTESIAN_POINT('Ctrl Pts',(0.00710307594744084,-0.0389928013815913,
-0.0110967360158397));
#19569=CARTESIAN_POINT('Ctrl Pts',(0.00715635362440578,-0.0389889860809594,
-0.0111526663914811));
#19570=CARTESIAN_POINT('Ctrl Pts',(0.00719317687776992,-0.0389862774906632,
-0.011195855932776));
#19571=CARTESIAN_POINT('Ctrl Pts',(0.00730154224009851,-0.0389779022255479,
-0.0113381453884242));
#19572=CARTESIAN_POINT('Ctrl Pts',(0.00736373765625368,-0.0389724850345071,
-0.0114437455928714));
#19573=CARTESIAN_POINT('Ctrl Pts',(0.00742305242963822,-0.0389653653146683,
-0.0115788462389623));
#19574=CARTESIAN_POINT('Ctrl Pts',(0.00743269731929412,-0.0389641173885052,
-0.0116023780062819));
#19575=CARTESIAN_POINT('Ctrl Pts',(0.00744536166511449,-0.0389623313679788,
-0.011635593078288));
#19576=CARTESIAN_POINT('Ctrl Pts',(0.00744887421934554,-0.0389618182098895,
-0.01164508504897));
#19577=CARTESIAN_POINT('Ctrl Pts',(0.00745510551182062,-0.0389608734327401,
-0.0116624467576147));
#19578=CARTESIAN_POINT('Ctrl Pts',(0.00745785444588624,-0.0389604434820309,
-0.0116703053383802));
#19579=CARTESIAN_POINT('Ctrl Pts',(0.00746359357554317,-0.0389595165110634,
-0.0116871483671832));
#19580=CARTESIAN_POINT('Ctrl Pts',(0.00746656483844161,-0.0389590185391279,
-0.011696138560573));
#19581=CARTESIAN_POINT('Ctrl Pts',(0.00747486694332621,-0.0389575749548826,
-0.0117220565677848));
#19582=CARTESIAN_POINT('Ctrl Pts',(0.00747998858189135,-0.0389566187838916,
-0.0117390493152656));
#19583=CARTESIAN_POINT('Ctrl Pts',(0.00750327774456135,-0.0389519488289575,
-0.0118214364027258));
#19584=CARTESIAN_POINT('Ctrl Pts',(0.00751740934664829,-0.038948082386374,
-0.0118878897704586));
#19585=CARTESIAN_POINT('Ctrl Pts',(0.00754354090173187,-0.0389376322812079,
-0.0120686228102988));
#19586=CARTESIAN_POINT('Ctrl Pts',(0.00754724351227303,-0.0389310766950217,
-0.0121836874928687));
#19587=CARTESIAN_POINT('Ctrl Pts',(0.00753619894531687,-0.0389235838767184,
-0.012322644342529));
#19588=CARTESIAN_POINT('Ctrl Pts',(0.00753366191799773,-0.0389222778987208,
-0.0123471309149035));
#19589=CARTESIAN_POINT('Ctrl Pts',(0.00752856910022536,-0.0389201763215992,
-0.0123869622947014));
#19590=CARTESIAN_POINT('Ctrl Pts',(0.00752636533178967,-0.0389193701633615,
-0.0124023470048303));
#19591=CARTESIAN_POINT('Ctrl Pts',(0.00752160667643864,-0.0389178091678657,
-0.0124323328155212));
#19592=CARTESIAN_POINT('Ctrl Pts',(0.00751907309202278,-0.0389170537675525,
-0.0124469355381817));
#19593=CARTESIAN_POINT('Ctrl Pts',(0.00751248791027667,-0.0389152559380051,
-0.012481892394416));
#19594=CARTESIAN_POINT('Ctrl Pts',(0.00750823526394893,-0.0389142198271718,
-0.0125022059381731));
#19595=CARTESIAN_POINT('Ctrl Pts',(0.00749035269647383,-0.0389102896839533,
-0.0125797873426293));
#19596=CARTESIAN_POINT('Ctrl Pts',(0.00747385930766225,-0.0389074836670514,
-0.0126363458925351));
#19597=CARTESIAN_POINT('Ctrl Pts',(0.00743276285457901,-0.038901739260366,
-0.0127521683776472));
#19598=CARTESIAN_POINT('Ctrl Pts',(0.00740761702544376,-0.0388988166066109,
-0.012811119312464));
#19599=CARTESIAN_POINT('Ctrl Pts',(0.007348218068312,-0.0388927159273206,
-0.012929395166544));
#19600=CARTESIAN_POINT('Ctrl Pts',(0.007313534998016,-0.0388895400290671,
-0.0129883443063694));
#19601=CARTESIAN_POINT('Ctrl Pts',(0.00726518862711358,-0.0388853172345711,
-0.0130592864904039));
#19602=CARTESIAN_POINT('Ctrl Pts',(0.00725506765641552,-0.038884442732458,
-0.0130736069380024));
#19603=CARTESIAN_POINT('Ctrl Pts',(0.00723913457509837,-0.0388830752889832,
-0.0130953549743917));
#19604=CARTESIAN_POINT('Ctrl Pts',(0.00723349448880731,-0.0388825929311686,
-0.0131029073230419));
#19605=CARTESIAN_POINT('Ctrl Pts',(0.00722273449711926,-0.0388816749024833,
-0.0131170434384656));
#19606=CARTESIAN_POINT('Ctrl Pts',(0.00721762985832142,-0.0388812401977442,
-0.0131236381087119));
#19607=CARTESIAN_POINT('Ctrl Pts',(0.00720497409479823,-0.0388801649079939,
-0.0131397170734844));
#19608=CARTESIAN_POINT('Ctrl Pts',(0.00719736425044089,-0.0388795204938058,
-0.0131491542692982));
#19609=CARTESIAN_POINT('Ctrl Pts',(0.00716738886979466,-0.0388769936245578,
-0.0131854440355372));
#19610=CARTESIAN_POINT('Ctrl Pts',(0.00714422592846327,-0.0388750654521368,
-0.0132116220683606));
#19611=CARTESIAN_POINT('Ctrl Pts',(0.007074335281738,-0.0388693703992489,
-0.0132854026263385));
#19612=CARTESIAN_POINT('Ctrl Pts',(0.00702538550427146,-0.0388655330027893,
-0.0133307906047031));
#19613=CARTESIAN_POINT('Ctrl Pts',(0.00690482984174703,-0.0388566480701473,
-0.0134288508195308));
#19614=CARTESIAN_POINT('Ctrl Pts',(0.00683129821697608,-0.0388516430724164,
-0.0134787985877224));
#19615=CARTESIAN_POINT('Ctrl Pts',(0.00673109230686452,-0.0388454514894299,
-0.0135349098569407));
#19616=CARTESIAN_POINT('Ctrl Pts',(0.00670798999677249,-0.0388440628462404,
-0.01354708667129));
#19617=CARTESIAN_POINT('Ctrl Pts',(0.00667039596381569,-0.0388418639766302,
-0.0135656982634023));
#19618=CARTESIAN_POINT('Ctrl Pts',(0.00665609544373935,-0.038841041269769,
-0.0135725059280733));
#19619=CARTESIAN_POINT('Ctrl Pts',(0.00662833713298731,-0.0388394699606003,
-0.0135851996264756));
#19620=CARTESIAN_POINT('Ctrl Pts',(0.0066148951886901,-0.038838720402377,
-0.0135911160128652));
#19621=CARTESIAN_POINT('Ctrl Pts',(0.00658305007562943,-0.0388369702336013,
-0.0136045930677316));
#19622=CARTESIAN_POINT('Ctrl Pts',(0.00656458091916511,-0.0388359750346175,
-0.0136119915749597));
#19623=CARTESIAN_POINT('Ctrl Pts',(0.00649822346896417,-0.0388324646538866,
-0.0136370954789874));
#19624=CARTESIAN_POINT('Ctrl Pts',(0.00644960447931477,-0.03883001353738,
-0.0136527797439021));
#19625=CARTESIAN_POINT('Ctrl Pts',(0.00631041788138256,-0.0388232287561061,
-0.0136901684397178));
#19626=CARTESIAN_POINT('Ctrl Pts',(0.0062185441687861,-0.0388190287757899,
-0.0137061303249693));
#19627=CARTESIAN_POINT('Ctrl Pts',(0.00607033792702761,-0.0388121111309378,
-0.0137182531696658));
#19628=CARTESIAN_POINT('Ctrl Pts',(0.00601468239509338,-0.0388094780685831,
-0.0137197860162273));
#19629=CARTESIAN_POINT('Ctrl Pts',(0.00594509199167016,-0.0388060172726381,
-0.0137179394224214));
#19630=CARTESIAN_POINT('Ctrl Pts',(0.00593111949503579,-0.0388053138443167,
-0.0137173785022215));
#19631=CARTESIAN_POINT('Ctrl Pts',(0.00590848221466177,-0.0388041576232975,
-0.0137161613611453));
#19632=CARTESIAN_POINT('Ctrl Pts',(0.0058998116710167,-0.038803710817056,
-0.0137156216986488));
#19633=CARTESIAN_POINT('Ctrl Pts',(0.00588235111475376,-0.0388028022844552,
-0.0137143868357823));
#19634=CARTESIAN_POINT('Ctrl Pts',(0.00587356162318101,-0.0388023404721878,
-0.0137136894520232));
#19635=CARTESIAN_POINT('Ctrl Pts',(0.00585023522484449,-0.0388011038786524,
-0.013711637341939));
#19636=CARTESIAN_POINT('Ctrl Pts',(0.0058357110336972,-0.0388003225593684,
-0.0137101515817557));
#19637=CARTESIAN_POINT('Ctrl Pts',(0.00573970412338155,-0.0387950923078076,
-0.0136989516994517));
#19638=CARTESIAN_POINT('Ctrl Pts',(0.00565909161361419,-0.0387903940043232,
-0.0136829572343369));
#19639=CARTESIAN_POINT('Ctrl Pts',(0.0054801130964723,-0.038779744484197,
-0.0136323463305039));
#19640=CARTESIAN_POINT('Ctrl Pts',(0.00538318823585556,-0.0387738334990884,
-0.0135940221098944));
#19641=CARTESIAN_POINT('Ctrl Pts',(0.00526798340782734,-0.038766845214362,
-0.0135344052300495));
#19642=CARTESIAN_POINT('Ctrl Pts',(0.00524541961612259,-0.0387654768773862,
-0.0135220034351331));
#19643=CARTESIAN_POINT('Ctrl Pts',(0.00520955526020677,-0.038763301891781,
-0.01350110594858));
#19644=CARTESIAN_POINT('Ctrl Pts',(0.00519605686572185,-0.0387624832452657,
-0.0134929610899507));
#19645=CARTESIAN_POINT('Ctrl Pts',(0.00517020526310192,-0.0387609146882033,
-0.0134768168483107));
#19646=CARTESIAN_POINT('Ctrl Pts',(0.00515783706482843,-0.0387601639146379,
-0.0134688448194509));
#19647=CARTESIAN_POINT('Ctrl Pts',(0.00512886033229832,-0.0387584032223533,
-0.0134495754168176));
#19648=CARTESIAN_POINT('Ctrl Pts',(0.0051123544587214,-0.0387573989148847,
-0.013438128147564));
#19649=CARTESIAN_POINT('Ctrl Pts',(0.00505340021225542,-0.0387538015648954,
-0.0133955133621236));
#19650=CARTESIAN_POINT('Ctrl Pts',(0.00501232938196228,-0.0387512771926606,
-0.0133624994987274));
#19651=CARTESIAN_POINT('Ctrl Pts',(0.00489850939520006,-0.0387441091084849,
-0.0132609964800816));
#19652=CARTESIAN_POINT('Ctrl Pts',(0.00483062288114043,-0.0387396223224157,
-0.0131874725798259));
#19653=CARTESIAN_POINT('Ctrl Pts',(0.00474158622180993,-0.0387327198280213,
-0.0130700042031375));
#19654=CARTESIAN_POINT('Ctrl Pts',(0.00471462638576875,-0.0387304503182971,
-0.013030794873091));
#19655=CARTESIAN_POINT('Ctrl Pts',(0.00468234447346436,-0.038727406255314,
-0.0129788587550929));
#19656=CARTESIAN_POINT('Ctrl Pts',(0.00467531994155035,-0.0387267215442087,
-0.0129672170388318));
#19657=CARTESIAN_POINT('Ctrl Pts',(0.00466453016997498,-0.0387256316026228,
-0.0129487889438324));
#19658=CARTESIAN_POINT('Ctrl Pts',(0.00466066057851887,-0.0387252326084171,
-0.0129420641624215));
#19659=CARTESIAN_POINT('Ctrl Pts',(0.00465257933629285,-0.0387243813782083,
-0.0129277718710238));
#19660=CARTESIAN_POINT('Ctrl Pts',(0.00464838039864991,-0.0387239283397429,
-0.0129201975932387));
#19661=CARTESIAN_POINT('Ctrl Pts',(0.00463763121422183,-0.038722741016591,
-0.0129004167381425));
#19662=CARTESIAN_POINT('Ctrl Pts',(0.00463118129430683,-0.0387220010383642,
-0.0128881567536514));
#19663=CARTESIAN_POINT('Ctrl Pts',(0.00459919978925148,-0.0387181945419569,
-0.0128253275540626));
#19664=CARTESIAN_POINT('Ctrl Pts',(0.00457630357197659,-0.0387150074745462,
-0.0127734698490567));
#19665=CARTESIAN_POINT('Ctrl Pts',(0.00451092713517522,-0.0387044596490242,
-0.0126001695449571));
#19666=CARTESIAN_POINT('Ctrl Pts',(0.0044807509164299,-0.0386970296432644,
-0.0124746401513882));
#19667=CARTESIAN_POINT('Ctrl Pts',(0.00446351390023315,-0.0386886291404036,
-0.0123200267575324));
#19668=CARTESIAN_POINT('Ctrl Pts',(0.00446122975971187,-0.0386871937913481,
-0.0122931639468433));
#19669=CARTESIAN_POINT('Ctrl Pts',(0.0044587128045693,-0.03868494004789,
-0.0122502771849483));
#19670=CARTESIAN_POINT('Ctrl Pts',(0.00445802375967009,-0.0386841080366129,
-0.0122342864525433));
#19671=CARTESIAN_POINT('Ctrl Pts',(0.0044571945605513,-0.0386825548500941,
-0.0122041463698509));
#19672=CARTESIAN_POINT('Ctrl Pts',(0.004457,-0.0386818320975096,-0.0121900003094259));
#19673=CARTESIAN_POINT('Ctrl Pts',(0.004457,-0.0386811151660051,-0.0121758532865598));
#19674=CARTESIAN_POINT('Origin',(0.006,-0.0418165664398416,-0.0121758532865581));
#19675=CARTESIAN_POINT('',(0.004457,-0.0396826982119552,-0.0121758532865581));
#19676=CARTESIAN_POINT('',(0.004457,-0.0395660360928446,-0.01217585328639));
#19677=CARTESIAN_POINT('',(0.004457,-0.0418165664398416,-0.0121758532865581));
#19678=CARTESIAN_POINT('Ctrl Pts',(0.004457,-0.0390679979850714,-0.0121758532865546));
#19679=CARTESIAN_POINT('Ctrl Pts',(0.00445699999999997,-0.0390686953839983,
-0.0121894198620967));
#19680=CARTESIAN_POINT('Ctrl Pts',(0.00445717892260015,-0.0390693872025768,
-0.0122029861465897));
#19681=CARTESIAN_POINT('Ctrl Pts',(0.00445805141405487,-0.0390710608261081,
-0.0122360559263837));
#19682=CARTESIAN_POINT('Ctrl Pts',(0.00445893610664614,-0.0390720366435178,
-0.0122555522144478));
#19683=CARTESIAN_POINT('Ctrl Pts',(0.00446344280615422,-0.039075504519834,
-0.0123255249457911));
#19684=CARTESIAN_POINT('Ctrl Pts',(0.00446917744010499,-0.0390779322546964,
-0.0123758344947069));
#19685=CARTESIAN_POINT('Ctrl Pts',(0.0044921969495062,-0.0390846143045803,
-0.0125160790739161));
#19686=CARTESIAN_POINT('Ctrl Pts',(0.00451502314309146,-0.0390887366631945,
-0.01260488387904));
#19687=CARTESIAN_POINT('Ctrl Pts',(0.00456549555276677,-0.0390957327627902,
-0.0127473434511737));
#19688=CARTESIAN_POINT('Ctrl Pts',(0.00458864638692,-0.0390985389073823,
-0.012802338565902));
#19689=CARTESIAN_POINT('Ctrl Pts',(0.00462106947919116,-0.0391021931685658,
-0.0128683808641343));
#19690=CARTESIAN_POINT('Ctrl Pts',(0.00462739029966787,-0.039102894822758,
-0.012880825918588));
#19691=CARTESIAN_POINT('Ctrl Pts',(0.00463784278334832,-0.0391040409642443,
-0.0129007321857558));
#19692=CARTESIAN_POINT('Ctrl Pts',(0.0046418691121806,-0.0391044792670903,
-0.01290824811603));
#19693=CARTESIAN_POINT('Ctrl Pts',(0.00465000883326701,-0.0391053598462119,
-0.0129231445533832));
#19694=CARTESIAN_POINT('Ctrl Pts',(0.00465412096044917,-0.0391058020444971,
-0.012930525394924));
#19695=CARTESIAN_POINT('Ctrl Pts',(0.00466500614659929,-0.0391069649779339,
-0.0129496912342172));
#19696=CARTESIAN_POINT('Ctrl Pts',(0.00467187457148897,-0.039107691334684,
-0.0129614209662401));
#19697=CARTESIAN_POINT('Ctrl Pts',(0.00470766636437324,-0.0391114333005876,
-0.0130207340245329));
#19698=CARTESIAN_POINT('Ctrl Pts',(0.00473899350325883,-0.0391145683035145,
-0.0130668141885997));
#19699=CARTESIAN_POINT('Ctrl Pts',(0.00484628643827727,-0.0391246644465148,
-0.0132076079219752));
#19700=CARTESIAN_POINT('Ctrl Pts',(0.00493097347345358,-0.0391317042723518,
-0.0132951217200965));
#19701=CARTESIAN_POINT('Ctrl Pts',(0.0050502642277241,-0.0391401067469135,
-0.0133923686507829));
#19702=CARTESIAN_POINT('Ctrl Pts',(0.00507612840976471,-0.0391418545591673,
-0.0134121255718104));
#19703=CARTESIAN_POINT('Ctrl Pts',(0.00511640525508696,-0.0391444664314168,
-0.0134409214099597));
#19704=CARTESIAN_POINT('Ctrl Pts',(0.00513037342017816,-0.039145353095776,
-0.0134505637134271));
#19705=CARTESIAN_POINT('Ctrl Pts',(0.00515617717978486,-0.0391469571070247,
-0.0134677545931989));
#19706=CARTESIAN_POINT('Ctrl Pts',(0.00516796199648746,-0.0391476771148746,
-0.0134753757818517));
#19707=CARTESIAN_POINT('Ctrl Pts',(0.00519406191203945,-0.0391492450861839,
-0.013491753865759));
#19708=CARTESIAN_POINT('Ctrl Pts',(0.00520841927653804,-0.0391500904185747,
-0.0135004402116778));
#19709=CARTESIAN_POINT('Ctrl Pts',(0.00525104340789119,-0.0391525521840638,
-0.0135252876261503));
#19710=CARTESIAN_POINT('Ctrl Pts',(0.00527968393099445,-0.0391541454467515,
-0.013540790631052));
#19711=CARTESIAN_POINT('Ctrl Pts',(0.00540259418865835,-0.0391607636270299,
-0.0136023743733456));
#19712=CARTESIAN_POINT('Ctrl Pts',(0.00550094045792831,-0.039165506874211,
-0.0136396827169335));
#19713=CARTESIAN_POINT('Ctrl Pts',(0.00566610370748841,-0.0391733719121199,
-0.0136837394866635));
#19714=CARTESIAN_POINT('Ctrl Pts',(0.0057309138947385,-0.0391764413992063,
-0.0136966421615009));
#19715=CARTESIAN_POINT('Ctrl Pts',(0.00581328573465872,-0.0391805275612473,
-0.0137076100751104));
#19716=CARTESIAN_POINT('Ctrl Pts',(0.00583026212705443,-0.0391813795744156,
-0.0137095840602991));
#19717=CARTESIAN_POINT('Ctrl Pts',(0.00585650219428668,-0.0391827164068374,
-0.0137121942349939));
#19718=CARTESIAN_POINT('Ctrl Pts',(0.00586574512224587,-0.0391831910956868,
-0.0137130295124682));
#19719=CARTESIAN_POINT('Ctrl Pts',(0.00588301870259816,-0.0391840862117972,
-0.0137144335361712));
#19720=CARTESIAN_POINT('Ctrl Pts',(0.00589104711586184,-0.0391845055466841,
-0.0137150228896817));
#19721=CARTESIAN_POINT('Ctrl Pts',(0.00591046549139351,-0.039185527414881,
-0.013716295679848));
#19722=CARTESIAN_POINT('Ctrl Pts',(0.00592185897528475,-0.0391861332496683,
-0.0137169156345494));
#19723=CARTESIAN_POINT('Ctrl Pts',(0.00596386839259034,-0.0391883875097967,
-0.0137187344429197));
#19724=CARTESIAN_POINT('Ctrl Pts',(0.00599450976258318,-0.0391900716738004,
-0.0137191476162022));
#19725=CARTESIAN_POINT('Ctrl Pts',(0.00607834829761232,-0.0391947533433757,
-0.0137177813968699));
#19726=CARTESIAN_POINT('Ctrl Pts',(0.00613147297031129,-0.0391978000109013,
-0.0137141624793291));
#19727=CARTESIAN_POINT('Ctrl Pts',(0.00629514240293824,-0.0392072599555462,
-0.0136944721791082));
#19728=CARTESIAN_POINT('Ctrl Pts',(0.00640422403476766,-0.0392136410940809,
-0.0136691455820318));
#19729=CARTESIAN_POINT('Ctrl Pts',(0.00653315678161299,-0.0392209952714821,
-0.0136240294924092));
#19730=CARTESIAN_POINT('Ctrl Pts',(0.00655648506677964,-0.0392223196634337,
-0.0136152263944231));
#19731=CARTESIAN_POINT('Ctrl Pts',(0.00659377084486842,-0.03922442698959,
-0.013600114249361));
#19732=CARTESIAN_POINT('Ctrl Pts',(0.00660786499297001,-0.0392252213587277,
-0.0135941562439969));
#19733=CARTESIAN_POINT('Ctrl Pts',(0.00663493016591397,-0.039226743095013,
-0.0135822374360965));
#19734=CARTESIAN_POINT('Ctrl Pts',(0.00664791162856453,-0.0392274713011273,
-0.0135763043678148));
#19735=CARTESIAN_POINT('Ctrl Pts',(0.00667836150793591,-0.0392291763118657,
-0.0135618734684553));
#19736=CARTESIAN_POINT('Ctrl Pts',(0.00669575563740352,-0.0392301478151441,
-0.0135532241209742));
#19737=CARTESIAN_POINT('Ctrl Pts',(0.0067572058870162,-0.0392335756898309,
-0.0135212063640623));
#19738=CARTESIAN_POINT('Ctrl Pts',(0.00680028839480739,-0.039235969814639,
-0.0134960330851471));
#19739=CARTESIAN_POINT('Ctrl Pts',(0.00690362017739876,-0.0392417721421321,
-0.0134287353106675));
#19740=CARTESIAN_POINT('Ctrl Pts',(0.00696222276467297,-0.0392451144893761,
-0.0133843111824927));
#19741=CARTESIAN_POINT('Ctrl Pts',(0.0070759684016399,-0.0392520614055408,
-0.0132845471335246));
#19742=CARTESIAN_POINT('Ctrl Pts',(0.00713052367811452,-0.0392556611642383,
-0.0132288603807474));
#19743=CARTESIAN_POINT('Ctrl Pts',(0.00718989359644846,-0.0392602349526987,
-0.0131583037140563));
#19744=CARTESIAN_POINT('Ctrl Pts',(0.00719899377424118,-0.0392609567091442,
-0.013147176875781));
#19745=CARTESIAN_POINT('Ctrl Pts',(0.0072132971267044,-0.0392621276847253,
-0.0131291807738793));
#19746=CARTESIAN_POINT('Ctrl Pts',(0.00721860068672292,-0.039262570225207,
-0.0131223920206809));
#19747=CARTESIAN_POINT('Ctrl Pts',(0.00722894616682311,-0.0392634508920071,
-0.0131089183559192));
#19748=CARTESIAN_POINT('Ctrl Pts',(0.00723399103190644,-0.0392638888043464,
-0.0131022361603833));
#19749=CARTESIAN_POINT('Ctrl Pts',(0.00724686308213792,-0.039265027487708,
-0.0130848947251949));
#19750=CARTESIAN_POINT('Ctrl Pts',(0.00725460796428767,-0.0392657334772657,
-0.0130741754536445));
#19751=CARTESIAN_POINT('Ctrl Pts',(0.00729071708465322,-0.0392691206022097,
-0.0130228208919799));
#19752=CARTESIAN_POINT('Ctrl Pts',(0.00731724885600675,-0.0392718964700562,
-0.0129809367734704));
#19753=CARTESIAN_POINT('Ctrl Pts',(0.00738083568070027,-0.0392792146620341,
-0.0128689739860248));
#19754=CARTESIAN_POINT('Ctrl Pts',(0.00741459209835948,-0.0392838036149811,
-0.012797185069273));
#19755=CARTESIAN_POINT('Ctrl Pts',(0.00746725863704162,-0.0392922220190079,
-0.0126583471720437));
#19756=CARTESIAN_POINT('Ctrl Pts',(0.00748744147699956,-0.039296066079905,
-0.0125919877843493));
#19757=CARTESIAN_POINT('Ctrl Pts',(0.00750800701896821,-0.0393009325778648,
-0.0125033223703571));
#19758=CARTESIAN_POINT('Ctrl Pts',(0.00751246920050807,-0.0393020806166226,
-0.0124820528157463));
#19759=CARTESIAN_POINT('Ctrl Pts',(0.00751891884626964,-0.0393039036996923,
-0.0124477153174316));
#19760=CARTESIAN_POINT('Ctrl Pts',(0.00752119019596254,-0.0393045875751073,
-0.0124347042619441));
#19761=CARTESIAN_POINT('Ctrl Pts',(0.00752559311442695,-0.0393060076883288,
-0.0124074194340762));
#19762=CARTESIAN_POINT('Ctrl Pts',(0.00752769205533074,-0.0393067428392544,
-0.012393141652205));
#19763=CARTESIAN_POINT('Ctrl Pts',(0.00753227361886957,-0.0393085022334846,
-0.0123586169939624));
#19764=CARTESIAN_POINT('Ctrl Pts',(0.00753455569284665,-0.0393095201540773,
-0.0123383460251102));
#19765=CARTESIAN_POINT('Ctrl Pts',(0.00754183775557845,-0.039313419275789,
-0.0122596551296015));
#19766=CARTESIAN_POINT('Ctrl Pts',(0.00754390877309404,-0.0393162112225813,
-0.0122010116419741));
#19767=CARTESIAN_POINT('Ctrl Pts',(0.00754005020850498,-0.0393245126117885,
-0.0120231399901397));
#19768=CARTESIAN_POINT('Ctrl Pts',(0.00752364561879022,-0.0393297938282777,
-0.0119046046787139));
#19769=CARTESIAN_POINT('Ctrl Pts',(0.00748685726419432,-0.0393368438622562,
-0.0117624981352158));
#19770=CARTESIAN_POINT('Ctrl Pts',(0.00747924553250601,-0.0393381902075373,
-0.0117360357114069));
#19771=CARTESIAN_POINT('Ctrl Pts',(0.00746753392973297,-0.0393401360248672,
-0.011699072819514));
#19772=CARTESIAN_POINT('Ctrl Pts',(0.0074640204258473,-0.0393407061469304,
-0.0116883908498046));
#19773=CARTESIAN_POINT('Ctrl Pts',(0.00745779889211259,-0.0393416946057261,
-0.0116701499691105));
#19774=CARTESIAN_POINT('Ctrl Pts',(0.00745514809726178,-0.0393421097224252,
-0.0116625722051338));
#19775=CARTESIAN_POINT('Ctrl Pts',(0.0074492751930599,-0.039343017061454,
-0.0116461946996333));
#19776=CARTESIAN_POINT('Ctrl Pts',(0.00744603202849368,-0.0393435104001268,
-0.0116374035045648));
#19777=CARTESIAN_POINT('Ctrl Pts',(0.00743630988549436,-0.0393449661224141,
-0.0116117712851429));
#19778=CARTESIAN_POINT('Ctrl Pts',(0.00742961549899903,-0.0393459398116313,
-0.0115950141844532));
#19779=CARTESIAN_POINT('Ctrl Pts',(0.00741320349817015,-0.0393482560793902,
-0.011555936030971));
#19780=CARTESIAN_POINT('Ctrl Pts',(0.00740324851413722,-0.0393496084347588,
-0.011533720091317));
#19781=CARTESIAN_POINT('Ctrl Pts',(0.00736298331225454,-0.0393548626703705,
-0.0114492749982722));
#19782=CARTESIAN_POINT('Ctrl Pts',(0.00732902487033237,-0.0393588589112449,
-0.0113888767813469));
#19783=CARTESIAN_POINT('Ctrl Pts',(0.0072432381655167,-0.0393678336274405,
-0.0112577808526611));
#19784=CARTESIAN_POINT('Ctrl Pts',(0.00718920850443293,-0.0393727712201326,
-0.0111887947561811));
#19785=CARTESIAN_POINT('Ctrl Pts',(0.00711195822786157,-0.0393788885134016,
-0.0111057738669521));
#19786=CARTESIAN_POINT('Ctrl Pts',(0.00709382236338263,-0.0393802678734445,
-0.0110872423321149));
#19787=CARTESIAN_POINT('Ctrl Pts',(0.00706411065729706,-0.0393824399331051,
-0.011058374987786));
#19788=CARTESIAN_POINT('Ctrl Pts',(0.0070528315603696,-0.0393832453731153,
-0.0110477420473776));
#19789=CARTESIAN_POINT('Ctrl Pts',(0.00703091463089175,-0.0393847749519049,
-0.0110276957592165));
#19790=CARTESIAN_POINT('Ctrl Pts',(0.00702030333587553,-0.039385500174762,
-0.0110182558590788));
#19791=CARTESIAN_POINT('Ctrl Pts',(0.00699524389711843,-0.039387178344524,
-0.0109965750764129));
#19792=CARTESIAN_POINT('Ctrl Pts',(0.00698069761950371,-0.0393881264915898,
-0.0109844508649484));
#19793=CARTESIAN_POINT('Ctrl Pts',(0.0069299835487691,-0.0393913482912109,
-0.0109437394045853));
#19794=CARTESIAN_POINT('Ctrl Pts',(0.00689275896597333,-0.0393935697898956,
-0.0109165058748375));
#19795=CARTESIAN_POINT('Ctrl Pts',(0.0067908828791787,-0.0393993506137635,
-0.0108487640836643));
#19796=CARTESIAN_POINT('Ctrl Pts',(0.00672435413730686,-0.0394028230549071,
-0.0108113119608518));
#19797=CARTESIAN_POINT('Ctrl Pts',(0.00658758886596875,-0.0394097558447258,
-0.0107471521294095));
#19798=CARTESIAN_POINT('Ctrl Pts',(0.00651763195780711,-0.039413208057472,
-0.0107203454985814));
#19799=CARTESIAN_POINT('Ctrl Pts',(0.00642960987282296,-0.0394177287425997,
-0.0106937675988903));
#19800=CARTESIAN_POINT('Ctrl Pts',(0.00641312501222299,-0.0394185829302909,
-0.0106890882385291));
#19801=CARTESIAN_POINT('Ctrl Pts',(0.0063875881418275,-0.0394199224660671,
-0.0106822968797147));
#19802=CARTESIAN_POINT('Ctrl Pts',(0.00637858883336489,-0.0394203976194904,
-0.0106799903934575));
#19803=CARTESIAN_POINT('Ctrl Pts',(0.00636175584962722,-0.0394212930605527,
-0.0106758377954993));
#19804=CARTESIAN_POINT('Ctrl Pts',(0.00635392773562898,-0.0394217122443688,
-0.0106739714949896));
#19805=CARTESIAN_POINT('Ctrl Pts',(0.00633498375343425,-0.0394227329725285,
-0.0106696113858608));
#19806=CARTESIAN_POINT('Ctrl Pts',(0.00632385433012678,-0.0394233377993604,
-0.0106671793203644));
#19807=CARTESIAN_POINT('Ctrl Pts',(0.00628283310367387,-0.0394255834116466,
-0.0106586899368512));
#19808=CARTESIAN_POINT('Ctrl Pts',(0.00625279189752091,-0.0394272595974423,
-0.0106533963156152));
#19809=CARTESIAN_POINT('Ctrl Pts',(0.00617035672210289,-0.0394319101036196,
-0.0106413772775292));
#19810=CARTESIAN_POINT('Ctrl Pts',(0.00611774320291216,-0.0394349329062986,
-0.0106364462131634));
#19811=CARTESIAN_POINT('Ctrl Pts',(0.00595269210824942,-0.0394444123670926,
-0.0106294889760128));
#19812=CARTESIAN_POINT('Ctrl Pts',(0.00584020401004156,-0.0394508385022363,
-0.0106370379744194));
#19813=CARTESIAN_POINT('Ctrl Pts',(0.00570506492205468,-0.0394582272720285,
-0.0106610993360945));
#19814=CARTESIAN_POINT('Ctrl Pts',(0.00568071335427352,-0.0394595469531732,
-0.0106660445689519));
#19815=CARTESIAN_POINT('Ctrl Pts',(0.00564159093022336,-0.0394616487267255,
-0.0106749783674692));
#19816=CARTESIAN_POINT('Ctrl Pts',(0.00562674206081955,-0.0394624421446139,
-0.0106786020994859));
#19817=CARTESIAN_POINT('Ctrl Pts',(0.0055981290235456,-0.0394639632510294,
-0.0106860369861944));
#19818=CARTESIAN_POINT('Ctrl Pts',(0.00558435916065565,-0.0394646917567988,
-0.0106898197738135));
#19819=CARTESIAN_POINT('Ctrl Pts',(0.00555194286451575,-0.0394663993032991,
-0.0106992108562706));
#19820=CARTESIAN_POINT('Ctrl Pts',(0.00553334597538514,-0.0394673729953005,
-0.0107049820727591));
#19821=CARTESIAN_POINT('Ctrl Pts',(0.00546717229893642,-0.03947082108304,
-0.0107268993478225));
#19822=CARTESIAN_POINT('Ctrl Pts',(0.00542027963022814,-0.0394732321872962,
-0.0107450151629393));
#19823=CARTESIAN_POINT('Ctrl Pts',(0.00529196275906799,-0.0394798346253841,
-0.0108019334403542));
#19824=CARTESIAN_POINT('Ctrl Pts',(0.00521293622902167,-0.0394838984970044,
-0.0108456265870401));
#19825=CARTESIAN_POINT('Ctrl Pts',(0.00508727004304241,-0.039490903777605,
-0.0109302452805476));
#19826=CARTESIAN_POINT('Ctrl Pts',(0.00503845935594229,-0.0394937870607772,
-0.010967526514593));
#19827=CARTESIAN_POINT('Ctrl Pts',(0.00498139135085344,-0.0394975301438743,
-0.0110167666444608));
#19828=CARTESIAN_POINT('Ctrl Pts',(0.00497090573769416,-0.0394982345580348,
-0.0110260661769412));
#19829=CARTESIAN_POINT('Ctrl Pts',(0.00495423816799124,-0.0394993841075498,
-0.011041259042327));
#19830=CARTESIAN_POINT('Ctrl Pts',(0.00494797573156072,-0.0394998229914564,
-0.0110470632971329));
#19831=CARTESIAN_POINT('Ctrl Pts',(0.00493562113641095,-0.0395007035436268,
-0.0110587061012606));
#19832=CARTESIAN_POINT('Ctrl Pts',(0.00492952807540038,-0.0395011451148093,
-0.0110645432263977));
#19833=CARTESIAN_POINT('Ctrl Pts',(0.00491378371668259,-0.0395023045275902,
-0.0110798758708019));
#19834=CARTESIAN_POINT('Ctrl Pts',(0.00490420913692148,-0.0395030279319976,
-0.0110894488176715));
#19835=CARTESIAN_POINT('Ctrl Pts',(0.00485659331262227,-0.0395067131943612,
-0.0111383263759616));
#19836=CARTESIAN_POINT('Ctrl Pts',(0.00482053772912876,-0.0395097903013872,
-0.0111795055768089));
#19837=CARTESIAN_POINT('Ctrl Pts',(0.00472857369128798,-0.0395182754451432,
-0.0112965414781219));
#19838=CARTESIAN_POINT('Ctrl Pts',(0.00467729406004648,-0.0395237340592735,
-0.0113757501141798));
#19839=CARTESIAN_POINT('Ctrl Pts',(0.00460934819643015,-0.0395319167039995,
-0.0115052919742768));
#19840=CARTESIAN_POINT('Ctrl Pts',(0.00458749349020553,-0.039534771741006,
-0.0115526429810435));
#19841=CARTESIAN_POINT('Ctrl Pts',(0.00456056200635623,-0.0395386220185198,
-0.0116197291926716));
#19842=CARTESIAN_POINT('Ctrl Pts',(0.00455341594966046,-0.0395396842253357,
-0.0116385913560591));
#19843=CARTESIAN_POINT('Ctrl Pts',(0.00454185561065168,-0.039541476070495,
-0.0116710097793207));
#19844=CARTESIAN_POINT('Ctrl Pts',(0.00453725575577049,-0.0395422117273783,
-0.0116844966737503));
#19845=CARTESIAN_POINT('Ctrl Pts',(0.00452819314722318,-0.0395437101806055,
-0.0117123243313634));
#19846=CARTESIAN_POINT('Ctrl Pts',(0.00452375161652047,-0.0395444722214163,
-0.0117266704341375));
#19847=CARTESIAN_POINT('Ctrl Pts',(0.00451289661452796,-0.0395464101513956,
-0.011763633585646));
#19848=CARTESIAN_POINT('Ctrl Pts',(0.00450678917596303,-0.0395475761713947,
-0.0117863368317175));
#19849=CARTESIAN_POINT('Ctrl Pts',(0.00448586224387566,-0.0395518884847612,
-0.0118718748533699));
#19850=CARTESIAN_POINT('Ctrl Pts',(0.00447447100211849,-0.0395549300823339,
-0.0119354821694805));
#19851=CARTESIAN_POINT('Ctrl Pts',(0.00446063355208643,-0.0395605389620168,
-0.0120558421289123));
#19852=CARTESIAN_POINT('Ctrl Pts',(0.00445726780193232,-0.0395631150864761,
-0.0121123779022069));
#19853=CARTESIAN_POINT('Ctrl Pts',(0.00445700511695951,-0.0395658248041787,
-0.0121712646770232));
#19854=CARTESIAN_POINT('Ctrl Pts',(0.0044570000000005,-0.0395659304248953,
-0.012173559022778));
#19855=CARTESIAN_POINT('Ctrl Pts',(0.004457,-0.0395660360928446,-0.012175853286222));
#19856=CARTESIAN_POINT('Ctrl Pts',(0.004457,-0.0396826982119552,-0.0121758532865581));
#19857=CARTESIAN_POINT('Ctrl Pts',(0.004457,-0.0396813477299627,-0.0121464846796299));
#19858=CARTESIAN_POINT('Ctrl Pts',(0.00445783847339417,-0.0396799949258229,
-0.0121171007278321));
#19859=CARTESIAN_POINT('Ctrl Pts',(0.0044628146601358,-0.0396759462670294,
-0.0120301049610795));
#19860=CARTESIAN_POINT('Ctrl Pts',(0.0044693426023891,-0.0396732191572142,
-0.0119727075344027));
#19861=CARTESIAN_POINT('Ctrl Pts',(0.00448141319135842,-0.0396696575578575,
-0.0119021079550972));
#19862=CARTESIAN_POINT('Ctrl Pts',(0.00448394202212993,-0.03966895783635,
-0.0118884327154763));
#19863=CARTESIAN_POINT('Ctrl Pts',(0.0044883471833378,-0.0396678061649656,
-0.0118662891469104));
#19864=CARTESIAN_POINT('Ctrl Pts',(0.00449011073731352,-0.039667360112438,
-0.0118577988825109));
#19865=CARTESIAN_POINT('Ctrl Pts',(0.00449358570177043,-0.0396665077070338,
-0.0118417499813716));
#19866=CARTESIAN_POINT('Ctrl Pts',(0.00449528267524121,-0.0396661022051225,
-0.0118341885034603));
#19867=CARTESIAN_POINT('Ctrl Pts',(0.00450010243933532,-0.0396649796913041,
-0.0118134449184029));
#19868=CARTESIAN_POINT('Ctrl Pts',(0.00450334192183023,-0.0396642566401885,
-0.0118002909204535));
#19869=CARTESIAN_POINT('Ctrl Pts',(0.00451856796563602,-0.0396609960613739,
-0.0117417936437361));
#19870=CARTESIAN_POINT('Ctrl Pts',(0.00453244432857552,-0.0396583767538485,
-0.0116969708733201));
#19871=CARTESIAN_POINT('Ctrl Pts',(0.00458237804669033,-0.0396500308634471,
-0.0115583727629975));
#19872=CARTESIAN_POINT('Ctrl Pts',(0.00462556288009749,-0.0396442067768584,
-0.0114674332420484));
#19873=CARTESIAN_POINT('Ctrl Pts',(0.00470446074305107,-0.039635648261241,
-0.0113360832850121));
#19874=CARTESIAN_POINT('Ctrl Pts',(0.00473394847505017,-0.0396327601067996,
-0.0112922527054986));
#19875=CARTESIAN_POINT('Ctrl Pts',(0.00477768781464053,-0.0396288824594807,
-0.01123393719722));
#19876=CARTESIAN_POINT('Ctrl Pts',(0.00479006148908284,-0.0396278249657828,
-0.0112180945238591));
#19877=CARTESIAN_POINT('Ctrl Pts',(0.00481202474720552,-0.0396260138521039,
-0.0111910790176491));
#19878=CARTESIAN_POINT('Ctrl Pts',(0.00482147100184777,-0.0396252548043261,
-0.011179793558469));
#19879=CARTESIAN_POINT('Ctrl Pts',(0.00484136391135476,-0.0396236961559212,
-0.0111567067120257));
#19880=CARTESIAN_POINT('Ctrl Pts',(0.00485183284751335,-0.0396228975837342,
-0.0111449267424395));
#19881=CARTESIAN_POINT('Ctrl Pts',(0.00487985460071512,-0.0396208146781954,
-0.0111143522291492));
#19882=CARTESIAN_POINT('Ctrl Pts',(0.00489770024196365,-0.0396195425516972,
-0.0110958322007141));
#19883=CARTESIAN_POINT('Ctrl Pts',(0.00499026602745119,-0.0396131942898049,
-0.011004454012922));
#19884=CARTESIAN_POINT('Ctrl Pts',(0.00507177605414737,-0.0396084218615467,
-0.0109388646206537));
#19885=CARTESIAN_POINT('Ctrl Pts',(0.00522781437372861,-0.03959986063786,
-0.0108374748169949));
#19886=CARTESIAN_POINT('Ctrl Pts',(0.00529976403573722,-0.0395960881101994,
-0.0107984664089359));
#19887=CARTESIAN_POINT('Ctrl Pts',(0.00538780060713031,-0.0395913100917849,
-0.0107594232560758));
#19888=CARTESIAN_POINT('Ctrl Pts',(0.00540122886535887,-0.0395905769266395,
-0.0107536946358699));
#19889=CARTESIAN_POINT('Ctrl Pts',(0.00542289402125798,-0.0395893840455478,
-0.0107448133052319));
#19890=CARTESIAN_POINT('Ctrl Pts',(0.00543108044167049,-0.0395889310424141,
-0.010741539071419));
#19891=CARTESIAN_POINT('Ctrl Pts',(0.00544738792697787,-0.0395880233536636,
-0.0107351783162355));
#19892=CARTESIAN_POINT('Ctrl Pts',(0.0054555078627059,-0.039587568791161,
-0.0107320898789015));
#19893=CARTESIAN_POINT('Ctrl Pts',(0.00547676543253324,-0.0395863728255643,
-0.0107242093404772));
#19894=CARTESIAN_POINT('Ctrl Pts',(0.00548994269434414,-0.0395856255829875,
-0.0107195270602234));
#19895=CARTESIAN_POINT('Ctrl Pts',(0.00555587875445098,-0.0395818637929086,
-0.0106971026181067));
#19896=CARTESIAN_POINT('Ctrl Pts',(0.00560950361920212,-0.0395787336211777,
-0.0106820464514176));
#19897=CARTESIAN_POINT('Ctrl Pts',(0.00575462281729089,-0.0395702686795682,
-0.010649650447936));
#19898=CARTESIAN_POINT('Ctrl Pts',(0.00584708012371164,-0.0395648933650903,
-0.0106376327076299));
#19899=CARTESIAN_POINT('Ctrl Pts',(0.00599106730777496,-0.0395568581375937,
-0.0106320349547745));
#19900=CARTESIAN_POINT('Ctrl Pts',(0.00604214631384966,-0.039554069253411,
-0.0106325842638334));
#19901=CARTESIAN_POINT('Ctrl Pts',(0.00611296474157648,-0.0395502973398212,
-0.0106368654059014));
#19902=CARTESIAN_POINT('Ctrl Pts',(0.00613279694005223,-0.0395492512057836,
-0.0106384497121049));
#19903=CARTESIAN_POINT('Ctrl Pts',(0.00616720681918736,-0.0395474530826791,
-0.0106418694094461));
#19904=CARTESIAN_POINT('Ctrl Pts',(0.00618179888186008,-0.0395466958805926,
-0.0106435302652938));
#19905=CARTESIAN_POINT('Ctrl Pts',(0.00621207369310954,-0.0395451352821237,
-0.010647414683645));
#19906=CARTESIAN_POINT('Ctrl Pts',(0.00622775042261874,-0.0395443330149265,
-0.0106496719137741));
#19907=CARTESIAN_POINT('Ctrl Pts',(0.00626917403819766,-0.0395422270801734,
-0.0106562888367076));
#19908=CARTESIAN_POINT('Ctrl Pts',(0.00629485018986162,-0.0395409361443949,
-0.0106610614719308));
#19909=CARTESIAN_POINT('Ctrl Pts',(0.00640527168510984,-0.0395354312145129,
-0.0106845006360704));
#19910=CARTESIAN_POINT('Ctrl Pts',(0.00648848281896762,-0.0395314138452922,
-0.0107096459613776));
#19911=CARTESIAN_POINT('Ctrl Pts',(0.0066324695229468,-0.039524288718721,
-0.0107667850576158));
#19912=CARTESIAN_POINT('Ctrl Pts',(0.00669406056589768,-0.0395211751249589,
-0.0107960815303267));
#19913=CARTESIAN_POINT('Ctrl Pts',(0.00678435861486421,-0.0395162567234915,
-0.0108466128520862));
#19914=CARTESIAN_POINT('Ctrl Pts',(0.00681460207201887,-0.0395145437879072,
-0.0108649292893225));
#19915=CARTESIAN_POINT('Ctrl Pts',(0.00685437394505175,-0.0395121660453758,
-0.0108909244011376));
#19916=CARTESIAN_POINT('Ctrl Pts',(0.00686448053538532,-0.0395115505375329,
-0.0108977020962806));
#19917=CARTESIAN_POINT('Ctrl Pts',(0.00688138227626394,-0.0395105001679217,
-0.0109093289285492));
#19918=CARTESIAN_POINT('Ctrl Pts',(0.00688822032611236,-0.0395100692725072,
-0.0109141150738139));
#19919=CARTESIAN_POINT('Ctrl Pts',(0.00690268068269267,-0.0395091447748852,
-0.0109244120990847));
#19920=CARTESIAN_POINT('Ctrl Pts',(0.00691029186237285,-0.0395086502977725,
-0.0109299374879752));
#19921=CARTESIAN_POINT('Ctrl Pts',(0.00693186511827695,-0.0395072272758132,
-0.0109459019424193));
#19922=CARTESIAN_POINT('Ctrl Pts',(0.00694570108428603,-0.039506288607471,
-0.0109565082498288));
#19923=CARTESIAN_POINT('Ctrl Pts',(0.00701132081403296,-0.0395017219760775,
-0.0110085994139154));
#19924=CARTESIAN_POINT('Ctrl Pts',(0.00706056951866714,-0.0394979467687672,
-0.0110531589714796));
#19925=CARTESIAN_POINT('Ctrl Pts',(0.00715025608634116,-0.0394905828958167,
-0.0111454888787071));
#19926=CARTESIAN_POINT('Ctrl Pts',(0.00719096653660539,-0.0394870033330039,
-0.0111928278015998));
#19927=CARTESIAN_POINT('Ctrl Pts',(0.00726618388378849,-0.0394800037621922,
-0.0112918469070288));
#19928=CARTESIAN_POINT('Ctrl Pts',(0.00730066353650197,-0.0394765892690963,
-0.0113434083495262));
#19929=CARTESIAN_POINT('Ctrl Pts',(0.00734257510813545,-0.0394721622303368,
-0.0114150747698283));
#19930=CARTESIAN_POINT('Ctrl Pts',(0.00735282647491831,-0.0394710528057832,
-0.0114334568571033));
#19931=CARTESIAN_POINT('Ctrl Pts',(0.00736967399406156,-0.0394691817601985,
-0.0114651752693526));
#19932=CARTESIAN_POINT('Ctrl Pts',(0.00737645900917835,-0.0394684137109337,
-0.0114784074389878));
#19933=CARTESIAN_POINT('Ctrl Pts',(0.00738990428348948,-0.039466860629517,
-0.011505589195671));
#19934=CARTESIAN_POINT('Ctrl Pts',(0.00739654833087479,-0.0394660762105413,
-0.0115195449365994));
#19935=CARTESIAN_POINT('Ctrl Pts',(0.00741304658386693,-0.0394640821783535,
-0.011555584756424));
#19936=CARTESIAN_POINT('Ctrl Pts',(0.00742259351896264,-0.0394628828222944,
-0.0115778052492526));
#19937=CARTESIAN_POINT('Ctrl Pts',(0.00747562986144973,-0.0394559216441528,
-0.0117097129568753));
#19938=CARTESIAN_POINT('Ctrl Pts',(0.00750694344444106,-0.0394505712751792,
-0.0118238685044784));
#19939=CARTESIAN_POINT('Ctrl Pts',(0.00753237966638465,-0.0394428789488251,
-0.0119886672284317));
#19940=CARTESIAN_POINT('Ctrl Pts',(0.00753752853051408,-0.039440612730165,
-0.0120371750878508));
#19941=CARTESIAN_POINT('Ctrl Pts',(0.00754207195897334,-0.0394368747944667,
-0.012114927858575));
#19942=CARTESIAN_POINT('Ctrl Pts',(0.00754294731747926,-0.0394354508996611,
-0.0121440536802233));
#19943=CARTESIAN_POINT('Ctrl Pts',(0.00754301545459039,-0.0394334725882418,
-0.0121834575229681));
#19944=CARTESIAN_POINT('Ctrl Pts',(0.00754293063581711,-0.0394329520788969,
-0.012193729779417));
#19945=CARTESIAN_POINT('Ctrl Pts',(0.00754259079738741,-0.0394319983784609,
-0.0122123564785995));
#19946=CARTESIAN_POINT('Ctrl Pts',(0.0075423704519968,-0.0394315669838307,
-0.0122207112725747));
#19947=CARTESIAN_POINT('Ctrl Pts',(0.00754175894997875,-0.0394306436476368,
-0.0122384330323876));
#19948=CARTESIAN_POINT('Ctrl Pts',(0.0075413502928078,-0.0394301508688712,
-0.012247798756299));
#19949=CARTESIAN_POINT('Ctrl Pts',(0.00753994571567989,-0.0394287377858593,
-0.0122744171383556));
#19950=CARTESIAN_POINT('Ctrl Pts',(0.00753874528646912,-0.0394278075655499,
-0.0122916571571346));
#19951=CARTESIAN_POINT('Ctrl Pts',(0.00753177511392533,-0.0394234021706708,
-0.0123722088515272));
#19952=CARTESIAN_POINT('Ctrl Pts',(0.00752238592811473,-0.0394197916372626,
-0.012435141760605));
#19953=CARTESIAN_POINT('Ctrl Pts',(0.00748376115408445,-0.0394091909128788,
-0.0126164727734878));
#19954=CARTESIAN_POINT('Ctrl Pts',(0.00744435035573978,-0.0394022112486446,
-0.0127322282952963));
#19955=CARTESIAN_POINT('Ctrl Pts',(0.0073815215085189,-0.039394406462627,
-0.012863461934239));
#19956=CARTESIAN_POINT('Ctrl Pts',(0.00737082950555611,-0.0393931547705145,
-0.0128845378977993));
#19957=CARTESIAN_POINT('Ctrl Pts',(0.00735240109533733,-0.0393911171079385,
-0.0129188847988983));
#19958=CARTESIAN_POINT('Ctrl Pts',(0.00734494340957853,-0.0393903217788686,
-0.012932300110989));
#19959=CARTESIAN_POINT('Ctrl Pts',(0.00732983328516685,-0.0393887659401232,
-0.0129585509646158));
#19960=CARTESIAN_POINT('Ctrl Pts',(0.00732219210545131,-0.0393880051504652,
-0.0129713910152601));
#19961=CARTESIAN_POINT('Ctrl Pts',(0.00730312691546296,-0.0393861676315112,
-0.0130023939971382));
#19962=CARTESIAN_POINT('Ctrl Pts',(0.00729150810773439,-0.0393850979851545,
-0.0130204337546251));
#19963=CARTESIAN_POINT('Ctrl Pts',(0.00724215521505821,-0.0393807467790544,
-0.0130936594565076));
#19964=CARTESIAN_POINT('Ctrl Pts',(0.00720122910888186,-0.0393775819218252,
-0.0131466094160062));
#19965=CARTESIAN_POINT('Ctrl Pts',(0.0071189177617141,-0.0393718009711476,
-0.0132398947139605));
#19966=CARTESIAN_POINT('Ctrl Pts',(0.00707845579281076,-0.0393691732790731,
-0.0132808846220152));
#19967=CARTESIAN_POINT('Ctrl Pts',(0.00698731281257816,-0.0393634992861697,
-0.013363431365392));
#19968=CARTESIAN_POINT('Ctrl Pts',(0.00693608663055851,-0.0393604504404471,
-0.0134042134842198));
#19969=CARTESIAN_POINT('Ctrl Pts',(0.00686816131919823,-0.0393563759987104,
-0.0134515678176983));
#19970=CARTESIAN_POINT('Ctrl Pts',(0.00685372372266027,-0.0393555081534511,
-0.013461274385076));
#19971=CARTESIAN_POINT('Ctrl Pts',(0.00683123889132765,-0.039354148919096,
-0.013475845297313));
#19972=CARTESIAN_POINT('Ctrl Pts',(0.00682330577582393,-0.0393536679148107,
-0.0134808839043566));
#19973=CARTESIAN_POINT('Ctrl Pts',(0.00680823861899004,-0.0393527507020857,
-0.0134902615373085));
#19974=CARTESIAN_POINT('Ctrl Pts',(0.00680111461139358,-0.0393523154246154,
-0.0134946156164375));
#19975=CARTESIAN_POINT('Ctrl Pts',(0.00678350750990883,-0.0393512361991847,
-0.0135051814857837));
#19976=CARTESIAN_POINT('Ctrl Pts',(0.00677298560503136,-0.0393505883564157,
-0.013511327253304));
#19977=CARTESIAN_POINT('Ctrl Pts',(0.00673153221613039,-0.0393480280940242,
-0.0135348858674737));
#19978=CARTESIAN_POINT('Ctrl Pts',(0.00670007796683072,-0.0393460684753522,
-0.0135513529986706));
#19979=CARTESIAN_POINT('Ctrl Pts',(0.00660619306212918,-0.0393402284134957,
-0.0135964494906086));
#19980=CARTESIAN_POINT('Ctrl Pts',(0.00654238602229767,-0.0393362739721421,
-0.0136220139417997));
#19981=CARTESIAN_POINT('Ctrl Pts',(0.0063952543354997,-0.0393274334059212,
-0.0136698506289411));
#19982=CARTESIAN_POINT('Ctrl Pts',(0.00631132821339653,-0.0393225857900594,
-0.0136895678719792));
#19983=CARTESIAN_POINT('Ctrl Pts',(0.00620036099988987,-0.0393165380231932,
-0.013706012145665));
#19984=CARTESIAN_POINT('Ctrl Pts',(0.00617444042482592,-0.0393151494417041,
-0.0137091834241441));
#19985=CARTESIAN_POINT('Ctrl Pts',(0.00613268754209303,-0.0393129506447138,
-0.0137132191561805));
#19986=CARTESIAN_POINT('Ctrl Pts',(0.00611690142752418,-0.0393121279502458,
-0.0137145000561371));
#19987=CARTESIAN_POINT('Ctrl Pts',(0.00608644415222851,-0.0393105566497989,
-0.0137164999265871));
#19988=CARTESIAN_POINT('Ctrl Pts',(0.00607177701558757,-0.0393098070881823,
-0.0137172528907943));
#19989=CARTESIAN_POINT('Ctrl Pts',(0.0060372205574106,-0.0393080568887944,
-0.0137185325809435));
#19990=CARTESIAN_POINT('Ctrl Pts',(0.00601732718663373,-0.0393070616631757,
-0.0137188842611421));
#19991=CARTESIAN_POINT('Ctrl Pts',(0.00594637482767709,-0.039303551032031,
-0.0137187661752197));
#19992=CARTESIAN_POINT('Ctrl Pts',(0.00589535115549701,-0.0393010997047533,
-0.0137161471023089));
#19993=CARTESIAN_POINT('Ctrl Pts',(0.00575194066052965,-0.0392943138716219,
-0.013701625102289));
#19994=CARTESIAN_POINT('Ctrl Pts',(0.00566037434013233,-0.0392901131104682,
-0.0136838875047544));
#19995=CARTESIAN_POINT('Ctrl Pts',(0.00551754075649261,-0.039283195535279,
-0.013642541876957));
#19996=CARTESIAN_POINT('Ctrl Pts',(0.00546499537765861,-0.0392805634681504,
-0.0136242011111475));
#19997=CARTESIAN_POINT('Ctrl Pts',(0.00540062601821025,-0.0392771038213513,
-0.0135977517849151));
#19998=CARTESIAN_POINT('Ctrl Pts',(0.00538776603958515,-0.0392764004451236,
-0.0135922621477581));
#19999=CARTESIAN_POINT('Ctrl Pts',(0.00536704035512664,-0.0392752442881333,
-0.0135830798332581));
#20000=CARTESIAN_POINT('Ctrl Pts',(0.0053591278513458,-0.0392747974925742,
-0.0135794940345151));
#20001=CARTESIAN_POINT('Ctrl Pts',(0.00534324601646462,-0.0392738889570015,
-0.0135721344014611));
#20002=CARTESIAN_POINT('Ctrl Pts',(0.00533527795192002,-0.039273427130702,
-0.0135683587042053));
#20003=CARTESIAN_POINT('Ctrl Pts',(0.00531420239727291,-0.0392721904587869,
-0.0135581498666673));
#20004=CARTESIAN_POINT('Ctrl Pts',(0.00530115337438712,-0.0392714090737808,
-0.0135515987396149));
#20005=CARTESIAN_POINT('Ctrl Pts',(0.00527203926043385,-0.0392696334575321,
-0.0135364612110366));
#20006=CARTESIAN_POINT('Ctrl Pts',(0.00525602937070322,-0.0392686345585567,
-0.0135277735573995));
#20007=CARTESIAN_POINT('Ctrl Pts',(0.00520443646351128,-0.0392653504626187,
-0.0134985830437455));
#20008=CARTESIAN_POINT('Ctrl Pts',(0.0051695183200595,-0.0392630255012293,
-0.0134769433051452));
#20009=CARTESIAN_POINT('Ctrl Pts',(0.00502926456191316,-0.0392533679337981,
-0.0133820759774999));
#20010=CARTESIAN_POINT('Ctrl Pts',(0.00493237841609905,-0.0392459766985508,
-0.0132972337122274));
#20011=CARTESIAN_POINT('Ctrl Pts',(0.0048305166975368,-0.0392377326885316,
-0.0131827201552549));
#20012=CARTESIAN_POINT('Ctrl Pts',(0.0048143809576707,-0.0392364074789784,
-0.0131636688904647));
#20013=CARTESIAN_POINT('Ctrl Pts',(0.00478891756095033,-0.0392342832560996,
-0.0131320812807735));
#20014=CARTESIAN_POINT('Ctrl Pts',(0.00477930595930315,-0.0392334732468315,
-0.0131197805790117));
#20015=CARTESIAN_POINT('Ctrl Pts',(0.00476095770797615,-0.0392319100803299,
-0.0130955498446295));
#20016=CARTESIAN_POINT('Ctrl Pts',(0.00475220264996732,-0.0392311562649615,
-0.0130836359438985));
#20017=CARTESIAN_POINT('Ctrl Pts',(0.00473170106261873,-0.0392293707410409,
-0.0130548802160828));
#20018=CARTESIAN_POINT('Ctrl Pts',(0.00472011669724982,-0.0392283451159299,
-0.013037925973519));
#20019=CARTESIAN_POINT('Ctrl Pts',(0.00467782647526548,-0.039224530357409,
-0.0129732999293021));
#20020=CARTESIAN_POINT('Ctrl Pts',(0.00464941657252458,-0.0392218222264274,
-0.0129241775015689));
#20021=CARTESIAN_POINT('Ctrl Pts',(0.00456857432880205,-0.0392134506605656,
-0.0127647251481053));
#20022=CARTESIAN_POINT('Ctrl Pts',(0.0045264948743849,-0.0392080363748214,
-0.0126496966453715));
#20023=CARTESIAN_POINT('Ctrl Pts',(0.00449254436710671,-0.0392009180337278,
-0.012506120026494));
#20024=CARTESIAN_POINT('Ctrl Pts',(0.00448729504029299,-0.0391996673600789,
-0.0124811763649061));
#20025=CARTESIAN_POINT('Ctrl Pts',(0.00448082614761093,-0.0391978780351706,
-0.0124461539039167));
#20026=CARTESIAN_POINT('Ctrl Pts',(0.00447908437208494,-0.0391973644414086,
-0.0124361747419941));
#20027=CARTESIAN_POINT('Ctrl Pts',(0.00447609004540929,-0.0391964191387795,
-0.0124179623436085));
#20028=CARTESIAN_POINT('Ctrl Pts',(0.00447480563451979,-0.0391959891059064,
-0.0124097346486363));
#20029=CARTESIAN_POINT('Ctrl Pts',(0.00447220407531662,-0.0391950623656671,
-0.0123921358694383));
#20030=CARTESIAN_POINT('Ctrl Pts',(0.00447090645100197,-0.0391945647136088,
-0.0123827625726031));
#20031=CARTESIAN_POINT('Ctrl Pts',(0.00446742697084075,-0.0391931230174556,
-0.0123558056381653));
#20032=CARTESIAN_POINT('Ctrl Pts',(0.0044654617234968,-0.0391921684549766,
-0.012338196029259));
#20033=CARTESIAN_POINT('Ctrl Pts',(0.00445926803716274,-0.039188566267966,
-0.0122724428785937));
#20034=CARTESIAN_POINT('Ctrl Pts',(0.00445700000038672,-0.0391858460740657,
-0.0122241549811162));
#20035=CARTESIAN_POINT('Ctrl Pts',(0.004457,-0.0391830969983919,-0.012175853298912));
#20036=CARTESIAN_POINT('Origin',(0.006,-0.0418165664398416,-0.0121758532865581));
#20037=CARTESIAN_POINT('',(0.004457,-0.0401812248373849,-0.0121758532903003));
#20038=CARTESIAN_POINT('',(0.004457,-0.0400658559061629,-0.0121758532865568));
#20039=CARTESIAN_POINT('',(0.004457,-0.0418165664398416,-0.0121758532865581));
#20040=CARTESIAN_POINT('',(0.00445700008689307,-0.0400658264344116,-0.0121753354525968));
#20041=CARTESIAN_POINT('Ctrl Pts',(0.004457,-0.0400658559061629,-0.0121758532865556));
#20042=CARTESIAN_POINT('Ctrl Pts',(0.004457,-0.0400658460818209,-0.0121756806755878));
#20043=CARTESIAN_POINT('Ctrl Pts',(0.00445700002896424,-0.040065836257903,
-0.0121755080642658));
#20044=CARTESIAN_POINT('Ctrl Pts',(0.00445700008689307,-0.0400658264344116,
-0.0121753354525968));
#20045=CARTESIAN_POINT('Ctrl Pts',(0.004457,-0.0395660360928446,-0.012175853286222));
#20046=CARTESIAN_POINT('Ctrl Pts',(0.00445699999998617,-0.0395689601809892,
-0.0122393411137212));
#20047=CARTESIAN_POINT('Ctrl Pts',(0.00446091839675691,-0.0395719185953119,
-0.0123027659954965));
#20048=CARTESIAN_POINT('Ctrl Pts',(0.00447083410518774,-0.0395758801751546,
-0.012382716565834));
#20049=CARTESIAN_POINT('Ctrl Pts',(0.00447321763691439,-0.039576731730892,
-0.012399630679702));
#20050=CARTESIAN_POINT('Ctrl Pts',(0.00447732845847337,-0.039578067994637,
-0.0124256661550697));
#20051=CARTESIAN_POINT('Ctrl Pts',(0.00447885816470674,-0.039578542585737,
-0.0124348177651906));
#20052=CARTESIAN_POINT('Ctrl Pts',(0.00448186914994206,-0.0395794376342485,
-0.0124518832473571));
#20053=CARTESIAN_POINT('Ctrl Pts',(0.00448332996972611,-0.0395798570017059,
-0.0124598001585569));
#20054=CARTESIAN_POINT('Ctrl Pts',(0.00448701159110442,-0.0395808791127856,
-0.0124789132782396));
#20055=CARTESIAN_POINT('Ctrl Pts',(0.00448929477719453,-0.0395814851619161,
-0.012490096820538));
#20056=CARTESIAN_POINT('Ctrl Pts',(0.00449816946914826,-0.0395837412623587,
-0.0125312328576436));
#20057=CARTESIAN_POINT('Ctrl Pts',(0.00450552918193665,-0.0395854271244627,
-0.0125610108273582));
#20058=CARTESIAN_POINT('Ctrl Pts',(0.00452809564029531,-0.0395901154443399,
-0.012641887057726));
#20059=CARTESIAN_POINT('Ctrl Pts',(0.00454507052962667,-0.039593167209448,
-0.0126924476312603));
#20060=CARTESIAN_POINT('Ctrl Pts',(0.00460553185885785,-0.0396026230303215,
-0.012845730439032));
#20061=CARTESIAN_POINT('Ctrl Pts',(0.00465756145700691,-0.0396089946135861,
-0.012944710943898));
#20062=CARTESIAN_POINT('Ctrl Pts',(0.00473373784842731,-0.0396163414180909,
-0.0130579255775263));
#20063=CARTESIAN_POINT('Ctrl Pts',(0.00474816494768303,-0.0396176667909736,
-0.0130782835947885));
#20064=CARTESIAN_POINT('Ctrl Pts',(0.00477222898515148,-0.0396197752738234,
-0.0131105519281751));
#20065=CARTESIAN_POINT('Ctrl Pts',(0.00478156024751075,-0.0396205698415416,
-0.013122683687153));
#20066=CARTESIAN_POINT('Ctrl Pts',(0.00479993847770898,-0.0396220917113368,
-0.0131458558608025));
#20067=CARTESIAN_POINT('Ctrl Pts',(0.00480896113887782,-0.0396228198568822,
-0.013156913478584));
#20068=CARTESIAN_POINT('Ctrl Pts',(0.00483061749799173,-0.0396245243474121,
-0.0131827149840867));
#20069=CARTESIAN_POINT('Ctrl Pts',(0.00484337875531893,-0.0396254954007976,
-0.0131973488825598));
#20070=CARTESIAN_POINT('Ctrl Pts',(0.00488983962916297,-0.0396289191362715,
-0.0132486403230585));
#20071=CARTESIAN_POINT('Ctrl Pts',(0.00492503409007518,-0.0396313097846007,
-0.0132839042429659));
#20072=CARTESIAN_POINT('Ctrl Pts',(0.00501625070944102,-0.039637111644823,
-0.0133668563839947));
#20073=CARTESIAN_POINT('Ctrl Pts',(0.0050740919059058,-0.0396404565945327,
-0.0134123586816373));
#20074=CARTESIAN_POINT('Ctrl Pts',(0.00519945609416132,-0.0396474078313954,
-0.0134972334979307));
#20075=CARTESIAN_POINT('Ctrl Pts',(0.00526716454226148,-0.0396510092741038,
-0.0135359511054023));
#20076=CARTESIAN_POINT('Ctrl Pts',(0.00535048183107094,-0.0396555850980917,
-0.0135755610499423));
#20077=CARTESIAN_POINT('Ctrl Pts',(0.00536355064413303,-0.0396563069575054,
-0.0135815516412352));
#20078=CARTESIAN_POINT('Ctrl Pts',(0.00538458191855621,-0.0396574780605296,
-0.0135908387312328));
#20079=CARTESIAN_POINT('Ctrl Pts',(0.00539249185925064,-0.0396579206229256,
-0.0135942527633123));
#20080=CARTESIAN_POINT('Ctrl Pts',(0.00540814433960766,-0.0396588012915822,
-0.0136008536289086));
#20081=CARTESIAN_POINT('Ctrl Pts',(0.00541588499099693,-0.039659239183179,
-0.0136040440111532));
#20082=CARTESIAN_POINT('Ctrl Pts',(0.00543591648040582,-0.0396603777493729,
-0.0136121100945936));
#20083=CARTESIAN_POINT('Ctrl Pts',(0.00544824456491845,-0.0396610836405821,
-0.0136168910212299));
#20084=CARTESIAN_POINT('Ctrl Pts',(0.00550703656575312,-0.0396644692349134,
-0.0136388260033595));
#20085=CARTESIAN_POINT('Ctrl Pts',(0.00555424435601024,-0.0396672435708072,
-0.0136538936367112));
#20086=CARTESIAN_POINT('Ctrl Pts',(0.0056790908890079,-0.0396745876573639,
-0.0136872161606285));
#20087=CARTESIAN_POINT('Ctrl Pts',(0.00575756796721962,-0.0396792050576329,
-0.0137017719065238));
#20088=CARTESIAN_POINT('Ctrl Pts',(0.00590530365845703,-0.0396876257641781,
-0.0137174838069692));
#20089=CARTESIAN_POINT('Ctrl Pts',(0.00597420365527438,-0.0396914462293089,
-0.0137201746222118));
#20090=CARTESIAN_POINT('Ctrl Pts',(0.00606475895485893,-0.0396962895632833,
-0.0137176465625296));
#20091=CARTESIAN_POINT('Ctrl Pts',(0.00608644376786908,-0.039697436409106,
-0.0137165829081762));
#20092=CARTESIAN_POINT('Ctrl Pts',(0.0061212705641571,-0.0396992581136982,
-0.0137141369983417));
#20093=CARTESIAN_POINT('Ctrl Pts',(0.00613442928562905,-0.0396999417786248,
-0.0137130429655469));
#20094=CARTESIAN_POINT('Ctrl Pts',(0.00616193989285474,-0.0397013618300341,
-0.0137103997326108));
#20095=CARTESIAN_POINT('Ctrl Pts',(0.00617628738550642,-0.0397020971238992,
-0.0137088177675608));
#20096=CARTESIAN_POINT('Ctrl Pts',(0.00621086968106721,-0.0397038575724294,
-0.0137045127503296));
#20097=CARTESIAN_POINT('Ctrl Pts',(0.00623107696766215,-0.0397048763843797,
-0.0137015889328666));
#20098=CARTESIAN_POINT('Ctrl Pts',(0.00630925560918444,-0.0397087856133673,
-0.0136886882765062));
#20099=CARTESIAN_POINT('Ctrl Pts',(0.00636669824511389,-0.0397115861334585,
-0.0136758006093356));
#20100=CARTESIAN_POINT('Ctrl Pts',(0.00652498748898999,-0.0397192652334389,
-0.01363064738563));
#20101=CARTESIAN_POINT('Ctrl Pts',(0.0066234469541039,-0.0397239839481114,
-0.0135912506289183));
#20102=CARTESIAN_POINT('Ctrl Pts',(0.00675058766311486,-0.0397307704770935,
-0.013524518431139));
#20103=CARTESIAN_POINT('Ctrl Pts',(0.00678341738103955,-0.0397325938957296,
-0.0135057165685662));
#20104=CARTESIAN_POINT('Ctrl Pts',(0.00682618318486149,-0.0397351085568061,
-0.013479090829643));
#20105=CARTESIAN_POINT('Ctrl Pts',(0.00683676361891034,-0.0397357425099431,
-0.013472322867994));
#20106=CARTESIAN_POINT('Ctrl Pts',(0.00685407972656392,-0.0397368016850029,
-0.0134609460484393));
#20107=CARTESIAN_POINT('Ctrl Pts',(0.00686086379646569,-0.039737222234509,
-0.0134564114101728));
#20108=CARTESIAN_POINT('Ctrl Pts',(0.00687487027219414,-0.0397381028137609,
-0.0134468875333432));
#20109=CARTESIAN_POINT('Ctrl Pts',(0.00688208656972172,-0.0397385633348284,
-0.0134418901445758));
#20110=CARTESIAN_POINT('Ctrl Pts',(0.00690163617719632,-0.0397398287761829,
-0.0134281034858799));
#20111=CARTESIAN_POINT('Ctrl Pts',(0.00691388308186435,-0.0397406411248792,
-0.0134191939627801));
#20112=CARTESIAN_POINT('Ctrl Pts',(0.00694138527024765,-0.0397425066346812,
-0.0133985604829386));
#20113=CARTESIAN_POINT('Ctrl Pts',(0.00695655631047808,-0.039743565354146,
-0.0133867286250402));
#20114=CARTESIAN_POINT('Ctrl Pts',(0.00700676473713766,-0.0397471594444508,
-0.0133460387221165));
#20115=CARTESIAN_POINT('Ctrl Pts',(0.00704074826069482,-0.0397497433488598,
-0.0133159199019664));
#20116=CARTESIAN_POINT('Ctrl Pts',(0.0071603379273686,-0.039759277615963,
-0.0132001215302169));
#20117=CARTESIAN_POINT('Ctrl Pts',(0.0072371203506172,-0.0397662490460964,
-0.0131059343680073));
#20118=CARTESIAN_POINT('Ctrl Pts',(0.0073161122185734,-0.0397741937360752,
-0.0129816941172273));
#20119=CARTESIAN_POINT('Ctrl Pts',(0.00732956097787736,-0.0397755834594344,
-0.0129593062415404));
#20120=CARTESIAN_POINT('Ctrl Pts',(0.00735009576582189,-0.0397777677088479,
-0.0129230693359607));
#20121=CARTESIAN_POINT('Ctrl Pts',(0.00735755147133362,-0.0397785752273182,
-0.0129094365657447));
#20122=CARTESIAN_POINT('Ctrl Pts',(0.00737142021085156,-0.0397801063723915,
-0.012883141748329));
#20123=CARTESIAN_POINT('Ctrl Pts',(0.00737786691407778,-0.0397808311277069,
-0.0128704993456897));
#20124=CARTESIAN_POINT('Ctrl Pts',(0.00739246934299865,-0.0397825047471759,
-0.0128408596596795));
#20125=CARTESIAN_POINT('Ctrl Pts',(0.00740048987347598,-0.0397834488966269,
-0.0128237981150153));
#20126=CARTESIAN_POINT('Ctrl Pts',(0.00742678961478523,-0.0397866370344907,
-0.0127650810785836));
#20127=CARTESIAN_POINT('Ctrl Pts',(0.00744353936174462,-0.0397888304224039,
-0.0127227651139747));
#20128=CARTESIAN_POINT('Ctrl Pts',(0.00748269907194559,-0.0397945002806422,
-0.0126094318132611));
#20129=CARTESIAN_POINT('Ctrl Pts',(0.00750188267725668,-0.0397978945657103,
-0.0125374273333806));
#20130=CARTESIAN_POINT('Ctrl Pts',(0.00753033840288857,-0.0398048763289034,
-0.0123879016505579));
#20131=CARTESIAN_POINT('Ctrl Pts',(0.00753908032451722,-0.0398084571103968,
-0.0123105001430206));
#20132=CARTESIAN_POINT('Ctrl Pts',(0.00754257501519921,-0.0398131168772153,
-0.0122158370118193));
#20133=CARTESIAN_POINT('Ctrl Pts',(0.00754292117120714,-0.0398139622688355,
-0.0121988878666902));
#20134=CARTESIAN_POINT('Ctrl Pts',(0.00754302448302113,-0.0398152908681977,
-0.0121726857992518));
#20135=CARTESIAN_POINT('Ctrl Pts',(0.00754297775591906,-0.03981576414013,
-0.0121634345665358));
#20136=CARTESIAN_POINT('Ctrl Pts',(0.00754273467718935,-0.0398166582835102,
-0.0121461269897887));
#20137=CARTESIAN_POINT('Ctrl Pts',(0.0075425584006346,-0.0398170780977159,
-0.0121380709209956));
#20138=CARTESIAN_POINT('Ctrl Pts',(0.00754197839178268,-0.039818103523416,
-0.012118554628847));
#20139=CARTESIAN_POINT('Ctrl Pts',(0.00754150999009453,-0.0398187124954392,
-0.0121070969632715));
#20140=CARTESIAN_POINT('Ctrl Pts',(0.00753929842190308,-0.0398209938810427,
-0.0120646091393436));
#20141=CARTESIAN_POINT('Ctrl Pts',(0.00753674565490548,-0.0398227031046073,
-0.0120336300449794));
#20142=CARTESIAN_POINT('Ctrl Pts',(0.00752714590257337,-0.0398274835599751,
-0.01194859982358));
#20143=CARTESIAN_POINT('Ctrl Pts',(0.00751816807466509,-0.0398306061301149,
-0.0118948123749389));
#20144=CARTESIAN_POINT('Ctrl Pts',(0.00748268635084925,-0.0398400069593393,
-0.0117349013369808));
#20145=CARTESIAN_POINT('Ctrl Pts',(0.00744773233527904,-0.0398462485053601,
-0.01163099120274));
#20146=CARTESIAN_POINT('Ctrl Pts',(0.00739157201136306,-0.0398534939955782,
-0.0115087624520685));
#20147=CARTESIAN_POINT('Ctrl Pts',(0.0073805020312642,-0.0398548320192375,
-0.0114861453157445));
#20148=CARTESIAN_POINT('Ctrl Pts',(0.00736179953917276,-0.0398569554130959,
-0.0114501903906567));
#20149=CARTESIAN_POINT('Ctrl Pts',(0.00735451301810145,-0.0398577525369486,
-0.0114366786591717));
#20150=CARTESIAN_POINT('Ctrl Pts',(0.00734007426627104,-0.0398592761463249,
-0.0114108349169459));
#20151=CARTESIAN_POINT('Ctrl Pts',(0.00733295041468553,-0.0398600035329605,
-0.0113984889224063));
#20152=CARTESIAN_POINT('Ctrl Pts',(0.00731578241728123,-0.0398617014471663,
-0.0113696660092753));
#20153=CARTESIAN_POINT('Ctrl Pts',(0.00730559814277987,-0.039862666806145,
-0.0113532751280467));
#20154=CARTESIAN_POINT('Ctrl Pts',(0.00726855940314006,-0.0398660387756522,
-0.0112960854826945));
#20155=CARTESIAN_POINT('Ctrl Pts',(0.00724007749705524,-0.0398683859785276,
-0.0112563737176329));
#20156=CARTESIAN_POINT('Ctrl Pts',(0.00715693817872098,-0.0398746952289001,
-0.0111513611968108));
#20157=CARTESIAN_POINT('Ctrl Pts',(0.00709869069952535,-0.0398785454628627,
-0.0110891293298039));
#20158=CARTESIAN_POINT('Ctrl Pts',(0.00698514534496306,-0.0398856033503526,
-0.0109863274609203));
#20159=CARTESIAN_POINT('Ctrl Pts',(0.00693171780386809,-0.0398887812087911,
-0.0109440321518834));
#20160=CARTESIAN_POINT('Ctrl Pts',(0.00686406838453483,-0.0398928602024527,
-0.0108974035760309));
#20161=CARTESIAN_POINT('Ctrl Pts',(0.00685234946808485,-0.0398935687622146,
-0.0108895608651134));
#20162=CARTESIAN_POINT('Ctrl Pts',(0.00683334923586824,-0.039894723432986,
-0.0108772188994914));
#20163=CARTESIAN_POINT('Ctrl Pts',(0.00682613487775849,-0.0398951631914547,
-0.0108726175530123));
#20164=CARTESIAN_POINT('Ctrl Pts',(0.00681174510379856,-0.0398960437245047,
-0.0108636071937029));
#20165=CARTESIAN_POINT('Ctrl Pts',(0.00680457115034996,-0.0398964843735361,
-0.0108591964680366));
#20166=CARTESIAN_POINT('Ctrl Pts',(0.00678583756339993,-0.0398976386069337,
-0.0108478888616278));
#20167=CARTESIAN_POINT('Ctrl Pts',(0.00677422331734705,-0.0398983576679461,
-0.0108410842350629));
#20168=CARTESIAN_POINT('Ctrl Pts',(0.00671616944245609,-0.0399019632481599,
-0.0108080838832279));
#20169=CARTESIAN_POINT('Ctrl Pts',(0.00666848577528093,-0.039904959325451,
-0.0107841573085156));
#20170=CARTESIAN_POINT('Ctrl Pts',(0.00654009953284305,-0.0399129450479861,
-0.0107278583691635));
#20171=CARTESIAN_POINT('Ctrl Pts',(0.00645772584742924,-0.0399179801517972,
-0.0106997486032343));
#20172=CARTESIAN_POINT('Ctrl Pts',(0.00636495540209971,-0.0399233618993406,
-0.0106766092341851));
#20173=CARTESIAN_POINT('Ctrl Pts',(0.00635646922346127,-0.0399238517299959,
-0.0106745688798677));
#20174=CARTESIAN_POINT('Ctrl Pts',(0.00629713691159126,-0.0399272586245619,
-0.0106608349055305));
#20175=CARTESIAN_POINT('Ctrl Pts',(0.00624574040996592,-0.0399301170106963,
-0.0106516539867863));
#20176=CARTESIAN_POINT('Ctrl Pts',(0.00617395992439847,-0.0399339707724918,
-0.0106425581697567));
#20177=CARTESIAN_POINT('Ctrl Pts',(0.00615389805821313,-0.0399350332861197,
-0.0106404147793104));
#20178=CARTESIAN_POINT('Ctrl Pts',(0.00611960340003261,-0.0399368254789721,
-0.0106374297180434));
#20179=CARTESIAN_POINT('Ctrl Pts',(0.0061053907983198,-0.0399375611828223,
-0.0106363907676631));
#20180=CARTESIAN_POINT('Ctrl Pts',(0.00607617685179372,-0.0399390595911033,
-0.0106346616909453));
#20181=CARTESIAN_POINT('Ctrl Pts',(0.00606117571367919,-0.0399398215423974,
-0.0106339933708603));
#20182=CARTESIAN_POINT('Ctrl Pts',(0.00602267971937258,-0.0399417589455805,
-0.0106328410473603));
#20183=CARTESIAN_POINT('Ctrl Pts',(0.00599917888313545,-0.039942924538978,
-0.0106326745741643));
#20184=CARTESIAN_POINT('Ctrl Pts',(0.0058730508151825,-0.0399491018858477,
-0.0106346625767733));
#20185=CARTESIAN_POINT('Ctrl Pts',(0.00577083080892855,-0.0399538075807174,
-0.0106465173430247));
#20186=CARTESIAN_POINT('Ctrl Pts',(0.00558761675042572,-0.0399624038705263,
-0.010686560030393));
#20187=CARTESIAN_POINT('Ctrl Pts',(0.00550633429027897,-0.0399662881862747,
-0.0107114947681038));
#20188=CARTESIAN_POINT('Ctrl Pts',(0.00541193466877153,-0.039971291047019,
-0.0107492103923557));
#20189=CARTESIAN_POINT('Ctrl Pts',(0.00539644967006315,-0.0399721284833082,
-0.0107556921202117));
#20190=CARTESIAN_POINT('Ctrl Pts',(0.00537263195242766,-0.0399734471835964,
-0.0107661216566464));
#20191=CARTESIAN_POINT('Ctrl Pts',(0.00536422330733505,-0.0399739187431029,
-0.0107698938545947));
#20192=CARTESIAN_POINT('Ctrl Pts',(0.00534851763882525,-0.0399748117239256,
-0.0107771092681014));
#20193=CARTESIAN_POINT('Ctrl Pts',(0.00534121306705222,-0.0399752321304616,
-0.0107805347342034));
#20194=CARTESIAN_POINT('Ctrl Pts',(0.00532352906560271,-0.0399762619286851,
-0.0107889974257831));
#20195=CARTESIAN_POINT('Ctrl Pts',(0.00531317875105843,-0.0399768747537031,
-0.0107940940238631));
#20196=CARTESIAN_POINT('Ctrl Pts',(0.00527466949984423,-0.0399791900389964,
-0.0108135959370207));
#20197=CARTESIAN_POINT('Ctrl Pts',(0.00524689983696445,-0.0399809306734793,
-0.0108287492368905));
#20198=CARTESIAN_POINT('Ctrl Pts',(0.00517119065911777,-0.0399858369391649,
-0.0108731348803742));
#20199=CARTESIAN_POINT('Ctrl Pts',(0.00512435122326446,-0.0399890567326861,
-0.0109041461924806));
#20200=CARTESIAN_POINT('Ctrl Pts',(0.0049938707845171,-0.0399983893664667,
-0.0110011668572233));
#20201=CARTESIAN_POINT('Ctrl Pts',(0.00491522730228807,-0.0400044608068186,
-0.0110733751208373));
#20202=CARTESIAN_POINT('Ctrl Pts',(0.00482778135832493,-0.040011570750854,
-0.011172160394389));
#20203=CARTESIAN_POINT('Ctrl Pts',(0.0048113949695302,-0.0400129230991725,
-0.0111916205146361));
#20204=CARTESIAN_POINT('Ctrl Pts',(0.00478587034249132,-0.0400150633620491,
-0.0112235007301256));
#20205=CARTESIAN_POINT('Ctrl Pts',(0.00477642451753024,-0.0400158633690262,
-0.0112356675184692));
#20206=CARTESIAN_POINT('Ctrl Pts',(0.00475860274850668,-0.0400173889852931,
-0.0112593466226858));
#20207=CARTESIAN_POINT('Ctrl Pts',(0.00475020088785849,-0.0400181155600753,
-0.0112708373762771));
#20208=CARTESIAN_POINT('Ctrl Pts',(0.00473086249891991,-0.0400198063119157,
-0.0112980684097304));
#20209=CARTESIAN_POINT('Ctrl Pts',(0.00472005774684049,-0.0400207654539418,
-0.011313899601009));
#20210=CARTESIAN_POINT('Ctrl Pts',(0.00468332896438323,-0.0400240821854562,
-0.0113699289774251));
#20211=CARTESIAN_POINT('Ctrl Pts',(0.00465898039820578,-0.0400263830975167,
-0.0114111288024565));
#20212=CARTESIAN_POINT('Ctrl Pts',(0.00461716318795908,-0.0400305948554303,
-0.011490045922268));
#20213=CARTESIAN_POINT('Ctrl Pts',(0.004599227949821,-0.0400325153987042,
-0.0115274651103423));
#20214=CARTESIAN_POINT('Ctrl Pts',(0.00454276940954693,-0.0400390806108443,
-0.0116585694926437));
#20215=CARTESIAN_POINT('Ctrl Pts',(0.00451197370351692,-0.0400436332411471,
-0.0117552849964633));
#20216=CARTESIAN_POINT('Ctrl Pts',(0.0044864692753042,-0.0400495937006845,
-0.0118749866806608));
#20217=CARTESIAN_POINT('Ctrl Pts',(0.00448248922326357,-0.04005063973444,
-0.011895751640434));
#20218=CARTESIAN_POINT('Ctrl Pts',(0.00447726486689411,-0.0400522098437399,
-0.0119264023368553));
#20219=CARTESIAN_POINT('Ctrl Pts',(0.00447568753151272,-0.0400527171684212,
-0.0119362295185568));
#20220=CARTESIAN_POINT('Ctrl Pts',(0.00447302054450397,-0.0400536395276828,
-0.0119539387802783));
#20221=CARTESIAN_POINT('Ctrl Pts',(0.00447189662110966,-0.0400540527083957,
-0.0119618150605848));
#20222=CARTESIAN_POINT('Ctrl Pts',(0.00446979058969465,-0.0400548780374543,
-0.0119774367808808));
#20223=CARTESIAN_POINT('Ctrl Pts',(0.0044688062873025,-0.0400552899753772,
-0.0119851814262938));
#20224=CARTESIAN_POINT('Ctrl Pts',(0.00446664725485208,-0.0400562577788002,
-0.012003265237146));
#20225=CARTESIAN_POINT('Ctrl Pts',(0.00446551826907159,-0.0400568158812481,
-0.0120136093883288));
#20226=CARTESIAN_POINT('Ctrl Pts',(0.00445951735299476,-0.0400601122539036,
-0.0120742748694939));
#20227=CARTESIAN_POINT('Ctrl Pts',(0.00445701705122449,-0.0400629496465278,
-0.0121247865047283));
#20228=CARTESIAN_POINT('Ctrl Pts',(0.00445700008689307,-0.0400658264344116,
-0.0121753354525968));
#20229=CARTESIAN_POINT('Ctrl Pts',(0.004457,-0.0401812248373849,-0.0121758532940426));
#20230=CARTESIAN_POINT('Ctrl Pts',(0.00445699999994688,-0.040180635876834,
-0.0121649030018824));
#20231=CARTESIAN_POINT('Ctrl Pts',(0.00445711656713364,-0.0401800501844204,
-0.0121539516973495));
#20232=CARTESIAN_POINT('Ctrl Pts',(0.00445777372115888,-0.0401784091749531,
-0.0121230933874333));
#20233=CARTESIAN_POINT('Ctrl Pts',(0.00445858301204432,-0.0401773619855601,
-0.012103195046473));
#20234=CARTESIAN_POINT('Ctrl Pts',(0.00446065838074593,-0.0401755624340552,
-0.0120686513996819));
#20235=CARTESIAN_POINT('Ctrl Pts',(0.00446174894820756,-0.0401748048444127,
-0.0120539985110329));
#20236=CARTESIAN_POINT('Ctrl Pts',(0.00446444969679944,-0.0401732437697908,
-0.012023586661551));
#20237=CARTESIAN_POINT('Ctrl Pts',(0.00446609359473845,-0.0401724414087836,
-0.0120078323887594));
#20238=CARTESIAN_POINT('Ctrl Pts',(0.00447108784806639,-0.0401703359124529,
-0.0119661920993181));
#20239=CARTESIAN_POINT('Ctrl Pts',(0.00447485297155762,-0.0401690454846411,
-0.0119403605706036));
#20240=CARTESIAN_POINT('Ctrl Pts',(0.00449363255762831,-0.040163635408136,
-0.0118310314728741));
#20241=CARTESIAN_POINT('Ctrl Pts',(0.00451486408403274,-0.0401597022010732,
-0.0117487493909857));
#20242=CARTESIAN_POINT('Ctrl Pts',(0.00456560682539897,-0.0401525996094248,
-0.0116029669746973));
#20243=CARTESIAN_POINT('Ctrl Pts',(0.00459287161515518,-0.0401494252726806,
-0.0115389299110801));
#20244=CARTESIAN_POINT('Ctrl Pts',(0.00463545219743835,-0.0401449590151719,
-0.0114551189031115));
#20245=CARTESIAN_POINT('Ctrl Pts',(0.00464706271274058,-0.0401437798563536,
-0.0114335532385743));
#20246=CARTESIAN_POINT('Ctrl Pts',(0.00466819035336545,-0.0401416834719464,
-0.0113964538337312));
#20247=CARTESIAN_POINT('Ctrl Pts',(0.00467747860489835,-0.0401407768206006,
-0.0113807950814925));
#20248=CARTESIAN_POINT('Ctrl Pts',(0.00469206472575814,-0.0401393696196115,
-0.0113571678985893));
#20249=CARTESIAN_POINT('Ctrl Pts',(0.00469716351239956,-0.040138880626556,
-0.011349077909768));
#20250=CARTESIAN_POINT('Ctrl Pts',(0.00470682864741006,-0.0401379580718214,
-0.0113340541572903));
#20251=CARTESIAN_POINT('Ctrl Pts',(0.004711376262438,-0.0401375256410104,
-0.0113271090535379));
#20252=CARTESIAN_POINT('Ctrl Pts',(0.00472151994265341,-0.0401365650275842,
-0.0113118871058551));
#20253=CARTESIAN_POINT('Ctrl Pts',(0.00472714076799248,-0.040136035341946,
-0.0113036272929654));
#20254=CARTESIAN_POINT('Ctrl Pts',(0.00474687769987846,-0.0401341859482964,
-0.0112752209307432));
#20255=CARTESIAN_POINT('Ctrl Pts',(0.00476139455948665,-0.0401328439239363,
-0.0112553585387399));
#20256=CARTESIAN_POINT('Ctrl Pts',(0.00485138826466713,-0.0401246706679953,
-0.0111382116256438));
#20257=CARTESIAN_POINT('Ctrl Pts',(0.00493781437787786,-0.0401174555169388,
-0.0110498989300811));
#20258=CARTESIAN_POINT('Ctrl Pts',(0.00507814701859921,-0.0401073656540049,
-0.0109371975835703));
#20259=CARTESIAN_POINT('Ctrl Pts',(0.00512440831636699,-0.0401042452452582,
-0.0109040745734365));
#20260=CARTESIAN_POINT('Ctrl Pts',(0.00518973768218066,-0.0401001228971598,
-0.0108625573745158));
#20261=CARTESIAN_POINT('Ctrl Pts',(0.00520729797308878,-0.0400990408257882,
-0.0108518839794864));
#20262=CARTESIAN_POINT('Ctrl Pts',(0.00523785311293039,-0.0400972014413967,
-0.0108341380561172));
#20263=CARTESIAN_POINT('Ctrl Pts',(0.00525074580059029,-0.0400964382313293,
-0.010826895984981));
#20264=CARTESIAN_POINT('Ctrl Pts',(0.00527745433556961,-0.040094882828721,
-0.0108123943536786));
#20265=CARTESIAN_POINT('Ctrl Pts',(0.00529128023460196,-0.0400940914597302,
-0.0108051568156108));
#20266=CARTESIAN_POINT('Ctrl Pts',(0.00532747939285731,-0.0400920536339528,
-0.0107869015718927));
#20267=CARTESIAN_POINT('Ctrl Pts',(0.00535001451932294,-0.0400908183803772,
-0.0107762141216076));
#20268=CARTESIAN_POINT('Ctrl Pts',(0.00549015401438133,-0.0400833203332449,
-0.0107138669531677));
#20269=CARTESIAN_POINT('Ctrl Pts',(0.00561356201952419,-0.0400775535039627,
-0.0106765157152171));
#20270=CARTESIAN_POINT('Ctrl Pts',(0.00578060631355024,-0.0400696932359926,
-0.0106479796427833));
#20271=CARTESIAN_POINT('Ctrl Pts',(0.00582129599906705,-0.0400677695528663,
-0.0106426879218692));
#20272=CARTESIAN_POINT('Ctrl Pts',(0.00588027475748021,-0.0400649120757031,
-0.0106373975153975));
#20273=CARTESIAN_POINT('Ctrl Pts',(0.00589843020376616,-0.0400640230111768,
-0.010636092322633));
#20274=CARTESIAN_POINT('Ctrl Pts',(0.00593117556479208,-0.0400623960117224,
-0.010634319909139));
#20275=CARTESIAN_POINT('Ctrl Pts',(0.0059457572392941,-0.0400616631311297,
-0.01063373796952));
#20276=CARTESIAN_POINT('Ctrl Pts',(0.00596915687348503,-0.0400604706216501,
-0.0106331363937962));
#20277=CARTESIAN_POINT('Ctrl Pts',(0.00597797084470707,-0.0400600176993975,
-0.0106329853665039));
#20278=CARTESIAN_POINT('Ctrl Pts',(0.0059954724680324,-0.0400591100979294,
-0.0106328354733705));
#20279=CARTESIAN_POINT('Ctrl Pts',(0.006004159746182,-0.0400586555405356,
-0.0106328344407947));
#20280=CARTESIAN_POINT('Ctrl Pts',(0.00602683198172644,-0.0400574594727238,
-0.0106330232061765));
#20281=CARTESIAN_POINT('Ctrl Pts',(0.00604081494898436,-0.0400567121197253,
-0.0106333297937456));
#20282=CARTESIAN_POINT('Ctrl Pts',(0.00611047336862383,-0.0400529471792749,
-0.0106358048982512));
#20283=CARTESIAN_POINT('Ctrl Pts',(0.00616600341077887,-0.0400498137250025,
-0.0106407978045264));
#20284=CARTESIAN_POINT('Ctrl Pts',(0.00631317247337864,-0.0400413477464493,
-0.0106621095352319));
#20285=CARTESIAN_POINT('Ctrl Pts',(0.00640382166846383,-0.0400359749604104,
-0.0106837315845034));
#20286=CARTESIAN_POINT('Ctrl Pts',(0.00654034606368712,-0.0400279427671415,
-0.0107296583363048));
#20287=CARTESIAN_POINT('Ctrl Pts',(0.00658788455097591,-0.0400251545052496,
-0.0107483217770079));
#20288=CARTESIAN_POINT('Ctrl Pts',(0.00665254565948249,-0.0400213833228971,
-0.0107774868128229));
#20289=CARTESIAN_POINT('Ctrl Pts',(0.0066705178407242,-0.0400203373203879,
-0.0107860149843751));
#20290=CARTESIAN_POINT('Ctrl Pts',(0.00670146240920835,-0.0400185394075941,
-0.0108014388294517));
#20291=CARTESIAN_POINT('Ctrl Pts',(0.0067145102467585,-0.0400177822852743,
-0.0108081765199103));
#20292=CARTESIAN_POINT('Ctrl Pts',(0.00674142551479173,-0.0400162218421084,
-0.0108225654478264));
#20293=CARTESIAN_POINT('Ctrl Pts',(0.00675527535502652,-0.04001541965048,
-0.010830246014736));
#20294=CARTESIAN_POINT('Ctrl Pts',(0.00679163995331315,-0.0400133139068312,
-0.0108511507358057));
#20295=CARTESIAN_POINT('Ctrl Pts',(0.00681394187386847,-0.0400120230857595,
-0.0108647356771748));
#20296=CARTESIAN_POINT('Ctrl Pts',(0.00691081761335415,-0.0400064025696993,
-0.0109271713596999));
#20297=CARTESIAN_POINT('Ctrl Pts',(0.00698142414794439,-0.0400022822898413,
-0.0109818669012067));
#20298=CARTESIAN_POINT('Ctrl Pts',(0.00709568112485136,-0.0399951303186407,
-0.011087396244405));
#20299=CARTESIAN_POINT('Ctrl Pts',(0.00714148773392469,-0.0399920927442163,
-0.0111355356218492));
#20300=CARTESIAN_POINT('Ctrl Pts',(0.00720640262278176,-0.0399872773634287,
-0.0112132230588179));
#20301=CARTESIAN_POINT('Ctrl Pts',(0.00722784099519396,-0.0399855870549997,
-0.0112407220454935));
#20302=CARTESIAN_POINT('Ctrl Pts',(0.0072554478415355,-0.0399832360743122,
-0.0112787209489036));
#20303=CARTESIAN_POINT('Ctrl Pts',(0.00726245141971938,-0.0399826232967991,
-0.0112886035416483));
#20304=CARTESIAN_POINT('Ctrl Pts',(0.00727407806896822,-0.0399815761320524,
-0.0113054260421249));
#20305=CARTESIAN_POINT('Ctrl Pts',(0.0072787626604972,-0.0399811456516794,
-0.0113123229914047));
#20306=CARTESIAN_POINT('Ctrl Pts',(0.00728862644620145,-0.0399802202154735,
-0.0113271013709235));
#20307=CARTESIAN_POINT('Ctrl Pts',(0.00729378957255423,-0.0399797243538421,
-0.0113349927361226));
#20308=CARTESIAN_POINT('Ctrl Pts',(0.00730835703616764,-0.0399782932379673,
-0.011357709597066));
#20309=CARTESIAN_POINT('Ctrl Pts',(0.0073175808687332,-0.0399773476903546,
-0.0113726485580136));
#20310=CARTESIAN_POINT('Ctrl Pts',(0.00736161887512091,-0.0399726468634982,
-0.0114467731550022));
#20311=CARTESIAN_POINT('Ctrl Pts',(0.00739270856398766,-0.0399687341462472,
-0.0115080768070202));
#20312=CARTESIAN_POINT('Ctrl Pts',(0.00744439709768179,-0.0399611849860902,
-0.0116294400717559));
#20313=CARTESIAN_POINT('Ctrl Pts',(0.0074655823188274,-0.0399575580285109,
-0.0116891095720938));
#20314=CARTESIAN_POINT('Ctrl Pts',(0.00749938259972236,-0.0399506805880792,
-0.0118067958176241));
#20315=CARTESIAN_POINT('Ctrl Pts',(0.00751243480359684,-0.0399474262906029,
-0.0118645757499254));
#20316=CARTESIAN_POINT('Ctrl Pts',(0.00752554220004797,-0.0399431644909464,
-0.0119434701026485));
#20317=CARTESIAN_POINT('Ctrl Pts',(0.00752853395107985,-0.039942069425714,
-0.0119640397747039));
#20318=CARTESIAN_POINT('Ctrl Pts',(0.00753294634577703,-0.0399402149959359,
-0.0119993757981228));
#20319=CARTESIAN_POINT('Ctrl Pts',(0.00753457127847003,-0.0399394494838702,
-0.012014113328108));
#20320=CARTESIAN_POINT('Ctrl Pts',(0.0075374631236616,-0.0399378952565843,
-0.0120443337523687));
#20321=CARTESIAN_POINT('Ctrl Pts',(0.00753870914690623,-0.0399371072633642,
-0.0120598169649866));
#20322=CARTESIAN_POINT('Ctrl Pts',(0.00754132194703761,-0.0399350907907916,
-0.0120998320952297));
#20323=CARTESIAN_POINT('Ctrl Pts',(0.007542337009579,-0.0399338730479364,
-0.0121243829473209));
#20324=CARTESIAN_POINT('Ctrl Pts',(0.00754490271431925,-0.0399266743253487,
-0.0122715044133184));
#20325=CARTESIAN_POINT('Ctrl Pts',(0.00753242995617212,-0.0399211404017791,
-0.012393874190513));
#20326=CARTESIAN_POINT('Ctrl Pts',(0.00749217880680639,-0.0399126362877349,
-0.0125733680256522));
#20327=CARTESIAN_POINT('Ctrl Pts',(0.00747518974740928,-0.0399097642755847,
-0.012632394223254));
#20328=CARTESIAN_POINT('Ctrl Pts',(0.00744905518544103,-0.0399059028752394,
-0.0127063041713141));
#20329=CARTESIAN_POINT('Ctrl Pts',(0.00744311209893908,-0.0399050525535822,
-0.0127222656748768));
#20330=CARTESIAN_POINT('Ctrl Pts',(0.0074335084510247,-0.0399037149184896,
-0.0127468081573597));
#20331=CARTESIAN_POINT('Ctrl Pts',(0.00743003208281494,-0.0399032374733162,
-0.0127554602028076));
#20332=CARTESIAN_POINT('Ctrl Pts',(0.0074233200266341,-0.0399023271763452,
-0.0127717372565016));
#20333=CARTESIAN_POINT('Ctrl Pts',(0.00742010101824096,-0.0399018952470575,
-0.0127793685643752));
#20334=CARTESIAN_POINT('Ctrl Pts',(0.00741274011529055,-0.0399009182254969,
-0.0127964340823686));
#20335=CARTESIAN_POINT('Ctrl Pts',(0.00740856484944494,-0.0399003712909099,
-0.0128058534543916));
#20336=CARTESIAN_POINT('Ctrl Pts',(0.00739312779361206,-0.0398983766293991,
-0.0128397586440691));
#20337=CARTESIAN_POINT('Ctrl Pts',(0.00738131974608067,-0.0398969018330847,
-0.0128639891576903));
#20338=CARTESIAN_POINT('Ctrl Pts',(0.00732765508390651,-0.0398904450897122,
-0.0129671580048346));
#20339=CARTESIAN_POINT('Ctrl Pts',(0.00727962126404893,-0.039885271311129,
-0.0130426866370688));
#20340=CARTESIAN_POINT('Ctrl Pts',(0.00717863886218274,-0.0398758059130695,
-0.0131746324503401));
#20341=CARTESIAN_POINT('Ctrl Pts',(0.00712746031583675,-0.0398715040160061,
-0.0132320657976271));
#20342=CARTESIAN_POINT('Ctrl Pts',(0.00705385904613277,-0.0398659924820446,
-0.0133031870515126));
#20343=CARTESIAN_POINT('Ctrl Pts',(0.00703506883535958,-0.039864636398005,
-0.0133204636630728));
#20344=CARTESIAN_POINT('Ctrl Pts',(0.00700402551975165,-0.0398624758327834,
-0.0133476164342518));
#20345=CARTESIAN_POINT('Ctrl Pts',(0.00699203535755855,-0.0398616596414898,
-0.0133577847531852));
#20346=CARTESIAN_POINT('Ctrl Pts',(0.00696851150286872,-0.039860092689147,
-0.0133771240743346));
#20347=CARTESIAN_POINT('Ctrl Pts',(0.00695699776118241,-0.0398593411221649,
-0.0133863165619317));
#20348=CARTESIAN_POINT('Ctrl Pts',(0.00692938492235703,-0.0398575737479358,
-0.0134077221586867));
#20349=CARTESIAN_POINT('Ctrl Pts',(0.00691317393719463,-0.0398565636789652,
-0.0134197868294619));
#20350=CARTESIAN_POINT('Ctrl Pts',(0.006856337959408,-0.0398531110049468,
-0.0134603757301412));
#20351=CARTESIAN_POINT('Ctrl Pts',(0.00681457572317758,-0.0398507277201316,
-0.0134872569363371));
#20352=CARTESIAN_POINT('Ctrl Pts',(0.00675858267759054,-0.0398476823092097,
-0.0135195894390562));
#20353=CARTESIAN_POINT('Ctrl Pts',(0.00674546852423048,-0.039846979168207,
-0.0135269088797831));
#20354=CARTESIAN_POINT('Ctrl Pts',(0.00666072847975548,-0.0398424922417613,
-0.0135725955613202));
#20355=CARTESIAN_POINT('Ctrl Pts',(0.00658627531055629,-0.0398388137929522,
-0.0136054448366188));
#20356=CARTESIAN_POINT('Ctrl Pts',(0.00645894969104511,-0.0398325273369262,
-0.0136499943157336));
#20357=CARTESIAN_POINT('Ctrl Pts',(0.00640743064427633,-0.0398299823707053,
-0.0136650564178983));
#20358=CARTESIAN_POINT('Ctrl Pts',(0.00634191545618927,-0.039826632122965,
-0.0136805559830389));
#20359=CARTESIAN_POINT('Ctrl Pts',(0.0063285534186693,-0.039825942951924,
-0.0136835299797456));
#20360=CARTESIAN_POINT('Ctrl Pts',(0.0063067092707106,-0.0398248042146958,
-0.0136880876736485));
#20361=CARTESIAN_POINT('Ctrl Pts',(0.00629825002464187,-0.0398243602948811,
-0.0136897787592414));
#20362=CARTESIAN_POINT('Ctrl Pts',(0.00628212820246123,-0.0398235079476141,
-0.0136928613032737));
#20363=CARTESIAN_POINT('Ctrl Pts',(0.00627446844570021,-0.039823100309428,
-0.0136942658499429));
#20364=CARTESIAN_POINT('Ctrl Pts',(0.00625325197977236,-0.0398219644512678,
-0.0136979904682242));
#20365=CARTESIAN_POINT('Ctrl Pts',(0.00623967466098199,-0.0398212299600893,
-0.0137001873040588));
#20366=CARTESIAN_POINT('Ctrl Pts',(0.00617655564368029,-0.0398177858692261,
-0.0137095359735397));
#20367=CARTESIAN_POINT('Ctrl Pts',(0.0061267169227291,-0.0398149830453155,
-0.0137144554332848));
#20368=CARTESIAN_POINT('Ctrl Pts',(0.00597919315170565,-0.0398065984356224,
-0.0137218006900586));
#20369=CARTESIAN_POINT('Ctrl Pts',(0.00588140606231653,-0.0398009426043927,
-0.0137173862474833));
#20370=CARTESIAN_POINT('Ctrl Pts',(0.005733039400861,-0.0397925784840061,
-0.0136964788117756));
#20371=CARTESIAN_POINT('Ctrl Pts',(0.00568178605135361,-0.039789726027195,
-0.0136865851071324));
#20372=CARTESIAN_POINT('Ctrl Pts',(0.00561168269060878,-0.0397858863281619,
-0.0136693256571105));
#20373=CARTESIAN_POINT('Ctrl Pts',(0.00559233151436458,-0.0397848328648956,
-0.0136641598778057));
#20374=CARTESIAN_POINT('Ctrl Pts',(0.00555895494323796,-0.0397830263723816,
-0.0136545501759719));
#20375=CARTESIAN_POINT('Ctrl Pts',(0.00554488270501247,-0.0397822679915335,
-0.0136502797852558));
#20376=CARTESIAN_POINT('Ctrl Pts',(0.00551583512666037,-0.0397807087042385,
-0.0136410094409908));
#20377=CARTESIAN_POINT('Ctrl Pts',(0.00550087112188317,-0.0397799088613901,
-0.0136359795029228));
#20378=CARTESIAN_POINT('Ctrl Pts',(0.00546161193663416,-0.0397778180029361,
-0.0136221089962299));
#20379=CARTESIAN_POINT('Ctrl Pts',(0.00543745679896261,-0.0397765393748755,
-0.0136128858279032));
#20380=CARTESIAN_POINT('Ctrl Pts',(0.00531892205585882,-0.0397702865112573,
-0.0135641784941042));
#20381=CARTESIAN_POINT('Ctrl Pts',(0.00522840109744926,-0.0397656017609241,
-0.0135159842058499));
#20382=CARTESIAN_POINT('Ctrl Pts',(0.00507633818917478,-0.0397571924103273,
-0.0134144743131082));
#20383=CARTESIAN_POINT('Ctrl Pts',(0.00501297346377977,-0.0397534808957977,
-0.0133645961004026));
#20384=CARTESIAN_POINT('Ctrl Pts',(0.00494186653268372,-0.0397487051032339,
-0.0132990033099942));
#20385=CARTESIAN_POINT('Ctrl Pts',(0.00493011182557243,-0.0397478933174103,
-0.0132878117686894));
#20386=CARTESIAN_POINT('Ctrl Pts',(0.00491200330152067,-0.0397466032932837,
-0.0132700178415358));
#20387=CARTESIAN_POINT('Ctrl Pts',(0.00490552777759662,-0.0397461338312949,
-0.0132635404822358));
#20388=CARTESIAN_POINT('Ctrl Pts',(0.00489325716545176,-0.0397452276129151,
-0.0132510458658604));
#20389=CARTESIAN_POINT('Ctrl Pts',(0.00488745264133763,-0.0397447915660869,
-0.0132450385595528));
#20390=CARTESIAN_POINT('Ctrl Pts',(0.00487294553290927,-0.0397436836556677,
-0.0132297786035136));
#20391=CARTESIAN_POINT('Ctrl Pts',(0.00486430797121918,-0.0397430072770849,
-0.0132204651480586));
#20392=CARTESIAN_POINT('Ctrl Pts',(0.00483076022009553,-0.0397403173538923,
-0.0131833843526046));
#20393=CARTESIAN_POINT('Ctrl Pts',(0.00480674668489662,-0.0397382524129708,
-0.013154825542188));
#20394=CARTESIAN_POINT('Ctrl Pts',(0.00472347268414423,-0.0397306466650612,
-0.0130481688067163));
#20395=CARTESIAN_POINT('Ctrl Pts',(0.00467065057179523,-0.0397249525323384,
-0.0129653388406234));
#20396=CARTESIAN_POINT('Ctrl Pts',(0.00459696386158113,-0.0397158252805594,
-0.012821160322121));
#20397=CARTESIAN_POINT('Ctrl Pts',(0.00457144578840077,-0.0397122995917525,
-0.0127625097948082));
#20398=CARTESIAN_POINT('Ctrl Pts',(0.00454239645416376,-0.0397077587772761,
-0.0126825000409533));
#20399=CARTESIAN_POINT('Ctrl Pts',(0.00453556845015233,-0.0397066400393274,
-0.0126624119417765));
#20400=CARTESIAN_POINT('Ctrl Pts',(0.00452465390485401,-0.0397047581673804,
-0.0126279869665255));
#20401=CARTESIAN_POINT('Ctrl Pts',(0.00452035701400596,-0.0397039884222852,
-0.0126137204116534));
#20402=CARTESIAN_POINT('Ctrl Pts',(0.00451203753660726,-0.0397024358429424,
-0.0125845758833694));
#20403=CARTESIAN_POINT('Ctrl Pts',(0.00450802986865213,-0.0397016535540137,
-0.012569695390064));
#20404=CARTESIAN_POINT('Ctrl Pts',(0.00449836542478563,-0.0396996730797273,
-0.0125315441848174));
#20405=CARTESIAN_POINT('Ctrl Pts',(0.0044930261482904,-0.0396984848640402,
-0.0125081969313366));
#20406=CARTESIAN_POINT('Ctrl Pts',(0.00446744827644895,-0.0396922254360072,
-0.0123830101099512));
#20407=CARTESIAN_POINT('Ctrl Pts',(0.004457,-0.039687465566661,-0.012279527802194));
#20408=CARTESIAN_POINT('Ctrl Pts',(0.004457,-0.0396826982119552,-0.0121758532865581));
#20409=CARTESIAN_POINT('Origin',(0.006,-0.0418165664398416,-0.0121758532865581));
#20410=CARTESIAN_POINT('',(0.00445636205606274,-0.040683589227672,-0.0121761473112929));
#20411=CARTESIAN_POINT('',(0.004457,-0.0405679692773165,-0.0121758532865581));
#20412=CARTESIAN_POINT('',(0.004457,-0.0418165664398416,-0.0121758532865581));
#20413=CARTESIAN_POINT('',(0.0066708408081921,-0.0408432743898683,-0.0135653933579799));
#20414=CARTESIAN_POINT('Ctrl Pts',(0.00445636205606274,-0.040683589227672,
-0.0121761473112929));
#20415=CARTESIAN_POINT('Ctrl Pts',(0.00445634241712689,-0.0406848802299932,
-0.0122003684416047));
#20416=CARTESIAN_POINT('Ctrl Pts',(0.00445690191082416,-0.0406861511658211,
-0.0122245773757201));
#20417=CARTESIAN_POINT('Ctrl Pts',(0.00445805707381056,-0.0406874049684561,
-0.0122487525271755));
#20418=CARTESIAN_POINT('Ctrl Pts',(0.00447278947892899,-0.0407033953772335,
-0.0125570710322108));
#20419=CARTESIAN_POINT('Ctrl Pts',(0.00458498283471403,-0.0407165990291478,
-0.0128616719032148));
#20420=CARTESIAN_POINT('Ctrl Pts',(0.00477117346292667,-0.040733100744054,
-0.0131079829187817));
#20421=CARTESIAN_POINT('Ctrl Pts',(0.00488365821068625,-0.0407430700494731,
-0.0132567886493516));
#20422=CARTESIAN_POINT('Ctrl Pts',(0.00502283501146244,-0.0407539848137185,
-0.0133847978149439));
#20423=CARTESIAN_POINT('Ctrl Pts',(0.00517953498196645,-0.0407638089246862,
-0.0134832713791425));
#20424=CARTESIAN_POINT('Ctrl Pts',(0.0051898898536264,-0.0407644581105662,
-0.0134897785987412));
#20425=CARTESIAN_POINT('Ctrl Pts',(0.0052003241170997,-0.0407651027688879,
-0.0134961588328292));
#20426=CARTESIAN_POINT('Ctrl Pts',(0.00521083657242243,-0.0407657432364286,
-0.0135024085181948));
#20427=CARTESIAN_POINT('Ctrl Pts',(0.00548429690826446,-0.0407824037085456,
-0.0136649814858335));
#20428=CARTESIAN_POINT('Ctrl Pts',(0.00581290359061553,-0.0407962283824575,
-0.0137394857874055));
#20429=CARTESIAN_POINT('Ctrl Pts',(0.00613310254693832,-0.0408131453283747,
-0.0137122202173662));
#20430=CARTESIAN_POINT('Ctrl Pts',(0.00631937727002341,-0.0408229867077857,
-0.0136963585588301));
#20431=CARTESIAN_POINT('Ctrl Pts',(0.00650283936617522,-0.0408336528440328,
-0.0136465014534069));
#20432=CARTESIAN_POINT('Ctrl Pts',(0.00667084080819075,-0.0408432743898699,
-0.0135653933579773));
#20433=CARTESIAN_POINT('',(0.00745756139467092,-0.0408425303804537,-0.0116656133925582));
#20434=CARTESIAN_POINT('Origin',(0.00600000000001,-0.0408432743898623,-0.0121758532865681));
#20435=CARTESIAN_POINT('Ctrl Pts',(0.00745636084418434,-0.0408417813214044,
-0.0116660865835196));
#20436=CARTESIAN_POINT('Ctrl Pts',(0.00746165020059864,-0.0408409726501889,
-0.0116811978325024));
#20437=CARTESIAN_POINT('Ctrl Pts',(0.00746670423706467,-0.0408401763062786,
-0.0116963910408018));
#20438=CARTESIAN_POINT('Ctrl Pts',(0.00748091109636588,-0.0408378574212748,
-0.0117414277196461));
#20439=CARTESIAN_POINT('Ctrl Pts',(0.00748939621149823,-0.0408363637400495,
-0.0117714743038455));
#20440=CARTESIAN_POINT('Ctrl Pts',(0.00752140454363981,-0.0408301444250377,
-0.0118995578575828));
#20441=CARTESIAN_POINT('Ctrl Pts',(0.0075362026694581,-0.0408256370371514,
-0.0119995186528621));
#20442=CARTESIAN_POINT('Ctrl Pts',(0.00754416486380153,-0.0408180759448483,
-0.0121617431562191));
#20443=CARTESIAN_POINT('Ctrl Pts',(0.00754349702246392,-0.0408151493490006,
-0.0122233951850473));
#20444=CARTESIAN_POINT('Ctrl Pts',(0.00753767474856551,-0.0408110849046505,
-0.0123056198926866));
#20445=CARTESIAN_POINT('Ctrl Pts',(0.0075357826221537,-0.0408100457985166,
-0.0123263680387618));
#20446=CARTESIAN_POINT('Ctrl Pts',(0.00753184734665668,-0.0408082549074869,
-0.0123616134192528));
#20447=CARTESIAN_POINT('Ctrl Pts',(0.00753001687733962,-0.0408075097373047,
-0.012376131734187));
#20448=CARTESIAN_POINT('Ctrl Pts',(0.0075258757163216,-0.0408059815367131,
-0.0124055942499645));
#20449=CARTESIAN_POINT('Ctrl Pts',(0.0075235512818924,-0.0408051981562626,
-0.0124205348799674));
#20450=CARTESIAN_POINT('Ctrl Pts',(0.00751706407621937,-0.0408031828835839,
-0.0124585458506635));
#20451=CARTESIAN_POINT('Ctrl Pts',(0.00751259453575199,-0.0408019416868216,
-0.0124815593366645));
#20452=CARTESIAN_POINT('Ctrl Pts',(0.00747958573376826,-0.0407936319400856,
-0.0126329986075741));
#20453=CARTESIAN_POINT('Ctrl Pts',(0.00743524769199549,-0.0407860585052013,
-0.0127574112264761));
#20454=CARTESIAN_POINT('Ctrl Pts',(0.00734999191524783,-0.0407753584871154,
-0.0129252458452654));
#20455=CARTESIAN_POINT('Ctrl Pts',(0.00732152704022689,-0.0407721704481418,
-0.0129743735538654));
#20456=CARTESIAN_POINT('Ctrl Pts',(0.00728286616919027,-0.040768366246518,
-0.0130333456575354));
#20457=CARTESIAN_POINT('Ctrl Pts',(0.00727515915993375,-0.0407676307868667,
-0.0130447652015192));
#20458=CARTESIAN_POINT('Ctrl Pts',(0.00726238827445254,-0.0407664505745708,
-0.0130631519834363));
#20459=CARTESIAN_POINT('Ctrl Pts',(0.00725741732687933,-0.0407660002590344,
-0.0130701825356703));
#20460=CARTESIAN_POINT('Ctrl Pts',(0.00724733488458996,-0.0407651054820061,
-0.0130841921601766));
#20461=CARTESIAN_POINT('Ctrl Pts',(0.00724222307824382,-0.0407646611126685,
-0.0130911705275256));
#20462=CARTESIAN_POINT('Ctrl Pts',(0.00722847101029089,-0.0407634890257665,
-0.0131096167086333));
#20463=CARTESIAN_POINT('Ctrl Pts',(0.00721972869714755,-0.0407627678562672,
-0.0131210078158341));
#20464=CARTESIAN_POINT('Ctrl Pts',(0.00716322392993987,-0.040758244510328,
-0.0131925427162463));
#20465=CARTESIAN_POINT('Ctrl Pts',(0.00711118158793278,-0.0407546851745562,
-0.0132491775622032));
#20466=CARTESIAN_POINT('Ctrl Pts',(0.00699813863725094,-0.040747559827924,
-0.0133551199350694));
#20467=CARTESIAN_POINT('Ctrl Pts',(0.00693717047657244,-0.0407440025590901,
-0.0134041291692879));
#20468=CARTESIAN_POINT('Ctrl Pts',(0.00683427346338951,-0.0407381054263292,
-0.0134747044620498));
#20469=CARTESIAN_POINT('Ctrl Pts',(0.00679461576248002,-0.0407358566580044,
-0.0134993380470959));
#20470=CARTESIAN_POINT('Ctrl Pts',(0.00673730244404835,-0.0407326016624396,
-0.0135314329339307));
#20471=CARTESIAN_POINT('Ctrl Pts',(0.00672053004103239,-0.0407316486708917,
-0.0135404218977194));
#20472=CARTESIAN_POINT('Ctrl Pts',(0.00669092545955046,-0.040729963705574,
-0.0135555901095967));
#20473=CARTESIAN_POINT('Ctrl Pts',(0.00667816582828285,-0.0407292365820017,
-0.0135619062376694));
#20474=CARTESIAN_POINT('Ctrl Pts',(0.00665132981715593,-0.0407277046601286,
-0.0135747310244224));
#20475=CARTESIAN_POINT('Ctrl Pts',(0.00663723910326167,-0.0407268988074884,
-0.0135812058253447));
#20476=CARTESIAN_POINT('Ctrl Pts',(0.00659939737363555,-0.0407247298313373,
-0.0135979082863153));
#20477=CARTESIAN_POINT('Ctrl Pts',(0.00657548352317444,-0.040723354125781,
-0.0136077528087148));
#20478=CARTESIAN_POINT('Ctrl Pts',(0.00645633253597576,-0.040716472909516,
-0.0136533362604753));
#20479=CARTESIAN_POINT('Ctrl Pts',(0.00635798105751931,-0.0407106865879567,
-0.0136801936378314));
#20480=CARTESIAN_POINT('Ctrl Pts',(0.00617678069143139,-0.040700134475921,
-0.0137108895387227));
#20481=CARTESIAN_POINT('Ctrl Pts',(0.00609487396701188,-0.0406954109239253,
-0.0137181205544821));
#20482=CARTESIAN_POINT('Ctrl Pts',(0.00599585040133589,-0.0406900099813477,
-0.0137189405510562));
#20483=CARTESIAN_POINT('Ctrl Pts',(0.00597892209000315,-0.0406890978688332,
-0.0137188021813164));
#20484=CARTESIAN_POINT('Ctrl Pts',(0.00595276283657161,-0.0406877091790826,
-0.0137181577331468));
#20485=CARTESIAN_POINT('Ctrl Pts',(0.00594352883045026,-0.0406872229925691,
-0.0137178472460173));
#20486=CARTESIAN_POINT('Ctrl Pts',(0.00592630323206072,-0.0406863242253804,
-0.0137171131017568));
#20487=CARTESIAN_POINT('Ctrl Pts',(0.00591831167343682,-0.040685910632611,
-0.0137167102074386));
#20488=CARTESIAN_POINT('Ctrl Pts',(0.00589899938271384,-0.0406849188701749,
-0.0137155859051825));
#20489=CARTESIAN_POINT('Ctrl Pts',(0.00588768294064504,-0.0406843440692333,
-0.0137148018088508));
#20490=CARTESIAN_POINT('Ctrl Pts',(0.00584591780513346,-0.0406822428076906,
-0.013711444821988));
#20491=CARTESIAN_POINT('Ctrl Pts',(0.00581553739024073,-0.040680753864107,
-0.0137080923172214));
#20492=CARTESIAN_POINT('Ctrl Pts',(0.00573268109587621,-0.0406767544661384,
-0.0136964486770872));
#20493=CARTESIAN_POINT('Ctrl Pts',(0.00568050128306055,-0.0406743029842307,
-0.0136863468638638));
#20494=CARTESIAN_POINT('Ctrl Pts',(0.00552019613408895,-0.0406667241952723,
-0.0136466317472969));
#20495=CARTESIAN_POINT('Ctrl Pts',(0.00541471472872338,-0.0406616419864291,
-0.0136079288617161));
#20496=CARTESIAN_POINT('Ctrl Pts',(0.00529214236532736,-0.0406549636278507,
-0.0135471305502521));
#20497=CARTESIAN_POINT('Ctrl Pts',(0.00527019991226979,-0.0406537370427915,
-0.013535579550183));
#20498=CARTESIAN_POINT('Ctrl Pts',(0.00523529111460153,-0.0406517300025516,
-0.0135161143203821));
#20499=CARTESIAN_POINT('Ctrl Pts',(0.00522214631399861,-0.0406509611750179,
-0.0135085283933331));
#20500=CARTESIAN_POINT('Ctrl Pts',(0.00519699088545164,-0.0406494634091028,
-0.013493512105536));
#20501=CARTESIAN_POINT('Ctrl Pts',(0.00518496614254834,-0.0406487354857501,
-0.0134861082979582));
#20502=CARTESIAN_POINT('Ctrl Pts',(0.00515687739360278,-0.0406470060111948,
-0.0134682773640541));
#20503=CARTESIAN_POINT('Ctrl Pts',(0.00514090280802337,-0.0406459994918813,
-0.0134577143149038));
#20504=CARTESIAN_POINT('Ctrl Pts',(0.00508516633443893,-0.0406424042933358,
-0.0134193492017226));
#20505=CARTESIAN_POINT('Ctrl Pts',(0.00504652609213745,-0.0406397573343502,
-0.0133899741873596));
#20506=CARTESIAN_POINT('Ctrl Pts',(0.00494495204452492,-0.0406323763439658,
-0.0133049127154077));
#20507=CARTESIAN_POINT('Ctrl Pts',(0.00488508082990064,-0.0406275363409812,
-0.0132458321708397));
#20508=CARTESIAN_POINT('Ctrl Pts',(0.00478795735482854,-0.0406189912885865,
-0.0131329428069117));
#20509=CARTESIAN_POINT('Ctrl Pts',(0.00474874467329652,-0.0406152890207445,
-0.0130810764685347));
#20510=CARTESIAN_POINT('Ctrl Pts',(0.00470353989613774,-0.0406108167308208,
-0.0130127100087736));
#20511=CARTESIAN_POINT('Ctrl Pts',(0.00469439860491936,-0.0406099003905455,
-0.0129983756373753));
#20512=CARTESIAN_POINT('Ctrl Pts',(0.00468067616177849,-0.0406085094900141,
-0.0129760522052363));
#20513=CARTESIAN_POINT('Ctrl Pts',(0.00467592672674916,-0.0406080250971745,
-0.0129681686751539));
#20514=CARTESIAN_POINT('Ctrl Pts',(0.00466718162780741,-0.0406071282183929,
-0.0129533545227395));
#20515=CARTESIAN_POINT('Ctrl Pts',(0.00466316892978935,-0.0406067147234556,
-0.0129464346750234));
#20516=CARTESIAN_POINT('Ctrl Pts',(0.00465361627777243,-0.0406057249895091,
-0.0129296620362231));
#20517=CARTESIAN_POINT('Ctrl Pts',(0.00464813034171527,-0.0406051520537887,
-0.0129197788203857));
#20518=CARTESIAN_POINT('Ctrl Pts',(0.00462849552945023,-0.0406030812901228,
-0.0128834710371234));
#20519=CARTESIAN_POINT('Ctrl Pts',(0.00461500812658388,-0.0406016192119426,
-0.0128566947565149));
#20520=CARTESIAN_POINT('Ctrl Pts',(0.00458055023017565,-0.0405977262078779,
-0.0127830181463181));
#20521=CARTESIAN_POINT('Ctrl Pts',(0.00456112714799178,-0.0405953499949163,
-0.0127354354813212));
#20522=CARTESIAN_POINT('Ctrl Pts',(0.00450608667804092,-0.0405877146426372,
-0.0125786560336434));
#20523=CARTESIAN_POINT('Ctrl Pts',(0.00448026918262782,-0.0405825141736164,
-0.0124664452040318));
#20524=CARTESIAN_POINT('Ctrl Pts',(0.0044643475766838,-0.0405757193609202,
-0.0123282142499272));
#20525=CARTESIAN_POINT('Ctrl Pts',(0.00446213401693944,-0.0405745142893773,
-0.0123039562400101));
#20526=CARTESIAN_POINT('Ctrl Pts',(0.00445948135767097,-0.0405725347763589,
-0.0122646147806767));
#20527=CARTESIAN_POINT('Ctrl Pts',(0.00445868766174779,-0.0405717713111558,
-0.0122495590909445));
#20528=CARTESIAN_POINT('Ctrl Pts',(0.00445773365451917,-0.0405704886291275,
-0.0122244748679434));
#20529=CARTESIAN_POINT('Ctrl Pts',(0.00445745026688442,-0.0405699732731458,
-0.0122144519033791));
#20530=CARTESIAN_POINT('Ctrl Pts',(0.00445708819810097,-0.0405689623995923,
-0.0121949033226106));
#20531=CARTESIAN_POINT('Ctrl Pts',(0.004457,-0.040568467201217,-0.012185378332967));
#20532=CARTESIAN_POINT('Ctrl Pts',(0.004457,-0.0405679692773165,-0.012175853286558));
#20533=CARTESIAN_POINT('Origin',(-0.0125,-0.0375520664398416,-0.0121758532865581));
#20534=CARTESIAN_POINT('',(-0.014043,-0.0304166107246751,-0.0121758532865582));
#20535=CARTESIAN_POINT('',(-0.014043,-0.0303011972027429,-0.0121758532865251));
#20536=CARTESIAN_POINT('',(-0.014043,-0.0375520664398416,-0.012175853286558));
#20537=CARTESIAN_POINT('',(-0.0140434115472061,-0.030301351634873,-0.0121743803418281));
#20538=CARTESIAN_POINT('Ctrl Pts',(-0.014043,-0.0303011972027429,-0.0121758532864921));
#20539=CARTESIAN_POINT('Ctrl Pts',(-0.014043,-0.0303011717518023,-0.0121754036077484));
#20540=CARTESIAN_POINT('Ctrl Pts',(-0.0140429998034242,-0.0303011463056326,
-0.0121749539243807));
#20541=CARTESIAN_POINT('Ctrl Pts',(-0.0140429994102604,-0.0303011208642816,
-0.0121745042365161));
#20542=CARTESIAN_POINT('',(-0.0131954570230097,-0.0302142743898648,-0.0107984686165645));
#20543=CARTESIAN_POINT('Ctrl Pts',(-0.0140434115472061,-0.030301351634873,
-0.0121743803418281));
#20544=CARTESIAN_POINT('Ctrl Pts',(-0.0140434740875886,-0.0302984285463748,
-0.0121215468731317));
#20545=CARTESIAN_POINT('Ctrl Pts',(-0.0140408865195758,-0.030295616371813,
-0.0120687879599));
#20546=CARTESIAN_POINT('Ctrl Pts',(-0.0140354833210815,-0.030292885581712,
-0.0120163446339196));
#20547=CARTESIAN_POINT('Ctrl Pts',(-0.0140053197530325,-0.0302776408385983,
-0.011723577704556));
#20548=CARTESIAN_POINT('Ctrl Pts',(-0.0138865745209328,-0.0302649324214751,
-0.0114393196839804));
#20549=CARTESIAN_POINT('Ctrl Pts',(-0.0137019165735488,-0.0302496228389727,
-0.0112095557337391));
#20550=CARTESIAN_POINT('Ctrl Pts',(-0.0135646906639459,-0.0302382457419439,
-0.0110388099439558));
#20551=CARTESIAN_POINT('Ctrl Pts',(-0.0133911038022161,-0.0302255801464012,
-0.0108972480096383));
#20552=CARTESIAN_POINT('Ctrl Pts',(-0.0131954570230095,-0.0302142743898697,
-0.0107984686165644));
#20553=CARTESIAN_POINT('',(-0.0112093823259403,-0.030215088191226,-0.0113276377436708));
#20554=CARTESIAN_POINT('Origin',(-0.01249999999999,-0.0302142743898623,
-0.0121758532865681));
#20555=CARTESIAN_POINT('Ctrl Pts',(-0.0112106409242372,-0.0302159019925798,
-0.0113282672002234));
#20556=CARTESIAN_POINT('Ctrl Pts',(-0.0112128889480957,-0.0302161112403416,
-0.0113248474768335));
#20557=CARTESIAN_POINT('Ctrl Pts',(-0.0112151505937373,-0.0302163196178771,
-0.011321436671487));
#20558=CARTESIAN_POINT('Ctrl Pts',(-0.0112210324192457,-0.0302168561563185,
-0.0113126424122188));
#20559=CARTESIAN_POINT('Ctrl Pts',(-0.0112246730592058,-0.0302171830508598,
-0.011307272672607));
#20560=CARTESIAN_POINT('Ctrl Pts',(-0.0112417552471371,-0.0302186936789069,
-0.0112824163643799));
#20561=CARTESIAN_POINT('Ctrl Pts',(-0.0112556108209913,-0.0302198531818524,
-0.0112632169578027));
#20562=CARTESIAN_POINT('Ctrl Pts',(-0.0113363765789313,-0.0302262976394441,
-0.0111565625229546));
#20563=CARTESIAN_POINT('Ctrl Pts',(-0.0114120594196726,-0.0302311901234243,
-0.011076143186243));
#20564=CARTESIAN_POINT('Ctrl Pts',(-0.0115503847147757,-0.0302395951819232,
-0.0109575449019186));
#20565=CARTESIAN_POINT('Ctrl Pts',(-0.0116083213402903,-0.0302429855296231,
-0.0109145237014696));
#20566=CARTESIAN_POINT('Ctrl Pts',(-0.011686140488403,-0.0302475289600024,
-0.0108647876252495));
#20567=CARTESIAN_POINT('Ctrl Pts',(-0.0117034458035125,-0.0302485382710704,
-0.0108542021082295));
#20568=CARTESIAN_POINT('Ctrl Pts',(-0.0117300479054118,-0.0302500905181481,
-0.0108386420998857));
#20569=CARTESIAN_POINT('Ctrl Pts',(-0.0117391956082126,-0.0302506244087221,
-0.0108334164515111));
#20570=CARTESIAN_POINT('Ctrl Pts',(-0.011755221200139,-0.0302515601969005,
-0.0108244782036918));
#20571=CARTESIAN_POINT('Ctrl Pts',(-0.0117620751748523,-0.0302519605738842,
-0.0108207233943327));
#20572=CARTESIAN_POINT('Ctrl Pts',(-0.0117775990626936,-0.0302528678627463,
-0.010812371647127));
#20573=CARTESIAN_POINT('Ctrl Pts',(-0.0117862848463781,-0.0302533758191923,
-0.0108078050531642));
#20574=CARTESIAN_POINT('Ctrl Pts',(-0.0118099753534279,-0.0302547623492623,
-0.0107956366714528));
#20575=CARTESIAN_POINT('Ctrl Pts',(-0.011825061483457,-0.0302556464655072,
-0.0107881970298671));
#20576=CARTESIAN_POINT('Ctrl Pts',(-0.0119129398735264,-0.0302608045273133,
-0.010746632362917));
#20577=CARTESIAN_POINT('Ctrl Pts',(-0.0119881799830745,-0.0302652616617878,
-0.0107179954451448));
#20578=CARTESIAN_POINT('Ctrl Pts',(-0.0121503146253649,-0.0302748462115804,
-0.0106703899907418));
#20579=CARTESIAN_POINT('Ctrl Pts',(-0.0122373199868089,-0.0302799787493356,
-0.010652797567));
#20580=CARTESIAN_POINT('Ctrl Pts',(-0.0123500996803343,-0.0302863335257897,
-0.0106399499032247));
#20581=CARTESIAN_POINT('Ctrl Pts',(-0.0123749113486741,-0.0302877125198554,
-0.0106377303254376));
#20582=CARTESIAN_POINT('Ctrl Pts',(-0.0124165652710717,-0.0302899843268226,
-0.0106350187631249));
#20583=CARTESIAN_POINT('Ctrl Pts',(-0.01243338112176,-0.0302908896808708,
-0.0106342001636292));
#20584=CARTESIAN_POINT('Ctrl Pts',(-0.0124571390710527,-0.0302921490056019,
-0.0106334330987397));
#20585=CARTESIAN_POINT('Ctrl Pts',(-0.0124640720731839,-0.0302925141217255,
-0.0106332560343302));
#20586=CARTESIAN_POINT('Ctrl Pts',(-0.0124759986750655,-0.0302931378521079,
-0.0106330318871608));
#20587=CARTESIAN_POINT('Ctrl Pts',(-0.0124809917118446,-0.0302933976588468,
-0.010632962292051));
#20588=CARTESIAN_POINT('Ctrl Pts',(-0.0124914516749318,-0.0302939390487119,
-0.0106328672814104));
#20589=CARTESIAN_POINT('Ctrl Pts',(-0.0124969185598081,-0.0302942203644687,
-0.0106328466785202));
#20590=CARTESIAN_POINT('Ctrl Pts',(-0.0125118384323821,-0.0302949839072028,
-0.0106328697450744));
#20591=CARTESIAN_POINT('Ctrl Pts',(-0.0125212912340889,-0.0302954630580415,
-0.0106329712270566));
#20592=CARTESIAN_POINT('Ctrl Pts',(-0.0125683923754362,-0.0302978301556941,
-0.0106339098563435));
#20593=CARTESIAN_POINT('Ctrl Pts',(-0.0126060046113189,-0.0302996555214584,
-0.0106360382098715));
#20594=CARTESIAN_POINT('Ctrl Pts',(-0.0127448491660251,-0.0303062714341073,
-0.0106490073839222));
#20595=CARTESIAN_POINT('Ctrl Pts',(-0.0128450132129234,-0.0303108171694383,
-0.0106684788984534));
#20596=CARTESIAN_POINT('Ctrl Pts',(-0.0130113085475643,-0.0303188633900924,
-0.0107182640257786));
#20597=CARTESIAN_POINT('Ctrl Pts',(-0.0130785559003934,-0.0303222636577658,
-0.0107436261684833));
#20598=CARTESIAN_POINT('Ctrl Pts',(-0.0131588080123629,-0.0303266406798236,
-0.0107804701562242));
#20599=CARTESIAN_POINT('Ctrl Pts',(-0.013173713863844,-0.0303274675381767,
-0.0107876055850281));
#20600=CARTESIAN_POINT('Ctrl Pts',(-0.0131971681214754,-0.0303287920357033,
-0.0107992998423665));
#20601=CARTESIAN_POINT('Ctrl Pts',(-0.0132057933493018,-0.0303292842278123,
-0.0108037022318877));
#20602=CARTESIAN_POINT('Ctrl Pts',(-0.0132212290482677,-0.0303301745192883,
-0.0108117647887721));
#20603=CARTESIAN_POINT('Ctrl Pts',(-0.0132280545721877,-0.0303305715687269,
-0.0108153955301812));
#20604=CARTESIAN_POINT('Ctrl Pts',(-0.0132440356719109,-0.0303315092894806,
-0.0108240511600488));
#20605=CARTESIAN_POINT('Ctrl Pts',(-0.0132531680111097,-0.030332051445356,
-0.0108291179710081));
#20606=CARTESIAN_POINT('Ctrl Pts',(-0.0132797871363435,-0.0303336505949328,
-0.0108442422521422));
#20607=CARTESIAN_POINT('Ctrl Pts',(-0.0132971285023787,-0.0303347165555468,
-0.0108545501329503));
#20608=CARTESIAN_POINT('Ctrl Pts',(-0.0133754308831641,-0.0303396431246271,
-0.0109031964207954));
#20609=CARTESIAN_POINT('Ctrl Pts',(-0.0134338571581009,-0.0303436450810037,
-0.0109454291875043));
#20610=CARTESIAN_POINT('Ctrl Pts',(-0.0135424034645513,-0.0303516853163875,
-0.0110360882473248));
#20611=CARTESIAN_POINT('Ctrl Pts',(-0.0135926253810445,-0.0303557073647253,
-0.0110841396476955));
#20612=CARTESIAN_POINT('Ctrl Pts',(-0.0136824149249653,-0.030363332887136,
-0.0111824722038504));
#20613=CARTESIAN_POINT('Ctrl Pts',(-0.0137224376692887,-0.0303669352308319,
-0.0112321591360074));
#20614=CARTESIAN_POINT('Ctrl Pts',(-0.0137652657179544,-0.0303709162266439,
-0.0112926437247606));
#20615=CARTESIAN_POINT('Ctrl Pts',(-0.0137711711424191,-0.0303714682133485,
-0.0113011645389617));
#20616=CARTESIAN_POINT('Ctrl Pts',(-0.0137801872895065,-0.0303723149476296,
-0.0113144579412226));
#20617=CARTESIAN_POINT('Ctrl Pts',(-0.013783358111617,-0.0303726135168364,
-0.0113191891770197));
#20618=CARTESIAN_POINT('Ctrl Pts',(-0.0137891462105387,-0.0303731598292146,
-0.0113279299573756));
#20619=CARTESIAN_POINT('Ctrl Pts',(-0.013791771064165,-0.0303734080630411,
-0.0113319341890156));
#20620=CARTESIAN_POINT('Ctrl Pts',(-0.0137977440881499,-0.0303739740860938,
-0.0113411392414262));
#20621=CARTESIAN_POINT('Ctrl Pts',(-0.0138010796582745,-0.0303742910432325,
-0.0113463480238528));
#20622=CARTESIAN_POINT('Ctrl Pts',(-0.013811473055066,-0.0303752818755205,
-0.0113627951499489));
#20623=CARTESIAN_POINT('Ctrl Pts',(-0.0138184174443557,-0.0303759486566424,
-0.0113741048393859));
#20624=CARTESIAN_POINT('Ctrl Pts',(-0.0138541184080652,-0.0303794096330583,
-0.0114339662291199));
#20625=CARTESIAN_POINT('Ctrl Pts',(-0.0138803438739666,-0.0303820691261823,
-0.0114839826899219));
#20626=CARTESIAN_POINT('Ctrl Pts',(-0.01395035767675,-0.0303898718469728,
-0.0116374243898987));
#20627=CARTESIAN_POINT('Ctrl Pts',(-0.013985665331939,-0.0303948723338038,
-0.0117442957161421));
#20628=CARTESIAN_POINT('Ctrl Pts',(-0.0140178041752537,-0.0304022027895388,
-0.0118950095262979));
#20629=CARTESIAN_POINT('Ctrl Pts',(-0.0140248664408474,-0.0304042351083484,
-0.0119363022550097));
#20630=CARTESIAN_POINT('Ctrl Pts',(-0.0140320427969083,-0.0304070201462079,
-0.011991757857305));
#20631=CARTESIAN_POINT('Ctrl Pts',(-0.0140336549765975,-0.0304077254412494,
-0.0120057102446011));
#20632=CARTESIAN_POINT('Ctrl Pts',(-0.0140359948986158,-0.0304088964065686,
-0.0120287104303252));
#20633=CARTESIAN_POINT('Ctrl Pts',(-0.014036833689447,-0.0304093585306091,
-0.0120377462446039));
#20634=CARTESIAN_POINT('Ctrl Pts',(-0.0140382682270244,-0.030410236737763,
-0.0120548364195145));
#20635=CARTESIAN_POINT('Ctrl Pts',(-0.0140388805381732,-0.0304106522778035,
-0.0120628891051825));
#20636=CARTESIAN_POINT('Ctrl Pts',(-0.0140400011847363,-0.030411504526978,
-0.0120793337069593));
#20637=CARTESIAN_POINT('Ctrl Pts',(-0.0140405042043225,-0.0304119413906177,
-0.0120877257034955));
#20638=CARTESIAN_POINT('Ctrl Pts',(-0.014041543983286,-0.0304129922645103,
-0.0121078209656391));
#20639=CARTESIAN_POINT('Ctrl Pts',(-0.0140420160767744,-0.0304136082954006,
-0.0121195269361538));
#20640=CARTESIAN_POINT('Ctrl Pts',(-0.0140427849275548,-0.0304150159869659,
-0.0121461055473814));
#20641=CARTESIAN_POINT('Ctrl Pts',(-0.014043,-0.0304158101282949,-0.0121609792078244));
#20642=CARTESIAN_POINT('Ctrl Pts',(-0.014043,-0.0304166107246751,-0.0121758532865585));
#20643=CARTESIAN_POINT('Origin',(-0.0125,-0.0375520664398416,-0.0121758532865581));
#20644=CARTESIAN_POINT('',(-0.014043,-0.0309187674107451,-0.0121758533048158));
#20645=CARTESIAN_POINT('',(-0.014043,-0.0308032888456207,-0.0121758532865568));
#20646=CARTESIAN_POINT('',(-0.014043,-0.0375520664398416,-0.012175853286558));
#20647=CARTESIAN_POINT('',(-0.0140429998315375,-0.0308032493790877,-0.0121751322628013));
#20648=CARTESIAN_POINT('Ctrl Pts',(-0.014043,-0.0308032888456207,-0.0121758532865555));
#20649=CARTESIAN_POINT('Ctrl Pts',(-0.014043,-0.0308032755095055,-0.0121756096173267));
#20650=CARTESIAN_POINT('Ctrl Pts',(-0.0140429999454013,-0.0308032627183605,
-0.0121753759327705));
#20651=CARTESIAN_POINT('Ctrl Pts',(-0.0140429998315375,-0.0308032493790877,
-0.0121751322628013));
#20652=CARTESIAN_POINT('Ctrl Pts',(-0.0140429998315375,-0.0308032493790877,
-0.0121751322628013));
#20653=CARTESIAN_POINT('Ctrl Pts',(-0.0140429494230278,-0.0307973439656581,
-0.0120672574234215));
#20654=CARTESIAN_POINT('Ctrl Pts',(-0.0140315862929371,-0.0307911149504177,
-0.0119596942407359));
#20655=CARTESIAN_POINT('Ctrl Pts',(-0.0139938756588056,-0.0307807274271626,
-0.0117827611841786));
#20656=CARTESIAN_POINT('Ctrl Pts',(-0.0139735908635154,-0.0307765709606792,
-0.0117124767654398));
#20657=CARTESIAN_POINT('Ctrl Pts',(-0.0139448135370339,-0.0307720887975717,
-0.0116341235815599));
#20658=CARTESIAN_POINT('Ctrl Pts',(-0.0139411281066165,-0.0307715350731643,
-0.0116243942926599));
#20659=CARTESIAN_POINT('Ctrl Pts',(-0.013935300213029,-0.0307706907111287,
-0.011609466585592));
#20660=CARTESIAN_POINT('Ctrl Pts',(-0.0139332273368253,-0.0307703961576646,
-0.0116042415306437));
#20661=CARTESIAN_POINT('Ctrl Pts',(-0.0139293354291963,-0.0307698538238913,
-0.0115945855594669));
#20662=CARTESIAN_POINT('Ctrl Pts',(-0.013927524313414,-0.0307696056024641,
-0.0115901517628385));
#20663=CARTESIAN_POINT('Ctrl Pts',(-0.0139233370211045,-0.0307690410349654,
-0.0115800356499321));
#20664=CARTESIAN_POINT('Ctrl Pts',(-0.0139209474430705,-0.0307687254998222,
-0.0115743590652198));
#20665=CARTESIAN_POINT('Ctrl Pts',(-0.0139132388108628,-0.0307677279934698,
-0.0115563490791319));
#20666=CARTESIAN_POINT('Ctrl Pts',(-0.0139077925512098,-0.030767053299491,
-0.0115440704477702));
#20667=CARTESIAN_POINT('Ctrl Pts',(-0.013859620407409,-0.0307613235492035,
-0.0114391830807388));
#20668=CARTESIAN_POINT('Ctrl Pts',(-0.0138079652272933,-0.0307567183531191,
-0.0113509397503003));
#20669=CARTESIAN_POINT('Ctrl Pts',(-0.0137072622140268,-0.0307488878584575,
-0.011212443082351));
#20670=CARTESIAN_POINT('Ctrl Pts',(-0.0136628308683721,-0.0307457059712628,
-0.0111592585208379));
#20671=CARTESIAN_POINT('Ctrl Pts',(-0.0135962327657241,-0.0307411088261712,
-0.0110896404486581));
#20672=CARTESIAN_POINT('Ctrl Pts',(-0.0135769715949999,-0.0307397975107651,
-0.0110705403487544));
#20673=CARTESIAN_POINT('Ctrl Pts',(-0.0135420153704053,-0.0307374400390593,
-0.0110376579695552));
#20674=CARTESIAN_POINT('Ctrl Pts',(-0.0135265249687069,-0.0307364026865651,
-0.0110236679507206));
#20675=CARTESIAN_POINT('Ctrl Pts',(-0.0135027982186729,-0.0307348219970792,
-0.0110030977037257));
#20676=CARTESIAN_POINT('Ctrl Pts',(-0.0134947701279002,-0.0307342885380063,
-0.0109962803511566));
#20677=CARTESIAN_POINT('Ctrl Pts',(-0.0134801371148019,-0.0307333183483052,
-0.0109841098140687));
#20678=CARTESIAN_POINT('Ctrl Pts',(-0.0134735565062655,-0.0307328828174035,
-0.0109787279826328));
#20679=CARTESIAN_POINT('Ctrl Pts',(-0.0134593177176003,-0.0307319419320742,
-0.0109672781006363));
#20680=CARTESIAN_POINT('Ctrl Pts',(-0.0134516457264063,-0.030731435886214,
-0.0109612278838804));
#20681=CARTESIAN_POINT('Ctrl Pts',(-0.0134306989216477,-0.0307300564533405,
-0.0109450292875952));
#20682=CARTESIAN_POINT('Ctrl Pts',(-0.0134173161417123,-0.0307291775103342,
-0.0109350232153287));
#20683=CARTESIAN_POINT('Ctrl Pts',(-0.0133281770452895,-0.0307233368788353,
-0.0108706057229196));
#20684=CARTESIAN_POINT('Ctrl Pts',(-0.0132477935132545,-0.0307181168976065,
-0.0108229494442921));
#20685=CARTESIAN_POINT('Ctrl Pts',(-0.0131031361488627,-0.030708945922402,
-0.0107540364882219));
#20686=CARTESIAN_POINT('Ctrl Pts',(-0.0130408494877025,-0.030705066069523,
-0.0107291957277703));
#20687=CARTESIAN_POINT('Ctrl Pts',(-0.0129292148328437,-0.0306983982392364,
-0.0106928954607309));
#20688=CARTESIAN_POINT('Ctrl Pts',(-0.0128805447208854,-0.030695582858372,
-0.0106796661776394));
#20689=CARTESIAN_POINT('Ctrl Pts',(-0.0128217893157134,-0.0306923591810636,
-0.0106667490244168));
#20690=CARTESIAN_POINT('Ctrl Pts',(-0.0128122480998191,-0.0306918411466117,
-0.0106647460198662));
#20691=CARTESIAN_POINT('Ctrl Pts',(-0.0127973060332986,-0.0306910390824373,
-0.0106617567735114));
#20692=CARTESIAN_POINT('Ctrl Pts',(-0.0127919179712198,-0.0306907517241886,
-0.0106607087297013));
#20693=CARTESIAN_POINT('Ctrl Pts',(-0.0127817729305266,-0.0306902143185438,
-0.0106587915218718));
#20694=CARTESIAN_POINT('Ctrl Pts',(-0.0127770173567079,-0.0306899639288118,
-0.0106579159470733));
#20695=CARTESIAN_POINT('Ctrl Pts',(-0.0127659386821497,-0.0306893840463748,
-0.0106559299891024));
#20696=CARTESIAN_POINT('Ctrl Pts',(-0.0127596125704511,-0.0306890555078882,
-0.0106548366762317));
#20697=CARTESIAN_POINT('Ctrl Pts',(-0.0127392376551842,-0.0306880051445119,
-0.0106514461940434));
#20698=CARTESIAN_POINT('Ctrl Pts',(-0.0127251634641828,-0.030687291472665,
-0.0106493038832516));
#20699=CARTESIAN_POINT('Ctrl Pts',(-0.0126312431836584,-0.0306825961354117,
-0.0106363349802867));
#20700=CARTESIAN_POINT('Ctrl Pts',(-0.0125506762103103,-0.0306788865497949,
-0.01063158133982));
#20701=CARTESIAN_POINT('Ctrl Pts',(-0.0123601624331091,-0.0306701592498833,
-0.0106352737465537));
#20702=CARTESIAN_POINT('Ctrl Pts',(-0.0122507770236676,-0.0306651636470311,
-0.0106491490349497));
#20703=CARTESIAN_POINT('Ctrl Pts',(-0.0121201739451476,-0.0306586079110084,
-0.0106801358558692));
#20704=CARTESIAN_POINT('Ctrl Pts',(-0.0120966873110969,-0.0306574062505756,
-0.0106862972255519));
#20705=CARTESIAN_POINT('Ctrl Pts',(-0.01206260818613,-0.0306556250520392,
-0.0106961024654139));
#20706=CARTESIAN_POINT('Ctrl Pts',(-0.0120518939316198,-0.0306550595703174,
-0.0106993117075613));
#20707=CARTESIAN_POINT('Ctrl Pts',(-0.0120330202214829,-0.0306540533484992,
-0.0107051892984499));
#20708=CARTESIAN_POINT('Ctrl Pts',(-0.0120248463055414,-0.0306536141938463,
-0.0107078098123495));
#20709=CARTESIAN_POINT('Ctrl Pts',(-0.0120077550872787,-0.0306526886876185,
-0.010713446859534));
#20710=CARTESIAN_POINT('Ctrl Pts',(-0.0119988426941627,-0.0306522018978928,
-0.0107164770631535));
#20711=CARTESIAN_POINT('Ctrl Pts',(-0.0119753903193451,-0.0306509096765467,
-0.0107246910089749));
#20712=CARTESIAN_POINT('Ctrl Pts',(-0.0119608996873145,-0.030650099723648,
-0.0107300116277281));
#20713=CARTESIAN_POINT('Ctrl Pts',(-0.0118949290143646,-0.0306463582493014,
-0.0107553641233125));
#20714=CARTESIAN_POINT('Ctrl Pts',(-0.0118444725404604,-0.0306433425308871,
-0.0107779322920615));
#20715=CARTESIAN_POINT('Ctrl Pts',(-0.0117084441162718,-0.0306347961772676,
-0.0108477611972743));
#20716=CARTESIAN_POINT('Ctrl Pts',(-0.0116259853465121,-0.0306291196217377,
-0.0109005159723672));
#20717=CARTESIAN_POINT('Ctrl Pts',(-0.0115054938057397,-0.0306203765260033,
-0.0109948076630089));
#20718=CARTESIAN_POINT('Ctrl Pts',(-0.0114637760304338,-0.030617255673004,
-0.0110312344862779));
#20719=CARTESIAN_POINT('Ctrl Pts',(-0.0114146650296267,-0.0306135500857657,
-0.0110790076429274));
#20720=CARTESIAN_POINT('Ctrl Pts',(-0.0114053446397557,-0.0306128453806097,
-0.0110883092512143));
#20721=CARTESIAN_POINT('Ctrl Pts',(-0.0113918281553366,-0.0306118228564228,
-0.0111021483371867));
#20722=CARTESIAN_POINT('Ctrl Pts',(-0.0113875386512043,-0.0306114982707693,
-0.0111065933061866));
#20723=CARTESIAN_POINT('Ctrl Pts',(-0.0113799837698613,-0.0306109266485566,
-0.0111145166748831));
#20724=CARTESIAN_POINT('Ctrl Pts',(-0.011376707656632,-0.0306106787951981,
-0.011117984640405));
#20725=CARTESIAN_POINT('Ctrl Pts',(-0.011369594156811,-0.0306101407404914,
-0.011125585021181));
#20726=CARTESIAN_POINT('Ctrl Pts',(-0.0113657632957425,-0.0306098510289648,
-0.0111297233231859));
#20727=CARTESIAN_POINT('Ctrl Pts',(-0.0113549943971347,-0.030609036449744,
-0.0111414851603933));
#20728=CARTESIAN_POINT('Ctrl Pts',(-0.0113481098222761,-0.0306085154811586,
-0.011149157479398));
#20729=CARTESIAN_POINT('Ctrl Pts',(-0.0112981484961286,-0.0306047283158406,
-0.0112059706575476));
#20730=CARTESIAN_POINT('Ctrl Pts',(-0.0112581510031366,-0.0306016589992643,
-0.011257739948259));
#20731=CARTESIAN_POINT('Ctrl Pts',(-0.0111852487920264,-0.0305956568415225,
-0.0113656172204017));
#20732=CARTESIAN_POINT('Ctrl Pts',(-0.0111523657429364,-0.0305927281169855,
-0.0114215752922551));
#20733=CARTESIAN_POINT('Ctrl Pts',(-0.0110864006852365,-0.0305860048597797,
-0.0115519961374219));
#20734=CARTESIAN_POINT('Ctrl Pts',(-0.0110554970487696,-0.0305821856347508,
-0.0116273370579108));
#20735=CARTESIAN_POINT('Ctrl Pts',(-0.0110256835874023,-0.0305773482220927,
-0.0117203235107662));
#20736=CARTESIAN_POINT('Ctrl Pts',(-0.0110209401514166,-0.0305765306276997,
-0.0117359689842479));
#20737=CARTESIAN_POINT('Ctrl Pts',(-0.0110138205785899,-0.0305752223553117,
-0.0117608702000671));
#20738=CARTESIAN_POINT('Ctrl Pts',(-0.0110112802165783,-0.0305747370980337,
-0.0117700779352432));
#20739=CARTESIAN_POINT('Ctrl Pts',(-0.0110066532492773,-0.0305738170960861,
-0.0117874772711904));
#20740=CARTESIAN_POINT('Ctrl Pts',(-0.0110045481435961,-0.0305733829785686,
-0.0117956636121019));
#20741=CARTESIAN_POINT('Ctrl Pts',(-0.0109999407520886,-0.0305723964077133,
-0.0118142113810097));
#20742=CARTESIAN_POINT('Ctrl Pts',(-0.0109974783760361,-0.0305718426742196,
-0.0118245821991285));
#20743=CARTESIAN_POINT('Ctrl Pts',(-0.0109903127649398,-0.0305701469274038,
-0.0118562164764711));
#20744=CARTESIAN_POINT('Ctrl Pts',(-0.010985952191084,-0.0305689939405844,
-0.0118775541004177));
#20745=CARTESIAN_POINT('Ctrl Pts',(-0.0109653526083149,-0.0305628412630669,
-0.0119904895517208));
#20746=CARTESIAN_POINT('Ctrl Pts',(-0.0109569723504914,-0.0305575944876602,
-0.0120833126911311));
#20747=CARTESIAN_POINT('Ctrl Pts',(-0.0109570310556734,-0.0305462854740702,
-0.0122802823658357));
#20748=CARTESIAN_POINT('Ctrl Pts',(-0.0109675701548483,-0.0305402283780848,
-0.0123839872079394));
#20749=CARTESIAN_POINT('Ctrl Pts',(-0.0109908578235556,-0.0305339559971616,
-0.0124975383991549));
#20750=CARTESIAN_POINT('Ctrl Pts',(-0.0109933910287286,-0.0305333163427565,
-0.0125092012202782));
#20751=CARTESIAN_POINT('Ctrl Pts',(-0.0109974016673079,-0.0305323655343222,
-0.0125266855762637));
#20752=CARTESIAN_POINT('Ctrl Pts',(-0.0109987781345088,-0.0305320491088742,
-0.012532529551301));
#20753=CARTESIAN_POINT('Ctrl Pts',(-0.0110013304375527,-0.0305314800344124,
-0.0125430891227222));
#20754=CARTESIAN_POINT('Ctrl Pts',(-0.0110024945079939,-0.030531226728674,
-0.0125478074780214));
#20755=CARTESIAN_POINT('Ctrl Pts',(-0.0110049464103402,-0.0305307059347612,
-0.0125575477186903));
#20756=CARTESIAN_POINT('Ctrl Pts',(-0.0110062372790875,-0.030530438618633,
-0.0125625686995377));
#20757=CARTESIAN_POINT('Ctrl Pts',(-0.0110096743575761,-0.0305297442262051,
-0.0125756635804875));
#20758=CARTESIAN_POINT('Ctrl Pts',(-0.0110118609023418,-0.0305293194148494,
-0.0125837268252921));
#20759=CARTESIAN_POINT('Ctrl Pts',(-0.0110220196005824,-0.0305274182439488,
-0.0126200191953254));
#20760=CARTESIAN_POINT('Ctrl Pts',(-0.0110307306761535,-0.0305259803376887,
-0.0126480368022343));
#20761=CARTESIAN_POINT('Ctrl Pts',(-0.0110587278539433,-0.0305218284427781,
-0.0127297856134861));
#20762=CARTESIAN_POINT('Ctrl Pts',(-0.0110802026541831,-0.0305191956550781,
-0.0127827162446283));
#20763=CARTESIAN_POINT('Ctrl Pts',(-0.011156662585713,-0.0305109887263886,
-0.0129447475557486));
#20764=CARTESIAN_POINT('Ctrl Pts',(-0.0112216765904696,-0.0305054715992893,
-0.0130485736948259));
#20765=CARTESIAN_POINT('Ctrl Pts',(-0.0113098757997528,-0.0304985580437578,
-0.0131580942112467));
#20766=CARTESIAN_POINT('Ctrl Pts',(-0.0113217654382306,-0.0304976368241939,
-0.0131723251261466));
#20767=CARTESIAN_POINT('Ctrl Pts',(-0.0113411685566166,-0.0304961483394291,
-0.0131947161777586));
#20768=CARTESIAN_POINT('Ctrl Pts',(-0.0113485187203051,-0.0304955877483875,
-0.0132030157661547));
#20769=CARTESIAN_POINT('Ctrl Pts',(-0.0113617395626463,-0.030494584783748,
-0.0132176240987487));
#20770=CARTESIAN_POINT('Ctrl Pts',(-0.0113675748990186,-0.0304941439085291,
-0.0132239642706958));
#20771=CARTESIAN_POINT('Ctrl Pts',(-0.0113798954720892,-0.0304932166438202,
-0.0132371277356155));
#20772=CARTESIAN_POINT('Ctrl Pts',(-0.0113863906442239,-0.0304927298350149,
-0.0132439412076329));
#20773=CARTESIAN_POINT('Ctrl Pts',(-0.0114036429511642,-0.0304914418643615,
-0.0132617105326062));
#20774=CARTESIAN_POINT('Ctrl Pts',(-0.0114145017937085,-0.0304906362758869,
-0.013272565809772));
#20775=CARTESIAN_POINT('Ctrl Pts',(-0.0114688045812437,-0.0304866313182435,
-0.0133252541192191));
#20776=CARTESIAN_POINT('Ctrl Pts',(-0.0115145091375823,-0.0304833304183131,
-0.0133646731809641));
#20777=CARTESIAN_POINT('Ctrl Pts',(-0.0116167928359515,-0.0304761087625533,
-0.0134429305290912));
#20778=CARTESIAN_POINT('Ctrl Pts',(-0.0116738946187512,-0.0304721717299995,
-0.0134808776667595));
#20779=CARTESIAN_POINT('Ctrl Pts',(-0.0117408997875379,-0.0304677368945097,
-0.0135192415635791));
#20780=CARTESIAN_POINT('Ctrl Pts',(-0.0117485116987227,-0.0304672357273039,
-0.0135235144194579));
#20781=CARTESIAN_POINT('Ctrl Pts',(-0.0118208725904811,-0.0304624984088769,
-0.0135633296358874));
#20782=CARTESIAN_POINT('Ctrl Pts',(-0.0118880651098639,-0.0304582975430782,
-0.0135942475560951));
#20783=CARTESIAN_POINT('Ctrl Pts',(-0.0119670189529705,-0.0304537690027713,
-0.0136239174433357));
#20784=CARTESIAN_POINT('Ctrl Pts',(-0.0119768562716497,-0.0304532118153955,
-0.0136275003682332));
#20785=CARTESIAN_POINT('Ctrl Pts',(-0.0119921419429425,-0.0304523577512523,
-0.013632892109869));
#20786=CARTESIAN_POINT('Ctrl Pts',(-0.011997565031341,-0.0304520570108528,
-0.0136347710508932));
#20787=CARTESIAN_POINT('Ctrl Pts',(-0.0120071742131388,-0.0304515282905298,
-0.013638040414886));
#20788=CARTESIAN_POINT('Ctrl Pts',(-0.0120113559134437,-0.0304512996033983,
-0.0136394431919941));
#20789=CARTESIAN_POINT('Ctrl Pts',(-0.0120213711478742,-0.0304507551408711,
-0.0136427551564418));
#20790=CARTESIAN_POINT('Ctrl Pts',(-0.0120272102229729,-0.0304504403265547,
-0.0136446475209974));
#20791=CARTESIAN_POINT('Ctrl Pts',(-0.0120449102584731,-0.0304494935025026,
-0.0136502673730838));
#20792=CARTESIAN_POINT('Ctrl Pts',(-0.0120568053751285,-0.0304488673160112,
-0.0136538864776071));
#20793=CARTESIAN_POINT('Ctrl Pts',(-0.0121432858394292,-0.0304443792744698,
-0.0136790603382886));
#20794=CARTESIAN_POINT('Ctrl Pts',(-0.0122193675082449,-0.0304407732031814,
-0.0136951044785367));
#20795=CARTESIAN_POINT('Ctrl Pts',(-0.0124120221433754,-0.030431815569623,
-0.0137207573530174));
#20796=CARTESIAN_POINT('Ctrl Pts',(-0.0125290679802229,-0.0304265009074883,
-0.013722986690178));
#20797=CARTESIAN_POINT('Ctrl Pts',(-0.0126635106112397,-0.0304198540856339,
-0.0137102749700046));
#20798=CARTESIAN_POINT('Ctrl Pts',(-0.0126817436636776,-0.0304189419127957,
-0.0137082223115352));
#20799=CARTESIAN_POINT('Ctrl Pts',(-0.0127109304055275,-0.0304174625238897,
-0.013704408264347));
#20800=CARTESIAN_POINT('Ctrl Pts',(-0.0127219094838851,-0.030416901647396,
-0.0137028530013345));
#20801=CARTESIAN_POINT('Ctrl Pts',(-0.0127414673467393,-0.0304158943082802,
-0.0136998671138763));
#20802=CARTESIAN_POINT('Ctrl Pts',(-0.0127500526574781,-0.0304154492837221,
-0.013698482029835));
#20803=CARTESIAN_POINT('Ctrl Pts',(-0.0127680735993039,-0.0304145090170615,
-0.0136954181547351));
#20804=CARTESIAN_POINT('Ctrl Pts',(-0.0127775061934778,-0.0304140133054916,
-0.0136937238839203));
#20805=CARTESIAN_POINT('Ctrl Pts',(-0.012802478211279,-0.0304126912727064,
-0.013688997888557));
#20806=CARTESIAN_POINT('Ctrl Pts',(-0.012817987526607,-0.0304118602145704,
-0.0136858147307157));
#20807=CARTESIAN_POINT('Ctrl Pts',(-0.0128976761518482,-0.0304075371738706,
-0.0136681771318004));
#20808=CARTESIAN_POINT('Ctrl Pts',(-0.0129609254904815,-0.0304039236816433,
-0.0136498691678098));
#20809=CARTESIAN_POINT('Ctrl Pts',(-0.0130841263647366,-0.0303965468009369,
-0.0136055011220681));
#20810=CARTESIAN_POINT('Ctrl Pts',(-0.0131439814088435,-0.0303927927114002,
-0.0135795568789032));
#20811=CARTESIAN_POINT('Ctrl Pts',(-0.0132700101696556,-0.0303846516667243,
-0.0135151679245038));
#20812=CARTESIAN_POINT('Ctrl Pts',(-0.0133353395666186,-0.0303802770251158,
-0.0134754258988562));
#20813=CARTESIAN_POINT('Ctrl Pts',(-0.0134080169292813,-0.0303754311130047,
-0.0134234600478813));
#20814=CARTESIAN_POINT('Ctrl Pts',(-0.0134184769205675,-0.0303747343583456,
-0.0134157797127629));
#20815=CARTESIAN_POINT('Ctrl Pts',(-0.0134343989358369,-0.0303736764289402,
-0.0134037767807791));
#20816=CARTESIAN_POINT('Ctrl Pts',(-0.0134399304422851,-0.0303733093944198,
-0.0133995477934748));
#20817=CARTESIAN_POINT('Ctrl Pts',(-0.0134492548124156,-0.0303726918248975,
-0.0133923185282897));
#20818=CARTESIAN_POINT('Ctrl Pts',(-0.0134530624926613,-0.0303724399601715,
-0.0133893376373446));
#20819=CARTESIAN_POINT('Ctrl Pts',(-0.0134607591902259,-0.0303719316240073,
-0.0133832536057947));
#20820=CARTESIAN_POINT('Ctrl Pts',(-0.0134646472362987,-0.0303716752555374,
-0.0133801495389822));
#20821=CARTESIAN_POINT('Ctrl Pts',(-0.0134747992607237,-0.0303710069550637,
-0.0133719638403907));
#20822=CARTESIAN_POINT('Ctrl Pts',(-0.0134810384902817,-0.0303705972902913,
-0.0133668518348593));
#20823=CARTESIAN_POINT('Ctrl Pts',(-0.01351012246613,-0.0303686910913438,
-0.0133426387488838));
#20824=CARTESIAN_POINT('Ctrl Pts',(-0.0135324526332497,-0.0303672375738174,
-0.0133229267366824));
#20825=CARTESIAN_POINT('Ctrl Pts',(-0.0135975102589157,-0.0303629840392982,
-0.0132620568278614));
#20826=CARTESIAN_POINT('Ctrl Pts',(-0.0136384512017853,-0.0303602804252429,
-0.0132190678590793));
#20827=CARTESIAN_POINT('Ctrl Pts',(-0.0137582763463087,-0.0303519015165297,
-0.0130777691031764));
#20828=CARTESIAN_POINT('Ctrl Pts',(-0.0138276604041924,-0.0303462875962367,
-0.0129721114137639));
#20829=CARTESIAN_POINT('Ctrl Pts',(-0.013892501448283,-0.0303391167815595,
-0.0128408404528043));
#20830=CARTESIAN_POINT('Ctrl Pts',(-0.0139012024494203,-0.0303381014887717,
-0.0128223050309537));
#20831=CARTESIAN_POINT('Ctrl Pts',(-0.0139136476553152,-0.030336564344782,
-0.0127943608892424));
#20832=CARTESIAN_POINT('Ctrl Pts',(-0.0139176724491935,-0.0303360527362019,
-0.0127850791625988));
#20833=CARTESIAN_POINT('Ctrl Pts',(-0.0139247363448817,-0.0303351279353409,
-0.0127683397334666));
#20834=CARTESIAN_POINT('Ctrl Pts',(-0.0139278089085867,-0.0303347159744179,
-0.0127608964980392));
#20835=CARTESIAN_POINT('Ctrl Pts',(-0.013934237808598,-0.0303338327932478,
-0.0127449702608046));
#20836=CARTESIAN_POINT('Ctrl Pts',(-0.0139375774448333,-0.030333360992527,
-0.0127364808875621));
#20837=CARTESIAN_POINT('Ctrl Pts',(-0.0139464404684414,-0.030332072580007,
-0.0127133510215719));
#20838=CARTESIAN_POINT('Ctrl Pts',(-0.0139518166402862,-0.0303312507887524,
-0.0126986556020744));
#20839=CARTESIAN_POINT('Ctrl Pts',(-0.013982035736537,-0.0303263844984363,
-0.0126119905761492));
#20840=CARTESIAN_POINT('Ctrl Pts',(-0.0140017446732389,-0.0303221620450477,
-0.0125383528249377));
#20841=CARTESIAN_POINT('Ctrl Pts',(-0.0140339403680866,-0.0303123269729252,
-0.0123687181106948));
#20842=CARTESIAN_POINT('Ctrl Pts',(-0.0140430000000041,-0.0303066610915457,
-0.0122723917483003));
#20843=CARTESIAN_POINT('Ctrl Pts',(-0.014043,-0.0303011972027429,-0.0121758532864921));
#20844=CARTESIAN_POINT('',(-0.0140429998425021,-0.0304166482542229,-0.0121765504512336));
#20845=CARTESIAN_POINT('Ctrl Pts',(-0.014043,-0.0304166107246751,-0.0121758532865585));
#20846=CARTESIAN_POINT('Ctrl Pts',(-0.014043,-0.0304166232329507,-0.0121760856746653));
#20847=CARTESIAN_POINT('Ctrl Pts',(-0.0140429999475007,-0.0304166357427992,
-0.0121763180628743));
#20848=CARTESIAN_POINT('Ctrl Pts',(-0.0140429998425021,-0.0304166482542194,
-0.012176550451168));
#20849=CARTESIAN_POINT('Ctrl Pts',(-0.0140429998425021,-0.0304166482542229,
-0.012176550451233));
#20850=CARTESIAN_POINT('Ctrl Pts',(-0.0140429619592719,-0.0304211623406919,
-0.0122603955171862));
#20851=CARTESIAN_POINT('Ctrl Pts',(-0.0140360912751621,-0.0304258834194363,
-0.0123440778667976));
#20852=CARTESIAN_POINT('Ctrl Pts',(-0.0140055671873961,-0.0304366479657113,
-0.0125292716504272));
#20853=CARTESIAN_POINT('Ctrl Pts',(-0.0139783707368846,-0.0304427144881944,
-0.01262979022047));
#20854=CARTESIAN_POINT('Ctrl Pts',(-0.0139350373405486,-0.0304493427776151,
-0.01274314730646));
#20855=CARTESIAN_POINT('Ctrl Pts',(-0.013928517068393,-0.0304502855523705,
-0.0127593716755159));
#20856=CARTESIAN_POINT('Ctrl Pts',(-0.013919037513126,-0.0304515797528431,
-0.0127818477267646));
#20857=CARTESIAN_POINT('Ctrl Pts',(-0.0139163100750219,-0.0304519439065037,
-0.0127881951030303));
#20858=CARTESIAN_POINT('Ctrl Pts',(-0.0139115804684773,-0.0304525613027739,
-0.0127990013161171));
#20859=CARTESIAN_POINT('Ctrl Pts',(-0.0139095996028356,-0.0304528158130124,
-0.0128034692900178));
#20860=CARTESIAN_POINT('Ctrl Pts',(-0.0139054131184268,-0.0304533452192109,
-0.0128127923736308));
#20861=CARTESIAN_POINT('Ctrl Pts',(-0.0139032035354575,-0.0304536198738844,
-0.0128176455222901));
#20862=CARTESIAN_POINT('Ctrl Pts',(-0.0138972261085774,-0.0304543505385233,
-0.0128305959545962));
#20863=CARTESIAN_POINT('Ctrl Pts',(-0.0138934129969186,-0.0304548038494557,
-0.0128386722566403));
#20864=CARTESIAN_POINT('Ctrl Pts',(-0.0138756599279586,-0.0304568589575214,
-0.0128754434912595));
#20865=CARTESIAN_POINT('Ctrl Pts',(-0.0138609014823846,-0.03045841560221,
-0.0129037365874803));
#20866=CARTESIAN_POINT('Ctrl Pts',(-0.0138010752388869,-0.0304642546108091,
-0.0130102375417289));
#20867=CARTESIAN_POINT('Ctrl Pts',(-0.0137500543379166,-0.0304683129173928,
-0.0130848967692267));
#20868=CARTESIAN_POINT('Ctrl Pts',(-0.0136353052765514,-0.0304766106755115,
-0.0132247310601838));
#20869=CARTESIAN_POINT('Ctrl Pts',(-0.0135717575881666,-0.0304808382146522,
-0.0132895839546813));
#20870=CARTESIAN_POINT('Ctrl Pts',(-0.0134901096780616,-0.0304861580368334,
-0.013359413480513));
#20871=CARTESIAN_POINT('Ctrl Pts',(-0.0134771495972244,-0.0304869989658315,
-0.0133701357255105));
#20872=CARTESIAN_POINT('Ctrl Pts',(-0.0134563982816042,-0.03048834131069,
-0.0133867399609093));
#20873=CARTESIAN_POINT('Ctrl Pts',(-0.0134487218921111,-0.0304888370032319,
-0.0133927637092664));
#20874=CARTESIAN_POINT('Ctrl Pts',(-0.0134341755295528,-0.0304897749274503,
-0.0134039571062186));
#20875=CARTESIAN_POINT('Ctrl Pts',(-0.0134273184563056,-0.0304902164907762,
-0.0134091429477865));
#20876=CARTESIAN_POINT('Ctrl Pts',(-0.013411754241254,-0.0304912176370259,
-0.0134207106034591));
#20877=CARTESIAN_POINT('Ctrl Pts',(-0.0134030228031522,-0.0304917785003676,
-0.0134270588431722));
#20878=CARTESIAN_POINT('Ctrl Pts',(-0.0133769584522568,-0.0304934507747414,
-0.0134455941298333));
#20879=CARTESIAN_POINT('Ctrl Pts',(-0.0133594408169735,-0.0304945721935955,
-0.0134575160183573));
#20880=CARTESIAN_POINT('Ctrl Pts',(-0.0132502144236064,-0.0305015514381697,
-0.0135286053184794));
#20881=CARTESIAN_POINT('Ctrl Pts',(-0.0131526997912829,-0.0305077588498726,
-0.0135782569892975));
#20882=CARTESIAN_POINT('Ctrl Pts',(-0.0129910222943623,-0.0305177073603594,
-0.013640038628511));
#20883=CARTESIAN_POINT('Ctrl Pts',(-0.0129298985789664,-0.0305213891917266,
-0.0136591366264577));
#20884=CARTESIAN_POINT('Ctrl Pts',(-0.012847287824246,-0.0305261329955067,
-0.0136794106303462));
#20885=CARTESIAN_POINT('Ctrl Pts',(-0.0128267101150639,-0.0305272956823491,
-0.0136840157750318));
#20886=CARTESIAN_POINT('Ctrl Pts',(-0.0127914889665945,-0.0305292463789131,
-0.0136911432580558));
#20887=CARTESIAN_POINT('Ctrl Pts',(-0.0127768919384072,-0.0305300434060506,
-0.0136938784515484));
#20888=CARTESIAN_POINT('Ctrl Pts',(-0.0127558266730342,-0.0305311749789225,
-0.0136975116894299));
#20889=CARTESIAN_POINT('Ctrl Pts',(-0.012749389070434,-0.0305315182970713,
-0.0136985800106363));
#20890=CARTESIAN_POINT('Ctrl Pts',(-0.0127381399445833,-0.0305321136299855,
-0.0137003735520935));
#20891=CARTESIAN_POINT('Ctrl Pts',(-0.0127333314647548,-0.0305323666415984,
-0.0137011169041322));
#20892=CARTESIAN_POINT('Ctrl Pts',(-0.0127230120705358,-0.0305329064150909,
-0.0137026622552686));
#20893=CARTESIAN_POINT('Ctrl Pts',(-0.0127175002615166,-0.0305331927844787,
-0.0137034571778443));
#20894=CARTESIAN_POINT('Ctrl Pts',(-0.0127023413139607,-0.0305339753546743,
-0.0137055597180189));
#20895=CARTESIAN_POINT('Ctrl Pts',(-0.0126926857650036,-0.030534468235438,
-0.0137068059242885));
#20896=CARTESIAN_POINT('Ctrl Pts',(-0.0126387997979758,-0.0305371910099088,
-0.0137132429057405));
#20897=CARTESIAN_POINT('Ctrl Pts',(-0.0125943692337139,-0.030539331624267,
-0.0137166087139355));
#20898=CARTESIAN_POINT('Ctrl Pts',(-0.0124687799145164,-0.0305452382153818,
-0.0137206684489272));
#20899=CARTESIAN_POINT('Ctrl Pts',(-0.0123876246663945,-0.0305488914232339,
-0.0137168923349803));
#20900=CARTESIAN_POINT('Ctrl Pts',(-0.0122297503350157,-0.0305562073189009,
-0.0136970036247948));
#20901=CARTESIAN_POINT('Ctrl Pts',(-0.012153216827278,-0.0305598546769151,
-0.0136814007288479));
#20902=CARTESIAN_POINT('Ctrl Pts',(-0.0120580667638414,-0.0305647133371462,
-0.0136543599411083));
#20903=CARTESIAN_POINT('Ctrl Pts',(-0.0120380565943718,-0.0305657533452563,
-0.0136482306668853));
#20904=CARTESIAN_POINT('Ctrl Pts',(-0.0120081160877149,-0.030567339712194,
-0.0136383892327033));
#20905=CARTESIAN_POINT('Ctrl Pts',(-0.0119980888296074,-0.0305678761652763,
-0.0136349784856771));
#20906=CARTESIAN_POINT('Ctrl Pts',(-0.0119800170550744,-0.0305688526900691,
-0.0136286230922377));
#20907=CARTESIAN_POINT('Ctrl Pts',(-0.0119719603870234,-0.0305692915572097,
-0.0136257141538498));
#20908=CARTESIAN_POINT('Ctrl Pts',(-0.0119546782030701,-0.0305702407124572,
-0.0136193110971556));
#20909=CARTESIAN_POINT('Ctrl Pts',(-0.0119454611722413,-0.0305707517144472,
-0.0136157952977533));
#20910=CARTESIAN_POINT('Ctrl Pts',(-0.0119205246041696,-0.0305721475255645,
-0.01360600841255));
#20911=CARTESIAN_POINT('Ctrl Pts',(-0.0119048738205827,-0.0305730380541613,
-0.0135995668176128));
#20912=CARTESIAN_POINT('Ctrl Pts',(-0.0118039981726782,-0.0305788741519992,
-0.0135560941437535));
#20913=CARTESIAN_POINT('Ctrl Pts',(-0.0117221723859712,-0.0305840756719932,
-0.0135116912794723));
#20914=CARTESIAN_POINT('Ctrl Pts',(-0.0115573167984598,-0.0305954138837792,
-0.0134019264622939));
#20915=CARTESIAN_POINT('Ctrl Pts',(-0.0114759716208755,-0.0306015553481338,
-0.0133348504458597));
#20916=CARTESIAN_POINT('Ctrl Pts',(-0.0113893643214617,-0.0306082932068849,
-0.013247144498999));
#20917=CARTESIAN_POINT('Ctrl Pts',(-0.0113768762287884,-0.0306092696785555,
-0.0132340449150845));
#20918=CARTESIAN_POINT('Ctrl Pts',(-0.0113598569604872,-0.0306106035290679,
-0.0132155514845421));
#20919=CARTESIAN_POINT('Ctrl Pts',(-0.0113551283242698,-0.0306109744660327,
-0.0132103422151133));
#20920=CARTESIAN_POINT('Ctrl Pts',(-0.0113471469066024,-0.0306116008613769,
-0.0132014277838151));
#20921=CARTESIAN_POINT('Ctrl Pts',(-0.0113438759740372,-0.0306118576527997,
-0.0131977390646101));
#20922=CARTESIAN_POINT('Ctrl Pts',(-0.011337123927671,-0.0306123878049065,
-0.0131900506803082));
#20923=CARTESIAN_POINT('Ctrl Pts',(-0.0113336456799263,-0.0306126609625325,
-0.0131860486710185));
#20924=CARTESIAN_POINT('Ctrl Pts',(-0.0113244423662386,-0.0306133841199227,
-0.0131753486028728));
#20925=CARTESIAN_POINT('Ctrl Pts',(-0.0113187538491829,-0.0306138315092047,
-0.0131686192085097));
#20926=CARTESIAN_POINT('Ctrl Pts',(-0.0112935203378516,-0.0306158198128638,
-0.0131382445289321));
#20927=CARTESIAN_POINT('Ctrl Pts',(-0.0112746243640372,-0.0306173190145845,
-0.0131140669385898));
#20928=CARTESIAN_POINT('Ctrl Pts',(-0.0112025494906394,-0.030623149254895,
-0.013015950711378));
#20929=CARTESIAN_POINT('Ctrl Pts',(-0.0111552375424365,-0.030627243638966,
-0.0129379278292193));
#20930=CARTESIAN_POINT('Ctrl Pts',(-0.0110749422758685,-0.0306355951768532,
-0.0127744742140938));
#20931=CARTESIAN_POINT('Ctrl Pts',(-0.0110421162633324,-0.0306398394525619,
-0.0126893795270005));
#20932=CARTESIAN_POINT('Ctrl Pts',(-0.0110123478014286,-0.0306451775304189,
-0.0125857579484948));
#20933=CARTESIAN_POINT('Ctrl Pts',(-0.0110079757565,-0.0306460168988562,
-0.012569546726585));
#20934=CARTESIAN_POINT('Ctrl Pts',(-0.0110014893245516,-0.0306473562455791,
-0.012543833483475));
#20935=CARTESIAN_POINT('Ctrl Pts',(-0.0109991987531483,-0.0306478504992553,
-0.0125343770396436));
#20936=CARTESIAN_POINT('Ctrl Pts',(-0.0109950601030574,-0.0306487853506769,
-0.0125165559136453));
#20937=CARTESIAN_POINT('Ctrl Pts',(-0.0109931919416164,-0.030649225278308,
-0.0125081962491017));
#20938=CARTESIAN_POINT('Ctrl Pts',(-0.0109891373545825,-0.0306502221907669,
-0.0124893154617643));
#20939=CARTESIAN_POINT('Ctrl Pts',(-0.0109869910518902,-0.0306507804446034,
-0.012478786255466));
#20940=CARTESIAN_POINT('Ctrl Pts',(-0.0109808300539897,-0.0306524803556776,
-0.0124468616590358));
#20941=CARTESIAN_POINT('Ctrl Pts',(-0.0109771580966731,-0.0306536328500733,
-0.0124254035516808));
#20942=CARTESIAN_POINT('Ctrl Pts',(-0.0109595680137425,-0.0306600116332963,
-0.0123076804651647));
#20943=CARTESIAN_POINT('Ctrl Pts',(-0.0109543241034389,-0.0306655090689206,
-0.0122103547704631));
#20944=CARTESIAN_POINT('Ctrl Pts',(-0.0109612556957566,-0.0306753151036192,
-0.0120397967497272));
#20945=CARTESIAN_POINT('Ctrl Pts',(-0.010969476643053,-0.0306795673559181,
-0.0119667019448935));
#20946=CARTESIAN_POINT('Ctrl Pts',(-0.010987018548352,-0.0306849504049318,
-0.0118721219714775));
#20947=CARTESIAN_POINT('Ctrl Pts',(-0.0109916568000309,-0.0306862077229858,
-0.0118498679125829));
#20948=CARTESIAN_POINT('Ctrl Pts',(-0.0110003256509675,-0.0306882978728411,
-0.0118124360475416));
#20949=CARTESIAN_POINT('Ctrl Pts',(-0.0110040992278845,-0.0306891414710078,
-0.0117972028407568));
#20950=CARTESIAN_POINT('Ctrl Pts',(-0.0110098017706814,-0.0306903251657888,
-0.0117756003048406));
#20951=CARTESIAN_POINT('Ctrl Pts',(-0.0110115404366519,-0.0306906752394195,
-0.0117691822358206));
#20952=CARTESIAN_POINT('Ctrl Pts',(-0.0110146232150849,-0.0306912773937334,
-0.0117580872233235));
#20953=CARTESIAN_POINT('Ctrl Pts',(-0.0110159480480263,-0.0306915305617535,
-0.0117534050850856));
#20954=CARTESIAN_POINT('Ctrl Pts',(-0.0110188097995528,-0.0306920656357347,
-0.0117434708938957));
#20955=CARTESIAN_POINT('Ctrl Pts',(-0.0110203525251162,-0.0306923472066169,
-0.0117382206834991));
#20956=CARTESIAN_POINT('Ctrl Pts',(-0.011024670551673,-0.0306931170189241,
-0.0117238094362247));
#20957=CARTESIAN_POINT('Ctrl Pts',(-0.0110275032615779,-0.0306936020335336,
-0.0117146657022878));
#20958=CARTESIAN_POINT('Ctrl Pts',(-0.0110426153138818,-0.0306960918336743,
-0.011667444483677));
#20959=CARTESIAN_POINT('Ctrl Pts',(-0.0110562879786035,-0.0306980248142775,
-0.0116298260922532));
#20960=CARTESIAN_POINT('Ctrl Pts',(-0.0111033029854586,-0.0307039044634106,
-0.0115146344757925));
#20961=CARTESIAN_POINT('Ctrl Pts',(-0.0111415567760878,-0.0307077024841035,
-0.0114392352185974));
#20962=CARTESIAN_POINT('Ctrl Pts',(-0.0112274929545942,-0.0307152357200265,
-0.0112995485770479));
#20963=CARTESIAN_POINT('Ctrl Pts',(-0.0112743787907372,-0.0307189517511015,
-0.0112350902162897));
#20964=CARTESIAN_POINT('Ctrl Pts',(-0.0113397333074098,-0.030723896382847,
-0.0111584661777838));
#20965=CARTESIAN_POINT('Ctrl Pts',(-0.0113537713148073,-0.0307249460144424,
-0.0111426761119587));
#20966=CARTESIAN_POINT('Ctrl Pts',(-0.0113753531124075,-0.0307265441084047,
-0.0111193820975619));
#20967=CARTESIAN_POINT('Ctrl Pts',(-0.0113826578108055,-0.0307270824316285,
-0.0111116594978831));
#20968=CARTESIAN_POINT('Ctrl Pts',(-0.0113959929561588,-0.0307280608851821,
-0.0110978501101519));
#20969=CARTESIAN_POINT('Ctrl Pts',(-0.0114019954527315,-0.0307284997866218,
-0.0110917368668703));
#20970=CARTESIAN_POINT('Ctrl Pts',(-0.0114149967993361,-0.030729447352476,
-0.0110787143845922));
#20971=CARTESIAN_POINT('Ctrl Pts',(-0.0114220113940059,-0.0307299567116823,
-0.0110718214595818));
#20972=CARTESIAN_POINT('Ctrl Pts',(-0.0114411804004771,-0.0307313438491194,
-0.0110533418049822));
#20973=CARTESIAN_POINT('Ctrl Pts',(-0.0114534586045064,-0.0307322272300015,
-0.0110418858937261));
#20974=CARTESIAN_POINT('Ctrl Pts',(-0.0115348687414218,-0.0307380531965798,
-0.0109683764485705));
#20975=CARTESIAN_POINT('Ctrl Pts',(-0.0116092877460205,-0.0307432517697466,
-0.0109124824317057));
#20976=CARTESIAN_POINT('Ctrl Pts',(-0.0117777427553323,-0.0307545884299237,
-0.0108082780066903));
#20977=CARTESIAN_POINT('Ctrl Pts',(-0.0118726434709606,-0.0307607315589126,
-0.010762225704277));
#20978=CARTESIAN_POINT('Ctrl Pts',(-0.0119883950716518,-0.030767464384224,
-0.0107200260264546));
#20979=CARTESIAN_POINT('Ctrl Pts',(-0.0120054033895746,-0.0307684348701076,
-0.0107141601375789));
#20980=CARTESIAN_POINT('Ctrl Pts',(-0.0120291885079166,-0.0307697621975758,
-0.0107064197736644));
#20981=CARTESIAN_POINT('Ctrl Pts',(-0.012035880805606,-0.0307701324089196,
-0.0107042923170377));
#20982=CARTESIAN_POINT('Ctrl Pts',(-0.0120472965931817,-0.0307707581089296,
-0.0107007489047131));
#20983=CARTESIAN_POINT('Ctrl Pts',(-0.0120520127416988,-0.0307710149191941,
-0.0106993097786609));
#20984=CARTESIAN_POINT('Ctrl Pts',(-0.0120618273026738,-0.0307715457612612,
-0.0106963662328868));
#20985=CARTESIAN_POINT('Ctrl Pts',(-0.0120669266884168,-0.030771819583202,
-0.010694865520531));
#20986=CARTESIAN_POINT('Ctrl Pts',(-0.0120805421215145,-0.0307725456422034,
-0.0106909349343394));
#20987=CARTESIAN_POINT('Ctrl Pts',(-0.0120890716209946,-0.0307729952389376,
-0.0106885519388215));
#20988=CARTESIAN_POINT('Ctrl Pts',(-0.0121276388578793,-0.0307750064555578,
-0.0106781340281651));
#20989=CARTESIAN_POINT('Ctrl Pts',(-0.0121578964739101,-0.0307765252451901,
-0.0106709342820215));
#20990=CARTESIAN_POINT('Ctrl Pts',(-0.012277221589053,-0.0307823564303481,
-0.0106463264540505));
#20991=CARTESIAN_POINT('Ctrl Pts',(-0.0123675392354059,-0.0307864369814528,
-0.0106358731519739));
#20992=CARTESIAN_POINT('Ctrl Pts',(-0.0125490537754813,-0.0307947659468167,
-0.0106309607689021));
#20993=CARTESIAN_POINT('Ctrl Pts',(-0.0126398834516143,-0.0307990017912982,
-0.0106365256891552));
#20994=CARTESIAN_POINT('Ctrl Pts',(-0.0127462966141307,-0.0308043302083165,
-0.0106525447049422));
#20995=CARTESIAN_POINT('Ctrl Pts',(-0.0127628616879551,-0.030805169853775,
-0.0106553156309625));
#20996=CARTESIAN_POINT('Ctrl Pts',(-0.0127889539324155,-0.0308065098558042,
-0.0106601193274885));
#20997=CARTESIAN_POINT('Ctrl Pts',(-0.0127985129744181,-0.0308070044923971,
-0.0106619729054995));
#20998=CARTESIAN_POINT('Ctrl Pts',(-0.0128164560618017,-0.0308079402117008,
-0.0106656287696141));
#20999=CARTESIAN_POINT('Ctrl Pts',(-0.0128248438973218,-0.0308083806253845,
-0.0106674107225067));
#21000=CARTESIAN_POINT('Ctrl Pts',(-0.0128437235527055,-0.0308093788468724,
-0.0106715863815443));
#21001=CARTESIAN_POINT('Ctrl Pts',(-0.0128542059869155,-0.0308099379277745,
-0.0106740201023731));
#21002=CARTESIAN_POINT('Ctrl Pts',(-0.0128851609110074,-0.03081160359428,
-0.0106815490540761));
#21003=CARTESIAN_POINT('Ctrl Pts',(-0.0129055547445077,-0.0308127201236252,
-0.0106869545807193));
#21004=CARTESIAN_POINT('Ctrl Pts',(-0.0130325293218204,-0.0308197945049652,
-0.0107234123468547));
#21005=CARTESIAN_POINT('Ctrl Pts',(-0.0131355953217276,-0.0308261170557336,
-0.0107654690165223));
#21006=CARTESIAN_POINT('Ctrl Pts',(-0.0132890159889861,-0.0308361480421952,
-0.0108483289663659));
#21007=CARTESIAN_POINT('Ctrl Pts',(-0.0133428826814456,-0.0308397973145065,
-0.0108818608243822));
#21008=CARTESIAN_POINT('Ctrl Pts',(-0.0134116219889735,-0.0308445030601893,
-0.0109307693202668));
#21009=CARTESIAN_POINT('Ctrl Pts',(-0.0134284593864447,-0.0308456596245896,
-0.0109432738882543));
#21010=CARTESIAN_POINT('Ctrl Pts',(-0.0134567215558228,-0.0308476006057915,
-0.0109651711068409));
#21011=CARTESIAN_POINT('Ctrl Pts',(-0.0134682755582404,-0.0308483939966565,
-0.0109743916972974));
#21012=CARTESIAN_POINT('Ctrl Pts',(-0.0134847150887634,-0.0308495204899492,
-0.010987902359445));
#21013=CARTESIAN_POINT('Ctrl Pts',(-0.0134897084787755,-0.0308498623307743,
-0.0109920592414255));
#21014=CARTESIAN_POINT('Ctrl Pts',(-0.0134983819025579,-0.0308504553007776,
-0.0109993729079864));
#21015=CARTESIAN_POINT('Ctrl Pts',(-0.013502073536278,-0.0308507074190815,
-0.0110025156818494));
#21016=CARTESIAN_POINT('Ctrl Pts',(-0.0135099648380958,-0.0308512457214186,
-0.0110092981410806));
#21017=CARTESIAN_POINT('Ctrl Pts',(-0.0135141597046751,-0.0308515315098546,
-0.0110129431537756));
#21018=CARTESIAN_POINT('Ctrl Pts',(-0.0135256275228104,-0.0308523120799809,
-0.0110230170417338));
#21019=CARTESIAN_POINT('Ctrl Pts',(-0.0135328597583993,-0.0308528035570709,
-0.0110294921080602));
#21020=CARTESIAN_POINT('Ctrl Pts',(-0.013572648899753,-0.0308555061701469,
-0.0110657978330293));
#21021=CARTESIAN_POINT('Ctrl Pts',(-0.013603977222896,-0.0308576293819689,
-0.0110969493681308));
#21022=CARTESIAN_POINT('Ctrl Pts',(-0.0136891656692589,-0.0308635356374126,
-0.0111892592360783));
#21023=CARTESIAN_POINT('Ctrl Pts',(-0.0137395790253832,-0.0308672026279364,
-0.0112533958816029));
#21024=CARTESIAN_POINT('Ctrl Pts',(-0.013828008975108,-0.0308745408381592,
-0.0113863239956194));
#21025=CARTESIAN_POINT('Ctrl Pts',(-0.0138663073724793,-0.0308781963844657,
-0.0114546272955443));
#21026=CARTESIAN_POINT('Ctrl Pts',(-0.0139080908935563,-0.0308830653584843,
-0.011544530967795));
#21027=CARTESIAN_POINT('Ctrl Pts',(-0.0139165318193202,-0.0308841063692228,
-0.0115637051127779));
#21028=CARTESIAN_POINT('Ctrl Pts',(-0.0139286487403395,-0.0308856937539192,
-0.0115928233061177));
#21029=CARTESIAN_POINT('Ctrl Pts',(-0.0139326170781135,-0.0308862301864663,
-0.0116026434806445));
#21030=CARTESIAN_POINT('Ctrl Pts',(-0.0139396093889504,-0.0308872064059661,
-0.0116204731555862));
#21031=CARTESIAN_POINT('Ctrl Pts',(-0.0139426684200045,-0.0308876449847313,
-0.0116284684962802));
#21032=CARTESIAN_POINT('Ctrl Pts',(-0.0139491048155499,-0.0308885932070914,
-0.0116457199913139));
#21033=CARTESIAN_POINT('Ctrl Pts',(-0.0139524603565234,-0.0308891035605338,
-0.0116549838366586));
#21034=CARTESIAN_POINT('Ctrl Pts',(-0.0139613261152707,-0.0308904968068033,
-0.0116802120876568));
#21035=CARTESIAN_POINT('Ctrl Pts',(-0.0139666632167006,-0.0308913853925636,
-0.0116962355311076));
#21036=CARTESIAN_POINT('Ctrl Pts',(-0.0140000051271375,-0.03089728200354,
-0.0118021026232651));
#21037=CARTESIAN_POINT('Ctrl Pts',(-0.0140199994568309,-0.0309025532529568,
-0.0118942471776128));
#21038=CARTESIAN_POINT('Ctrl Pts',(-0.0140391534379602,-0.0309115449730766,
-0.0120500901012688));
#21039=CARTESIAN_POINT('Ctrl Pts',(-0.0140430000007467,-0.0309151869899036,
-0.0121129498483668));
#21040=CARTESIAN_POINT('Ctrl Pts',(-0.014043,-0.0309187674097093,-0.0121758533048748));
#21041=CARTESIAN_POINT('Origin',(-0.0125,-0.0375520664398416,-0.0121758532865581));
#21042=CARTESIAN_POINT('',(-0.014043,-0.0314187998068562,-0.0121758533148101));
#21043=CARTESIAN_POINT('',(-0.014043,-0.0313028240247934,-0.012175853286558));
#21044=CARTESIAN_POINT('',(-0.014043,-0.0375520664398416,-0.012175853286558));
#21045=CARTESIAN_POINT('Ctrl Pts',(-0.014043,-0.0313028240247934,-0.012175853286558));
#21046=CARTESIAN_POINT('Ctrl Pts',(-0.014043,-0.0313005190170936,-0.0121265275259863));
#21047=CARTESIAN_POINT('Ctrl Pts',(-0.0140406347849488,-0.0312981692539751,
-0.0120772051756399));
#21048=CARTESIAN_POINT('Ctrl Pts',(-0.0140338217440674,-0.0312946809599502,
-0.0120064041507614));
#21049=CARTESIAN_POINT('Ctrl Pts',(-0.0140312806644925,-0.0312936011312428,
-0.0119847993155959));
#21050=CARTESIAN_POINT('Ctrl Pts',(-0.0140268066319898,-0.0312919676677619,
-0.0119526371310362));
#21051=CARTESIAN_POINT('Ctrl Pts',(-0.0140252188406569,-0.031291424927535,
-0.0119420340740226));
#21052=CARTESIAN_POINT('Ctrl Pts',(-0.0140221682962787,-0.0312904436278096,
-0.0119230182053871));
#21053=CARTESIAN_POINT('Ctrl Pts',(-0.0140207459527931,-0.0312900063722433,
-0.0119145993035507));
#21054=CARTESIAN_POINT('Ctrl Pts',(-0.0140175605185017,-0.0312890681217481,
-0.0118966527277991));
#21055=CARTESIAN_POINT('Ctrl Pts',(-0.0140157774145337,-0.0312885665028,
-0.0118871290181793));
#21056=CARTESIAN_POINT('Ctrl Pts',(-0.0140106781529482,-0.0312871927391396,
-0.0118612436754009));
#21057=CARTESIAN_POINT('Ctrl Pts',(-0.0140071860355736,-0.0312863149998045,
-0.0118449183778706));
#21058=CARTESIAN_POINT('Ctrl Pts',(-0.0139834471966939,-0.0312807148054992,
-0.0117421255008378));
#21059=CARTESIAN_POINT('Ctrl Pts',(-0.0139560348964219,-0.0312757595954976,
-0.0116574964101312));
#21060=CARTESIAN_POINT('Ctrl Pts',(-0.0138875438819905,-0.0312656985551237,
-0.0114952698372967));
#21061=CARTESIAN_POINT('Ctrl Pts',(-0.0138468197716936,-0.0312606167738904,
-0.0114178634818881));
#21062=CARTESIAN_POINT('Ctrl Pts',(-0.0137803875331701,-0.0312536983617118,
-0.0113140238327408));
#21063=CARTESIAN_POINT('Ctrl Pts',(-0.0137599529244731,-0.031251714526073,
-0.0112844155522293));
#21064=CARTESIAN_POINT('Ctrl Pts',(-0.0137329721680036,-0.0312492939318396,
-0.0112481062528848));
#21065=CARTESIAN_POINT('Ctrl Pts',(-0.0137273763371305,-0.0312488019098052,
-0.0112407157240016));
#21066=CARTESIAN_POINT('Ctrl Pts',(-0.0137184210559769,-0.0312480307572239,
-0.0112291071766932));
#21067=CARTESIAN_POINT('Ctrl Pts',(-0.0137151056003922,-0.0312477486939512,
-0.0112248556799171));
#21068=CARTESIAN_POINT('Ctrl Pts',(-0.0137087556794671,-0.0312472151110408,
-0.0112168004298651));
#21069=CARTESIAN_POINT('Ctrl Pts',(-0.0137057254418329,-0.0312469633209034,
-0.0112129935700234));
#21070=CARTESIAN_POINT('Ctrl Pts',(-0.0136984538037513,-0.0312463657082569,
-0.011203946434757));
#21071=CARTESIAN_POINT('Ctrl Pts',(-0.0136941959271362,-0.0312460210537556,
-0.0111987194476353));
#21072=CARTESIAN_POINT('Ctrl Pts',(-0.0136795084245081,-0.0312448494325104,
-0.0111809284147174));
#21073=CARTESIAN_POINT('Ctrl Pts',(-0.0136689133758189,-0.0312440336178028,
-0.011168501717371));
#21074=CARTESIAN_POINT('Ctrl Pts',(-0.0136422593199032,-0.0312420458234462,
-0.0111382266894987));
#21075=CARTESIAN_POINT('Ctrl Pts',(-0.0136259769468366,-0.0312408869670091,
-0.0111205801846117));
#21076=CARTESIAN_POINT('Ctrl Pts',(-0.0135524081518246,-0.0312358524697818,
-0.0110444901932278));
#21077=CARTESIAN_POINT('Ctrl Pts',(-0.0134909347650257,-0.0312321580340759,
-0.0109902753235302));
#21078=CARTESIAN_POINT('Ctrl Pts',(-0.0133559939598241,-0.0312244326390659,
-0.010889129713864));
#21079=CARTESIAN_POINT('Ctrl Pts',(-0.0132822749709674,-0.0312204048739834,
-0.01084302651057));
#21080=CARTESIAN_POINT('Ctrl Pts',(-0.0131858139626322,-0.0312150855436296,
-0.0107934722996522));
#21081=CARTESIAN_POINT('Ctrl Pts',(-0.0131663455494081,-0.0312140103464438,
-0.0107839834884451));
#21082=CARTESIAN_POINT('Ctrl Pts',(-0.0131369669927512,-0.0312123825279386,
-0.0107704221782014));
#21083=CARTESIAN_POINT('Ctrl Pts',(-0.01312720327993,-0.0312118406869284,
-0.0107660378417762));
#21084=CARTESIAN_POINT('Ctrl Pts',(-0.0131095713611014,-0.0312108603544565,
-0.0107583397483868));
#21085=CARTESIAN_POINT('Ctrl Pts',(-0.0131017197167644,-0.0312104231556606,
-0.0107549890236042));
#21086=CARTESIAN_POINT('Ctrl Pts',(-0.0130848864820876,-0.0312094843018567,
-0.0107479699147983));
#21087=CARTESIAN_POINT('Ctrl Pts',(-0.0130758973173038,-0.0312089820147118,
-0.0107443207530781));
#21088=CARTESIAN_POINT('Ctrl Pts',(-0.0130512943288748,-0.0312076045266062,
-0.0107346023788394));
#21089=CARTESIAN_POINT('Ctrl Pts',(-0.0130356154374764,-0.031206723680201,
-0.0107287023997226));
#21090=CARTESIAN_POINT('Ctrl Pts',(-0.0129342466001967,-0.031201007907147,
-0.0106924302429863));
#21091=CARTESIAN_POINT('Ctrl Pts',(-0.0128461220448033,-0.031195928251443,
-0.0106694305730379));
#21092=CARTESIAN_POINT('Ctrl Pts',(-0.0126669335673251,-0.0311855366367846,
-0.0106392232659509));
#21093=CARTESIAN_POINT('Ctrl Pts',(-0.0125762113815732,-0.0311802471659527,
-0.0106320622022023));
#21094=CARTESIAN_POINT('Ctrl Pts',(-0.0124543255623496,-0.0311734452865964,
-0.0106332166961741));
#21095=CARTESIAN_POINT('Ctrl Pts',(-0.0124232795539096,-0.0311717406208604,
-0.0106344487245602));
#21096=CARTESIAN_POINT('Ctrl Pts',(-0.0123834825228855,-0.0311696089553695,
-0.0106372335706211));
#21097=CARTESIAN_POINT('Ctrl Pts',(-0.0123746802217776,-0.0311691408530085,
-0.0106379254881434));
#21098=CARTESIAN_POINT('Ctrl Pts',(-0.0123606093942982,-0.0311683985144417,
-0.0106391531551615));
#21099=CARTESIAN_POINT('Ctrl Pts',(-0.0123553369690545,-0.0311681216923717,
-0.010639640526576));
#21100=CARTESIAN_POINT('Ctrl Pts',(-0.0123451854952486,-0.0311675914182987,
-0.0106406316328125));
#21101=CARTESIAN_POINT('Ctrl Pts',(-0.0123403062233601,-0.0311673377695546,
-0.0106411315023298));
#21102=CARTESIAN_POINT('Ctrl Pts',(-0.0123284948285749,-0.0311667265721093,
-0.0106423984885686));
#21103=CARTESIAN_POINT('Ctrl Pts',(-0.0123215652740173,-0.0311663703395413,
-0.010643189365978));
#21104=CARTESIAN_POINT('Ctrl Pts',(-0.0122969636725558,-0.0311651132311436,
-0.0106461662858608));
#21105=CARTESIAN_POINT('Ctrl Pts',(-0.0122793237856051,-0.0311642258140123,
-0.0106486112855031));
#21106=CARTESIAN_POINT('Ctrl Pts',(-0.0121583326540826,-0.0311582114863341,
-0.0106675215962063));
#21107=CARTESIAN_POINT('Ctrl Pts',(-0.0120568375989976,-0.031153516538237,
-0.0106941607960075));
#21108=CARTESIAN_POINT('Ctrl Pts',(-0.011870697009067,-0.0311444087027044,
-0.0107638758042902));
#21109=CARTESIAN_POINT('Ctrl Pts',(-0.0117857906274547,-0.0311400321842557,
-0.0108048663533));
#21110=CARTESIAN_POINT('Ctrl Pts',(-0.0116908961306411,-0.0311345506455391,
-0.0108618987205334));
#21111=CARTESIAN_POINT('Ctrl Pts',(-0.0116767792295656,-0.0311337192033832,
-0.0108706968939959));
#21112=CARTESIAN_POINT('Ctrl Pts',(-0.0116545998468666,-0.0311323859911732,
-0.0108850229120981));
#21113=CARTESIAN_POINT('Ctrl Pts',(-0.0116464427123398,-0.0311318897542957,
-0.0108904022274014));
#21114=CARTESIAN_POINT('Ctrl Pts',(-0.0116312619504509,-0.0311309548612989,
-0.0109006215631267));
#21115=CARTESIAN_POINT('Ctrl Pts',(-0.0116242262729878,-0.0311305169182789,
-0.0109054430684162));
#21116=CARTESIAN_POINT('Ctrl Pts',(-0.0116085343097703,-0.0311295294932626,
-0.0109163889730781));
#21117=CARTESIAN_POINT('Ctrl Pts',(-0.0115999005113475,-0.0311289788167575,
-0.0109225447304792));
#21118=CARTESIAN_POINT('Ctrl Pts',(-0.0115742441204289,-0.0311273198262368,
-0.0109412391678987));
#21119=CARTESIAN_POINT('Ctrl Pts',(-0.0115574155588669,-0.0311262014037959,
-0.0109540388644997));
#21120=CARTESIAN_POINT('Ctrl Pts',(-0.0114781619539282,-0.0311207854773813,
-0.0110169306531468));
#21121=CARTESIAN_POINT('Ctrl Pts',(-0.0114194415795425,-0.0311163109085506,
-0.0110714777212019));
#21122=CARTESIAN_POINT('Ctrl Pts',(-0.0113074279156442,-0.031106870717989,
-0.0111930533605935));
#21123=CARTESIAN_POINT('Ctrl Pts',(-0.0112549350824193,-0.031101908248443,
-0.0112604641424284));
#21124=CARTESIAN_POINT('Ctrl Pts',(-0.0111870507173682,-0.0310949224586195,
-0.0113643609691927));
#21125=CARTESIAN_POINT('Ctrl Pts',(-0.0111670518366827,-0.0310927752266633,
-0.0113976468630364));
#21126=CARTESIAN_POINT('Ctrl Pts',(-0.0111437602459878,-0.0310901894747661,
-0.011439950822192));
#21127=CARTESIAN_POINT('Ctrl Pts',(-0.0111392685022474,-0.0310896864884867,
-0.0114482898822647));
#21128=CARTESIAN_POINT('Ctrl Pts',(-0.0111323202740601,-0.0310889021407934,
-0.0114614789367094));
#21129=CARTESIAN_POINT('Ctrl Pts',(-0.0111298122170721,-0.0310886176822952,
-0.0114663013252655));
#21130=CARTESIAN_POINT('Ctrl Pts',(-0.0111251139595864,-0.0310880824073191,
-0.011475452750135));
#21131=CARTESIAN_POINT('Ctrl Pts',(-0.0111229186460618,-0.0310878312878547,
-0.0114797789511274));
#21132=CARTESIAN_POINT('Ctrl Pts',(-0.0111177632486421,-0.031087239042276,
-0.0114900583000764));
#21133=CARTESIAN_POINT('Ctrl Pts',(-0.0111148211425578,-0.0310868990256422,
-0.0114960204127502));
#21134=CARTESIAN_POINT('Ctrl Pts',(-0.0111050326269539,-0.031085760227282,
-0.0115161839940852));
#21135=CARTESIAN_POINT('Ctrl Pts',(-0.0110983651551519,-0.0310849717737282,
-0.0115304717364148));
#21136=CARTESIAN_POINT('Ctrl Pts',(-0.0110825561425577,-0.0310830640951102,
-0.0115657500526432));
#21137=CARTESIAN_POINT('Ctrl Pts',(-0.011073660356683,-0.0310819566575063,
-0.0115868470458324));
#21138=CARTESIAN_POINT('Ctrl Pts',(-0.0110377984019296,-0.0310773091971512,
-0.0116774789781477));
#21139=CARTESIAN_POINT('Ctrl Pts',(-0.0110154216321738,-0.03107392375148,
-0.0117487247801976));
#21140=CARTESIAN_POINT('Ctrl Pts',(-0.01097626581616,-0.0310661315592871,
-0.0119145757500195));
#21141=CARTESIAN_POINT('Ctrl Pts',(-0.0109629844860348,-0.0310617159960887,
-0.0120096817091262));
#21142=CARTESIAN_POINT('Ctrl Pts',(-0.0109576162560431,-0.0310559503038506,
-0.0121271249687789));
#21143=CARTESIAN_POINT('Ctrl Pts',(-0.0109570826618411,-0.0310548705814258,
-0.0121488701201978));
#21144=CARTESIAN_POINT('Ctrl Pts',(-0.0109569725114194,-0.0310532372833294,
-0.0121813386347357));
#21145=CARTESIAN_POINT('Ctrl Pts',(-0.0109570478613904,-0.0310526946015177,
-0.0121920585324064));
#21146=CARTESIAN_POINT('Ctrl Pts',(-0.0109573838690453,-0.0310517134114333,
-0.0122113125077997));
#21147=CARTESIAN_POINT('Ctrl Pts',(-0.0109576036693031,-0.031051276207012,
-0.012219846911247));
#21148=CARTESIAN_POINT('Ctrl Pts',(-0.0109582240675939,-0.0310503380719188,
-0.0122380612446153));
#21149=CARTESIAN_POINT('Ctrl Pts',(-0.0109586450312573,-0.0310498365173575,
-0.0122477400750566));
#21150=CARTESIAN_POINT('Ctrl Pts',(-0.0109600393977087,-0.0310484629485315,
-0.0122740823602664));
#21151=CARTESIAN_POINT('Ctrl Pts',(-0.0109611920708989,-0.0310475853407344,
-0.0122907346830704));
#21152=CARTESIAN_POINT('Ctrl Pts',(-0.0109701797365539,-0.031041987693695,
-0.012395801729819));
#21153=CARTESIAN_POINT('Ctrl Pts',(-0.0109853604041931,-0.031037035122964,
-0.0124834087278465));
#21154=CARTESIAN_POINT('Ctrl Pts',(-0.0110302204661157,-0.0310269812824074,
-0.0126535625986533));
#21155=CARTESIAN_POINT('Ctrl Pts',(-0.0110595705451287,-0.0310219041063863,
-0.0127358722422504));
#21156=CARTESIAN_POINT('Ctrl Pts',(-0.0111106681819876,-0.0310149827822227,
-0.0128480940182276));
#21157=CARTESIAN_POINT('Ctrl Pts',(-0.0111267659440434,-0.0310129923785422,
-0.0128803950497096));
#21158=CARTESIAN_POINT('Ctrl Pts',(-0.0111484092874477,-0.031010565137391,
-0.0129202574921695));
#21159=CARTESIAN_POINT('Ctrl Pts',(-0.011152909743729,-0.0310100726732616,
-0.0129283710108423));
#21160=CARTESIAN_POINT('Ctrl Pts',(-0.011160141437612,-0.0310093010078231,
-0.0129411356619324));
#21161=CARTESIAN_POINT('Ctrl Pts',(-0.0111628242807973,-0.0310090188667659,
-0.0129458137913819));
#21162=CARTESIAN_POINT('Ctrl Pts',(-0.0111679737966436,-0.0310084852567781,
-0.0129546850130064));
#21163=CARTESIAN_POINT('Ctrl Pts',(-0.0111704358242123,-0.0310082335159733,
-0.0129588805959455));
#21164=CARTESIAN_POINT('Ctrl Pts',(-0.0111763546002404,-0.0310076361981139,
-0.0129688584808408));
#21165=CARTESIAN_POINT('Ctrl Pts',(-0.011179829488834,-0.031007291786187,
-0.0129746299807336));
#21166=CARTESIAN_POINT('Ctrl Pts',(-0.0111918409033299,-0.0310061218476698,
-0.0129942874388786));
#21167=CARTESIAN_POINT('Ctrl Pts',(-0.0112005598606468,-0.0310053074309449,
-0.0130080612220807));
#21168=CARTESIAN_POINT('Ctrl Pts',(-0.0112226240601629,-0.0310033237572431,
-0.0130417246730382));
#21169=CARTESIAN_POINT('Ctrl Pts',(-0.0112362174672482,-0.0310021675538656,
-0.0130614470730105));
#21170=CARTESIAN_POINT('Ctrl Pts',(-0.0112980277246355,-0.0309971540684869,
-0.0131468029614563));
#21171=CARTESIAN_POINT('Ctrl Pts',(-0.0113509394552251,-0.0309934765240861,
-0.0132088789021195));
#21172=CARTESIAN_POINT('Ctrl Pts',(-0.0114758488817147,-0.0309853823298892,
-0.0133338864009991));
#21173=CARTESIAN_POINT('Ctrl Pts',(-0.0115492838821746,-0.0309809558937707,
-0.0133948949450062));
#21174=CARTESIAN_POINT('Ctrl Pts',(-0.0116416731843121,-0.0309754121445663,
-0.0134581964913626));
#21175=CARTESIAN_POINT('Ctrl Pts',(-0.0116556301136451,-0.0309745758274465,
-0.0134674292560259));
#21176=CARTESIAN_POINT('Ctrl Pts',(-0.011677988908923,-0.0309732365604675,
-0.013481702695055));
#21177=CARTESIAN_POINT('Ctrl Pts',(-0.0116862935610924,-0.0309727392322758,
-0.0134868936127972));
#21178=CARTESIAN_POINT('Ctrl Pts',(-0.0117019200456593,-0.0309718033949768,
-0.0134964554562701));
#21179=CARTESIAN_POINT('Ctrl Pts',(-0.0117092298122922,-0.0309713656136902,
-0.0135008454414439));
#21180=CARTESIAN_POINT('Ctrl Pts',(-0.0117256832486443,-0.0309703800294736,
-0.0135105421382006));
#21181=CARTESIAN_POINT('Ctrl Pts',(-0.0117348457680845,-0.0309698310511575,
-0.0135158158815605));
#21182=CARTESIAN_POINT('Ctrl Pts',(-0.0117623517470979,-0.0309681823257206,
-0.0135312736031221));
#21183=CARTESIAN_POINT('Ctrl Pts',(-0.0117808489710853,-0.0309670726544111,
-0.0135411777602971));
#21184=CARTESIAN_POINT('Ctrl Pts',(-0.0118696968007565,-0.030961736442912,
-0.0135864439912578));
#21185=CARTESIAN_POINT('Ctrl Pts',(-0.0119424760997342,-0.0309573388393052,
-0.0136167601913685));
#21186=CARTESIAN_POINT('Ctrl Pts',(-0.0120956776001367,-0.0309481341353171,
-0.0136672258043267));
#21187=CARTESIAN_POINT('Ctrl Pts',(-0.0121760589441339,-0.0309433324564841,
-0.0136867241320808));
#21188=CARTESIAN_POINT('Ctrl Pts',(-0.0122997019858036,-0.0309362604012892,
-0.0137063910731471));
#21189=CARTESIAN_POINT('Ctrl Pts',(-0.0123420526491352,-0.0309338943701879,
-0.0137113396619697));
#21190=CARTESIAN_POINT('Ctrl Pts',(-0.0123941313120377,-0.030931095948976,
-0.0137152470008867));
#21191=CARTESIAN_POINT('Ctrl Pts',(-0.0124037125345544,-0.0309305857104295,
-0.0137158759876751));
#21192=CARTESIAN_POINT('Ctrl Pts',(-0.0124188104996167,-0.0309297896015973,
-0.0137167256807697));
#21193=CARTESIAN_POINT('Ctrl Pts',(-0.0124243234717443,-0.0309295005659932,
-0.0137170062754458));
#21194=CARTESIAN_POINT('Ctrl Pts',(-0.0124346659409761,-0.0309289615968069,
-0.0137174770470344));
#21195=CARTESIAN_POINT('Ctrl Pts',(-0.0124394948270623,-0.0309287113066356,
-0.0137176741200312));
#21196=CARTESIAN_POINT('Ctrl Pts',(-0.0124508169665904,-0.0309281275309323,
-0.0137180829170477));
#21197=CARTESIAN_POINT('Ctrl Pts',(-0.0124573107200674,-0.0309277950628319,
-0.013718276325883));
#21198=CARTESIAN_POINT('Ctrl Pts',(-0.0124786578030399,-0.0309267093106307,
-0.01371877720549));
#21199=CARTESIAN_POINT('Ctrl Pts',(-0.0124935147706009,-0.0309259650759251,
-0.0137189111861308));
#21200=CARTESIAN_POINT('Ctrl Pts',(-0.012529504346246,-0.0309241850212241,
-0.0137187159144776));
#21201=CARTESIAN_POINT('Ctrl Pts',(-0.0125506330762215,-0.0309231590068975,
-0.0137181671182491));
#21202=CARTESIAN_POINT('Ctrl Pts',(-0.0126360418514792,-0.0309190654877355,
-0.0137141915793627));
#21203=CARTESIAN_POINT('Ctrl Pts',(-0.012700092534102,-0.0309161174221325,
-0.0137071782008028));
#21204=CARTESIAN_POINT('Ctrl Pts',(-0.012871342986869,-0.0309081699097549,
-0.0136774951502817));
#21205=CARTESIAN_POINT('Ctrl Pts',(-0.0129768606266926,-0.0309031799190236,
-0.0136473917860184));
#21206=CARTESIAN_POINT('Ctrl Pts',(-0.0130979618606991,-0.0308967704333187,
-0.0135984355095743));
#21207=CARTESIAN_POINT('Ctrl Pts',(-0.0131174528354949,-0.0308957176050501,
-0.0135900847065962));
#21208=CARTESIAN_POINT('Ctrl Pts',(-0.0131465645792169,-0.0308941100558627,
-0.0135768953946216));
#21209=CARTESIAN_POINT('Ctrl Pts',(-0.0131563173006883,-0.030893565478811,
-0.0135723533176647));
#21210=CARTESIAN_POINT('Ctrl Pts',(-0.0131737293795579,-0.0308925820122013,
-0.0135640214092683));
#21211=CARTESIAN_POINT('Ctrl Pts',(-0.0131814063120283,-0.0308921444469597,
-0.0135602692095438));
#21212=CARTESIAN_POINT('Ctrl Pts',(-0.0131977057952542,-0.030891206788878,
-0.0135521342080454));
#21213=CARTESIAN_POINT('Ctrl Pts',(-0.0132063190667737,-0.0308907060857857,
-0.0135477337193074));
#21214=CARTESIAN_POINT('Ctrl Pts',(-0.0132296036359554,-0.0308893380728076,
-0.0135355603097986));
#21215=CARTESIAN_POINT('Ctrl Pts',(-0.0132441914788461,-0.0308884652523189,
-0.0135276312521803));
#21216=CARTESIAN_POINT('Ctrl Pts',(-0.0133332288349783,-0.0308830385571604,
-0.0134773579121625));
#21217=CARTESIAN_POINT('Ctrl Pts',(-0.0134041636691832,-0.0308782693275541,
-0.0134291166730617));
#21218=CARTESIAN_POINT('Ctrl Pts',(-0.0135340838198056,-0.030868733716134,
-0.0133239665058592));
#21219=CARTESIAN_POINT('Ctrl Pts',(-0.0135932805261852,-0.0308639952928679,
-0.0132677465442893));
#21220=CARTESIAN_POINT('Ctrl Pts',(-0.0136772695135252,-0.0308568873207405,
-0.0131742695953239));
#21221=CARTESIAN_POINT('Ctrl Pts',(-0.0137053592258453,-0.0308544324730081,
-0.0131401708623074));
#21222=CARTESIAN_POINT('Ctrl Pts',(-0.0137377792462662,-0.0308515465744558,
-0.0130971812862224));
#21223=CARTESIAN_POINT('Ctrl Pts',(-0.0137435362833015,-0.0308510319370611,
-0.0130893959877722));
#21224=CARTESIAN_POINT('Ctrl Pts',(-0.0137524705225291,-0.0308502305148623,
-0.0130770731601995));
#21225=CARTESIAN_POINT('Ctrl Pts',(-0.0137556971352038,-0.030849940497253,
-0.0130725719587064));
#21226=CARTESIAN_POINT('Ctrl Pts',(-0.013761408353671,-0.0308494262564917,
-0.0130645133967215));
#21227=CARTESIAN_POINT('Ctrl Pts',(-0.0137639022094597,-0.0308492014100959,
-0.0130609629020573));
#21228=CARTESIAN_POINT('Ctrl Pts',(-0.0137699038301692,-0.0308486595189075,
-0.0130523413240749));
#21229=CARTESIAN_POINT('Ctrl Pts',(-0.0137733962086973,-0.0308483435160092,
-0.0130472596877231));
#21230=CARTESIAN_POINT('Ctrl Pts',(-0.0137841950752339,-0.0308473638266477,
-0.0130313430788124));
#21231=CARTESIAN_POINT('Ctrl Pts',(-0.0137913946134809,-0.0308467069408973,
-0.0130204358755078));
#21232=CARTESIAN_POINT('Ctrl Pts',(-0.013827828768116,-0.0308433559756539,
-0.0129636832785706));
#21233=CARTESIAN_POINT('Ctrl Pts',(-0.0138547661281363,-0.030840786408751,
-0.0129164037821995));
#21234=CARTESIAN_POINT('Ctrl Pts',(-0.0139248674980924,-0.0308335386331882,
-0.0127766807744706));
#21235=CARTESIAN_POINT('Ctrl Pts',(-0.013961439716183,-0.0308289842246961,
-0.0126812595850956));
#21236=CARTESIAN_POINT('Ctrl Pts',(-0.0140021511263143,-0.0308217251250766,
-0.0125324114727777));
#21237=CARTESIAN_POINT('Ctrl Pts',(-0.0140133858916283,-0.030819206517818,
-0.0124812288204585));
#21238=CARTESIAN_POINT('Ctrl Pts',(-0.014024495316186,-0.0308158496982509,
-0.0124145873610451));
#21239=CARTESIAN_POINT('Ctrl Pts',(-0.0140267724902431,-0.0308150879787133,
-0.0123995621812588));
#21240=CARTESIAN_POINT('Ctrl Pts',(-0.0140300931750389,-0.030813845652624,
-0.0123752310809937));
#21241=CARTESIAN_POINT('Ctrl Pts',(-0.0140312745770285,-0.0308133694373306,
-0.0123659448273697));
#21242=CARTESIAN_POINT('Ctrl Pts',(-0.0140333367189323,-0.0308124690384065,
-0.0123484666725585));
#21243=CARTESIAN_POINT('Ctrl Pts',(-0.0140342364899137,-0.0308120454762187,
-0.0123402773241824));
#21244=CARTESIAN_POINT('Ctrl Pts',(-0.0140359147144746,-0.0308111890925589,
-0.0123237873637089));
#21245=CARTESIAN_POINT('Ctrl Pts',(-0.0140366915631573,-0.0308107562353505,
-0.012315486869047));
#21246=CARTESIAN_POINT('Ctrl Pts',(-0.014038320504432,-0.0308097575942595,
-0.0122964174451424));
#21247=CARTESIAN_POINT('Ctrl Pts',(-0.0140391268413355,-0.030809190389752,
-0.0122856451302186));
#21248=CARTESIAN_POINT('Ctrl Pts',(-0.014041939566174,-0.0308068743987195,
-0.0122419021072547));
#21249=CARTESIAN_POINT('Ctrl Pts',(-0.0140430000000001,-0.030805096474939,
-0.0122088811687427));
#21250=CARTESIAN_POINT('Ctrl Pts',(-0.014043,-0.0308032888456207,-0.0121758532865555));
#21251=CARTESIAN_POINT('Ctrl Pts',(-0.014043,-0.0309187674097093,-0.0121758533048748));
#21252=CARTESIAN_POINT('Ctrl Pts',(-0.0140429999997999,-0.0309197267292913,
-0.0121927073390054));
#21253=CARTESIAN_POINT('Ctrl Pts',(-0.0140427238577457,-0.0309206814208278,
-0.0122095645227286));
#21254=CARTESIAN_POINT('Ctrl Pts',(-0.0140413384621183,-0.0309230574164513,
-0.0122518175606727));
#21255=CARTESIAN_POINT('Ctrl Pts',(-0.0140398782586855,-0.0309244690359173,
-0.0122771937571986));
#21256=CARTESIAN_POINT('Ctrl Pts',(-0.0140363931382051,-0.0309267847732897,
-0.0123195035874159));
#21257=CARTESIAN_POINT('Ctrl Pts',(-0.0140347132494167,-0.0309277026349426,
-0.012336460176902));
#21258=CARTESIAN_POINT('Ctrl Pts',(-0.014031962124351,-0.030928970686247,
-0.0123602123718667));
#21259=CARTESIAN_POINT('Ctrl Pts',(-0.0140311258586705,-0.0309293327863993,
-0.0123670333880292));
#21260=CARTESIAN_POINT('Ctrl Pts',(-0.0140296149479145,-0.0309299489013664,
-0.0123787107393482));
#21261=CARTESIAN_POINT('Ctrl Pts',(-0.0140289626800033,-0.0309302041436871,
-0.0123835698257165));
#21262=CARTESIAN_POINT('Ctrl Pts',(-0.0140275471559694,-0.0309307362609983,
-0.0123937467129794));
#21263=CARTESIAN_POINT('Ctrl Pts',(-0.0140267792772837,-0.0309310128789367,
-0.0123990637234993));
#21264=CARTESIAN_POINT('Ctrl Pts',(-0.0140246335990807,-0.0309317547926685,
-0.0124133916641692));
#21265=CARTESIAN_POINT('Ctrl Pts',(-0.0140232036731765,-0.0309322172402755,
-0.0124223947029267));
#21266=CARTESIAN_POINT('Ctrl Pts',(-0.0140160595552021,-0.0309343870014191,
-0.012464938041969));
#21267=CARTESIAN_POINT('Ctrl Pts',(-0.0140093164845565,-0.0309360427540956,
-0.0124982980427139));
#21268=CARTESIAN_POINT('Ctrl Pts',(-0.0139810469113904,-0.030941888174126,
-0.0126176772879945));
#21269=CARTESIAN_POINT('Ctrl Pts',(-0.0139532205792408,-0.0309458753313444,
-0.0127020283231891));
#21270=CARTESIAN_POINT('Ctrl Pts',(-0.0138830248715679,-0.0309540546000406,
-0.0128658643282637));
#21271=CARTESIAN_POINT('Ctrl Pts',(-0.0138406470350087,-0.030958236270876,
-0.0129449672449545));
#21272=CARTESIAN_POINT('Ctrl Pts',(-0.0137824822075436,-0.0309635013414945,
-0.0130339729371519));
#21273=CARTESIAN_POINT('Ctrl Pts',(-0.0137730851630063,-0.0309643393753712,
-0.0130478533366812));
#21274=CARTESIAN_POINT('Ctrl Pts',(-0.0137578787239697,-0.0309656773985198,
-0.0130695449510751));
#21275=CARTESIAN_POINT('Ctrl Pts',(-0.0137522182108292,-0.0309661716973291,
-0.0130774591994918));
#21276=CARTESIAN_POINT('Ctrl Pts',(-0.0137414283646035,-0.0309671071460843,
-0.0130922473977398));
#21277=CARTESIAN_POINT('Ctrl Pts',(-0.0137363158197064,-0.0309675476317604,
-0.0130991331690595));
#21278=CARTESIAN_POINT('Ctrl Pts',(-0.0137246525950884,-0.0309685465186392,
-0.0131145710639826));
#21279=CARTESIAN_POINT('Ctrl Pts',(-0.0137180692685168,-0.0309691061996272,
-0.0131230978660948));
#21280=CARTESIAN_POINT('Ctrl Pts',(-0.0136982971299149,-0.0309707753298544,
-0.0131481599935476));
#21281=CARTESIAN_POINT('Ctrl Pts',(-0.0136848573908443,-0.0309718947833409,
-0.0131644933865907));
#21282=CARTESIAN_POINT('Ctrl Pts',(-0.013599607983548,-0.0309789066292323,
-0.013263861633095));
#21283=CARTESIAN_POINT('Ctrl Pts',(-0.0135194521904476,-0.0309851545951428,
-0.0133393009105908));
#21284=CARTESIAN_POINT('Ctrl Pts',(-0.0133808170987185,-0.0309951608916098,
-0.0134443691810781));
#21285=CARTESIAN_POINT('Ctrl Pts',(-0.0133272741725891,-0.0309988588622458,
-0.0134799197867874));
#21286=CARTESIAN_POINT('Ctrl Pts',(-0.0132533798821043,-0.0310036199124827,
-0.0135225952334969));
#21287=CARTESIAN_POINT('Ctrl Pts',(-0.0132348737252259,-0.0310047851272844,
-0.0135327820979586));
#21288=CARTESIAN_POINT('Ctrl Pts',(-0.0132030001029772,-0.0310067390190267,
-0.0135494837710494));
#21289=CARTESIAN_POINT('Ctrl Pts',(-0.0131897372243734,-0.0310075368144819,
-0.0135561910879665));
#21290=CARTESIAN_POINT('Ctrl Pts',(-0.0131705263658104,-0.0310086683968085,
-0.01356556037592));
#21291=CARTESIAN_POINT('Ctrl Pts',(-0.0131646555701357,-0.0310090110245991,
-0.0135683777486628));
#21292=CARTESIAN_POINT('Ctrl Pts',(-0.0131543807138519,-0.0310096049105123,
-0.013573228830074));
#21293=CARTESIAN_POINT('Ctrl Pts',(-0.0131499846347196,-0.031009857166506,
-0.0135752790634877));
#21294=CARTESIAN_POINT('Ctrl Pts',(-0.0131405376316122,-0.0310103952635411,
-0.0135796308146671));
#21295=CARTESIAN_POINT('Ctrl Pts',(-0.0131354839011096,-0.0310106807144809,
-0.0135819258377602));
#21296=CARTESIAN_POINT('Ctrl Pts',(-0.0131215875496647,-0.0310114593267562,
-0.0135881462857946));
#21297=CARTESIAN_POINT('Ctrl Pts',(-0.0131127200845871,-0.0310119492118839,
-0.013592015955395));
#21298=CARTESIAN_POINT('Ctrl Pts',(-0.013063767907049,-0.0310146185447421,
-0.0136128322959929));
#21299=CARTESIAN_POINT('Ctrl Pts',(-0.0130230134595776,-0.0310167126499927,
-0.0136281619406473));
#21300=CARTESIAN_POINT('Ctrl Pts',(-0.01290386020267,-0.0310226143502235,
-0.0136673131991004));
#21301=CARTESIAN_POINT('Ctrl Pts',(-0.0128241435143882,-0.0310263011890831,
-0.0136866437324693));
#21302=CARTESIAN_POINT('Ctrl Pts',(-0.012665844421335,-0.0310336686199884,
-0.0137119169659547));
#21303=CARTESIAN_POINT('Ctrl Pts',(-0.0125875982687394,-0.0310373329892026,
-0.0137183580556447));
#21304=CARTESIAN_POINT('Ctrl Pts',(-0.0124882326912814,-0.0310422129895159,
-0.013718950971472));
#21305=CARTESIAN_POINT('Ctrl Pts',(-0.0124672587562583,-0.0310432552753258,
-0.0137186484423189));
#21306=CARTESIAN_POINT('Ctrl Pts',(-0.0124357069778531,-0.0310448442603338,
-0.0137175496624171));
#21307=CARTESIAN_POINT('Ctrl Pts',(-0.0124251201090016,-0.0310453809899061,
-0.0137170717339816));
#21308=CARTESIAN_POINT('Ctrl Pts',(-0.0124059903499639,-0.031046357579604,
-0.013716010581419));
#21309=CARTESIAN_POINT('Ctrl Pts',(-0.0123974457426624,-0.03104679622856,
-0.0137154652271415));
#21310=CARTESIAN_POINT('Ctrl Pts',(-0.0123790810876162,-0.0310477444113113,
-0.013714139558045));
#21311=CARTESIAN_POINT('Ctrl Pts',(-0.0123692631224394,-0.0310482546528639,
-0.013713336261814));
#21312=CARTESIAN_POINT('Ctrl Pts',(-0.0123426482946646,-0.0310496471127105,
-0.0137109018930533));
#21313=CARTESIAN_POINT('Ctrl Pts',(-0.0123258697440226,-0.031050535011485,
-0.0137090892132329));
#21314=CARTESIAN_POINT('Ctrl Pts',(-0.012216813550849,-0.031056373395258,
-0.0136954941044142));
#21315=CARTESIAN_POINT('Ctrl Pts',(-0.0121257454425382,-0.0310615806010856,
-0.0136756638961651));
#21316=CARTESIAN_POINT('Ctrl Pts',(-0.0119600813405946,-0.0310715218734116,
-0.0136235561292637));
#21317=CARTESIAN_POINT('Ctrl Pts',(-0.0118851501116786,-0.0310762074079022,
-0.0135933565807054));
#21318=CARTESIAN_POINT('Ctrl Pts',(-0.0117900448187887,-0.0310821782538876,
-0.0135460596560954));
#21319=CARTESIAN_POINT('Ctrl Pts',(-0.0117674517988811,-0.0310835978162309,
-0.0135341150823386));
#21320=CARTESIAN_POINT('Ctrl Pts',(-0.0117302459833056,-0.0310859250798677,
-0.0135132464042558));
#21321=CARTESIAN_POINT('Ctrl Pts',(-0.011715466625256,-0.0310868466852827,
-0.0135046305549598));
#21322=CARTESIAN_POINT('Ctrl Pts',(-0.0116949451066805,-0.0310881189824366,
-0.0134922054412082));
#21323=CARTESIAN_POINT('Ctrl Pts',(-0.01168908100374,-0.0310884816851732,
-0.0134886010770101));
#21324=CARTESIAN_POINT('Ctrl Pts',(-0.0116790798933332,-0.031089098515078,
-0.0134823613173361));
#21325=CARTESIAN_POINT('Ctrl Pts',(-0.0116749310045456,-0.0310893538766728,
-0.0134797452342304));
#21326=CARTESIAN_POINT('Ctrl Pts',(-0.011666267956283,-0.0310898858840773,
-0.0134742248394573));
#21327=CARTESIAN_POINT('Ctrl Pts',(-0.0116617564013197,-0.0310901622765562,
-0.0134713167098475));
#21328=CARTESIAN_POINT('Ctrl Pts',(-0.0116496410565979,-0.0310909029549704,
-0.0134634174184723));
#21329=CARTESIAN_POINT('Ctrl Pts',(-0.0116420659629052,-0.0310913644087414,
-0.0134583823981348));
#21330=CARTESIAN_POINT('Ctrl Pts',(-0.0116065589249322,-0.0310935217388308,
-0.0134343261755774));
#21331=CARTESIAN_POINT('Ctrl Pts',(-0.0115792105544783,-0.0310951667641105,
-0.0134144565560531));
#21332=CARTESIAN_POINT('Ctrl Pts',(-0.0114824342448742,-0.0311010109886243,
-0.0133391663908452));
#21333=CARTESIAN_POINT('Ctrl Pts',(-0.0114171692275707,-0.031105005431088,
-0.0132786754863899));
#21334=CARTESIAN_POINT('Ctrl Pts',(-0.0112971988020621,-0.0311131963200409,
-0.0131465023820683));
#21335=CARTESIAN_POINT('Ctrl Pts',(-0.0112428369460793,-0.0311173821542475,
-0.0130749801744246));
#21336=CARTESIAN_POINT('Ctrl Pts',(-0.0111860523406025,-0.0311226520673691,
-0.0129849710500098));
#21337=CARTESIAN_POINT('Ctrl Pts',(-0.0111773398722174,-0.0311234901848296,
-0.0129706489618191));
#21338=CARTESIAN_POINT('Ctrl Pts',(-0.0111639419606316,-0.0311248282860984,
-0.012947794080044));
#21339=CARTESIAN_POINT('Ctrl Pts',(-0.0111591008255313,-0.0311253225772011,
-0.0129393538245042));
#21340=CARTESIAN_POINT('Ctrl Pts',(-0.0111501438200613,-0.0311262579761414,
-0.0129233897948665));
#21341=CARTESIAN_POINT('Ctrl Pts',(-0.0111460102048364,-0.0311266984193158,
-0.0129158763729574));
#21342=CARTESIAN_POINT('Ctrl Pts',(-0.0111368266679554,-0.0311276971607501,
-0.0128988494615704));
#21343=CARTESIAN_POINT('Ctrl Pts',(-0.0111318133316558,-0.0311282567380392,
-0.0128893168349656));
#21344=CARTESIAN_POINT('Ctrl Pts',(-0.0111169256987649,-0.031129963151428,
-0.0128602746366784));
#21345=CARTESIAN_POINT('Ctrl Pts',(-0.0111073662144627,-0.0311311209257603,
-0.012840607512082));
#21346=CARTESIAN_POINT('Ctrl Pts',(-0.0110607219278723,-0.031137102606807,
-0.0127392188744835));
#21347=CARTESIAN_POINT('Ctrl Pts',(-0.0110304041011302,-0.0311421528906475,
-0.0126545872917843));
#21348=CARTESIAN_POINT('Ctrl Pts',(-0.0109903420781809,-0.0311511948352812,
-0.0125020507816218));
#21349=CARTESIAN_POINT('Ctrl Pts',(-0.0109774359771608,-0.0311551327015931,
-0.0124352195095036));
#21350=CARTESIAN_POINT('Ctrl Pts',(-0.0109651997208015,-0.0311606998811778,
-0.0123375965698176));
#21351=CARTESIAN_POINT('Ctrl Pts',(-0.0109623113754691,-0.031162399786375,
-0.0123073320358549));
#21352=CARTESIAN_POINT('Ctrl Pts',(-0.0109590484480718,-0.031165127141809,
-0.0122576632037539));
#21353=CARTESIAN_POINT('Ctrl Pts',(-0.0109581424565425,-0.0311661747410972,
-0.0122383027164186));
#21354=CARTESIAN_POINT('Ctrl Pts',(-0.0109573997453987,-0.0311675877622278,
-0.0122117089779379));
#21355=CARTESIAN_POINT('Ctrl Pts',(-0.010957248792155,-0.0311679688627185,
-0.0122044870225952));
#21356=CARTESIAN_POINT('Ctrl Pts',(-0.0109570796508526,-0.0311686072878051,
-0.0121922988135003));
#21357=CARTESIAN_POINT('Ctrl Pts',(-0.0109570347133661,-0.0311688660655803,
-0.0121873330838899));
#21358=CARTESIAN_POINT('Ctrl Pts',(-0.0109569916181838,-0.0311693952042206,
-0.0121771247251873));
#21359=CARTESIAN_POINT('Ctrl Pts',(-0.0109569962038278,-0.0311696654148973,
-0.0121718822021046));
#21360=CARTESIAN_POINT('Ctrl Pts',(-0.0109570784197879,-0.0311703712887587,
-0.0121581136928511));
#21361=CARTESIAN_POINT('Ctrl Pts',(-0.0109572000003191,-0.0311708045647993,
-0.0121495880395073));
#21362=CARTESIAN_POINT('Ctrl Pts',(-0.0109580187732477,-0.0311726349978654,
-0.0121132828204177));
#21363=CARTESIAN_POINT('Ctrl Pts',(-0.010959395680332,-0.0311739982119459,
-0.0120855223909404));
#21364=CARTESIAN_POINT('Ctrl Pts',(-0.0109686508018625,-0.0311798198603566,
-0.0119648959344783));
#21365=CARTESIAN_POINT('Ctrl Pts',(-0.0109841832778093,-0.0311840101716126,
-0.0118728094945433));
#21366=CARTESIAN_POINT('Ctrl Pts',(-0.0110314466607925,-0.0311925138532889,
-0.0116934467709577));
#21367=CARTESIAN_POINT('Ctrl Pts',(-0.0110629169821904,-0.0311968121845459,
-0.0116065072015876));
#21368=CARTESIAN_POINT('Ctrl Pts',(-0.0111090846695419,-0.0312022138392394,
-0.0115076565783938));
#21369=CARTESIAN_POINT('Ctrl Pts',(-0.0111164560409825,-0.0312030552750401,
-0.0114925243886525));
#21370=CARTESIAN_POINT('Ctrl Pts',(-0.0111284836261574,-0.0312043974756499,
-0.0114688265567624));
#21371=CARTESIAN_POINT('Ctrl Pts',(-0.0111329760998269,-0.0312048924871565,
-0.0114601790512941));
#21372=CARTESIAN_POINT('Ctrl Pts',(-0.011141574594219,-0.0312058285074883,
-0.011444004309123));
#21373=CARTESIAN_POINT('Ctrl Pts',(-0.0111456620439648,-0.0312062688419898,
-0.0114364675917224));
#21374=CARTESIAN_POINT('Ctrl Pts',(-0.0111550150009916,-0.0312072663301049,
-0.01141955976564));
#21375=CARTESIAN_POINT('Ctrl Pts',(-0.011160316010977,-0.0312078247494321,
-0.0114102088919434));
#21376=CARTESIAN_POINT('Ctrl Pts',(-0.0111766388626056,-0.0312095239808521,
-0.0113821042925125));
#21377=CARTESIAN_POINT('Ctrl Pts',(-0.0111879596588067,-0.0312106755962077,
-0.0113635280786875));
#21378=CARTESIAN_POINT('Ctrl Pts',(-0.0112528187808207,-0.0312171317976559,
-0.0112619957958249));
#21379=CARTESIAN_POINT('Ctrl Pts',(-0.0113138241330732,-0.0312227164045157,
-0.0111840981045602));
#21380=CARTESIAN_POINT('Ctrl Pts',(-0.0114316282162692,-0.0312325385762263,
-0.0110602141609473));
#21381=CARTESIAN_POINT('Ctrl Pts',(-0.0114850322445972,-0.0312367177322726,
-0.0110114177966349));
#21382=CARTESIAN_POINT('Ctrl Pts',(-0.0115593191796873,-0.0312420197606286,
-0.0109525478163445));
#21383=CARTESIAN_POINT('Ctrl Pts',(-0.0115772833932574,-0.0312432657176012,
-0.0109389414752818));
#21384=CARTESIAN_POINT('Ctrl Pts',(-0.0116081740004673,-0.0312453392971401,
-0.0109165921695208));
#21385=CARTESIAN_POINT('Ctrl Pts',(-0.0116209464427121,-0.0312461774619369,
-0.0109076431090239));
#21386=CARTESIAN_POINT('Ctrl Pts',(-0.0116393454923739,-0.0312473552021274,
-0.0108951632897102));
#21387=CARTESIAN_POINT('Ctrl Pts',(-0.0116448622419863,-0.031247704604537,
-0.010891473098485));
#21388=CARTESIAN_POINT('Ctrl Pts',(-0.0116544654328692,-0.0312483061370609,
-0.0108851387624942));
#21389=CARTESIAN_POINT('Ctrl Pts',(-0.0116585408457478,-0.0312485593448531,
-0.010882478174338));
#21390=CARTESIAN_POINT('Ctrl Pts',(-0.0116672333130352,-0.0312490949490242,
-0.0108768618717511));
#21391=CARTESIAN_POINT('Ctrl Pts',(-0.0116718535883144,-0.0312493770050019,
-0.0108739114394363));
#21392=CARTESIAN_POINT('Ctrl Pts',(-0.0116846238486616,-0.0312501496512385,
-0.010865852045191));
#21393=CARTESIAN_POINT('Ctrl Pts',(-0.0116928061608303,-0.0312506369741942,
-0.0108607944911011));
#21394=CARTESIAN_POINT('Ctrl Pts',(-0.0117357025130474,-0.0312531545595775,
-0.0108348311298225));
#21395=CARTESIAN_POINT('Ctrl Pts',(-0.0117711853453037,-0.031255111143097,
-0.0108152208042713));
#21396=CARTESIAN_POINT('Ctrl Pts',(-0.0118824743987821,-0.0312609925952532,
-0.0107593190983834));
#21397=CARTESIAN_POINT('Ctrl Pts',(-0.0119605045893482,-0.0312647732333334,
-0.0107278018578865));
#21398=CARTESIAN_POINT('Ctrl Pts',(-0.0121165116196277,-0.031272279977967,
-0.0106791605316225));
#21399=CARTESIAN_POINT('Ctrl Pts',(-0.0121940131859898,-0.0312759873359157,
-0.0106614151083494));
#21400=CARTESIAN_POINT('Ctrl Pts',(-0.0122933978351906,-0.0312809209924038,
-0.0106466019452003));
#21401=CARTESIAN_POINT('Ctrl Pts',(-0.0123143260863358,-0.031281969229822,
-0.0106439201080648));
#21402=CARTESIAN_POINT('Ctrl Pts',(-0.0123458631698375,-0.0312835654911346,
-0.0106405345384491));
#21403=CARTESIAN_POINT('Ctrl Pts',(-0.0123564354451908,-0.0312841034040758,
-0.0106395098900538));
#21404=CARTESIAN_POINT('Ctrl Pts',(-0.012375549059105,-0.031285081251584,
-0.0106378564402917));
#21405=CARTESIAN_POINT('Ctrl Pts',(-0.0123840867072331,-0.0312855199601821,
-0.0106371894374848));
#21406=CARTESIAN_POINT('Ctrl Pts',(-0.0124024385166975,-0.0312864672622507,
-0.010635909311979));
#21407=CARTESIAN_POINT('Ctrl Pts',(-0.0124122538382186,-0.0312869765519656,
-0.0106353188685943));
#21408=CARTESIAN_POINT('Ctrl Pts',(-0.0124388490866719,-0.0312883638656256,
-0.0106339740145444));
#21409=CARTESIAN_POINT('Ctrl Pts',(-0.0124556364473477,-0.0312892475002527,
-0.0106333997317607));
#21410=CARTESIAN_POINT('Ctrl Pts',(-0.0125704938159743,-0.0312953492017711,
-0.0106313471124719));
#21411=CARTESIAN_POINT('Ctrl Pts',(-0.012668487372212,-0.0313008553547883,
-0.0106389487559617));
#21412=CARTESIAN_POINT('Ctrl Pts',(-0.0128429466235424,-0.0313110090258485,
-0.0106693727204599));
#21413=CARTESIAN_POINT('Ctrl Pts',(-0.0129196526182226,-0.0313155950207616,
-0.0106889140619312));
#21414=CARTESIAN_POINT('Ctrl Pts',(-0.0130168898550949,-0.0313213476946538,
-0.0107218136260671));
#21415=CARTESIAN_POINT('Ctrl Pts',(-0.0130390792974556,-0.0313226555674681,
-0.0107298933754122));
#21416=CARTESIAN_POINT('Ctrl Pts',(-0.0130761133177147,-0.0313248201810509,
-0.0107443495181992));
#21417=CARTESIAN_POINT('Ctrl Pts',(-0.0130910587182855,-0.0313256886165501,
-0.0107504553682053));
#21418=CARTESIAN_POINT('Ctrl Pts',(-0.0131120939334941,-0.0313269007924542,
-0.0107594369331056));
#21419=CARTESIAN_POINT('Ctrl Pts',(-0.0131182645298868,-0.0313272551293908,
-0.0107621194912024));
#21420=CARTESIAN_POINT('Ctrl Pts',(-0.013128880205169,-0.0313278622994748,
-0.0107668172673062));
#21421=CARTESIAN_POINT('Ctrl Pts',(-0.0131333335911517,-0.0313281162683805,
-0.0107688133508342));
#21422=CARTESIAN_POINT('Ctrl Pts',(-0.0131427281013041,-0.0313286503610117,
-0.0107730777716749));
#21423=CARTESIAN_POINT('Ctrl Pts',(-0.0131476667777454,-0.0313289301780944,
-0.0107753511251391));
#21424=CARTESIAN_POINT('Ctrl Pts',(-0.0131611214909912,-0.0313296901569358,
-0.0107816309421281));
#21425=CARTESIAN_POINT('Ctrl Pts',(-0.0131696131809573,-0.031330167226973,
-0.0107856893509535));
#21426=CARTESIAN_POINT('Ctrl Pts',(-0.0132118066745237,-0.0313325273371271,
-0.0108063310933569));
#21427=CARTESIAN_POINT('Ctrl Pts',(-0.0132449344289738,-0.0313343472715819,
-0.0108240645205944));
#21428=CARTESIAN_POINT('Ctrl Pts',(-0.0133517755032359,-0.0313402109989266,
-0.0108863789230458));
#21429=CARTESIAN_POINT('Ctrl Pts',(-0.0134224073458359,-0.0313440852657322,
-0.0109359210994207));
#21430=CARTESIAN_POINT('Ctrl Pts',(-0.0135502929232256,-0.0313517326713571,
-0.0110426267863424));
#21431=CARTESIAN_POINT('Ctrl Pts',(-0.0136079193139404,-0.0313554846830447,
-0.0110988989378598));
#21432=CARTESIAN_POINT('Ctrl Pts',(-0.0136748757773923,-0.0313604741009463,
-0.0111753702043208));
#21433=CARTESIAN_POINT('Ctrl Pts',(-0.0136885261557252,-0.0313615284658871,
-0.0111916251562969));
#21434=CARTESIAN_POINT('Ctrl Pts',(-0.013708513501919,-0.0313631322157503,
-0.0112164485420964));
#21435=CARTESIAN_POINT('Ctrl Pts',(-0.0137151043714358,-0.0313636713432469,
-0.0112248098032431));
#21436=CARTESIAN_POINT('Ctrl Pts',(-0.0137267926811872,-0.031364646481713,
-0.0112399575957178));
#21437=CARTESIAN_POINT('Ctrl Pts',(-0.013731921686652,-0.0313650812109238,
-0.0112467192914424));
#21438=CARTESIAN_POINT('Ctrl Pts',(-0.0137428446459158,-0.0313660220366368,
-0.0112613687502036));
#21439=CARTESIAN_POINT('Ctrl Pts',(-0.0137486198364894,-0.031366528842055,
-0.0112692699869681));
#21440=CARTESIAN_POINT('Ctrl Pts',(-0.0137639816519964,-0.0313679027444263,
-0.0112907122608906));
#21441=CARTESIAN_POINT('Ctrl Pts',(-0.0137734255022911,-0.0313687752719427,
-0.0113043535946737));
#21442=CARTESIAN_POINT('Ctrl Pts',(-0.0138262623926238,-0.0313738218903273,
-0.0113833676767165));
#21443=CARTESIAN_POINT('Ctrl Pts',(-0.0138648334690308,-0.0313781741396072,
-0.0114518144486001));
#21444=CARTESIAN_POINT('Ctrl Pts',(-0.0139383546983522,-0.031388052756501,
-0.0116092272285832));
#21445=CARTESIAN_POINT('Ctrl Pts',(-0.0139705940672988,-0.031393613462857,
-0.011699112259949));
#21446=CARTESIAN_POINT('Ctrl Pts',(-0.0140007705764022,-0.0314004243894994,
-0.0118164043836479));
#21447=CARTESIAN_POINT('Ctrl Pts',(-0.0140065762251424,-0.0314018596450021,
-0.0118415719137731));
#21448=CARTESIAN_POINT('Ctrl Pts',(-0.014015199515888,-0.031404209607931,
-0.0118837632711088));
#21449=CARTESIAN_POINT('Ctrl Pts',(-0.0140183682408435,-0.0314051385426463,
-0.0119007095351413));
#21450=CARTESIAN_POINT('Ctrl Pts',(-0.0140224074768403,-0.031406419095244,
-0.011924512604793));
#21451=CARTESIAN_POINT('Ctrl Pts',(-0.0140235168407667,-0.0314067829250573,
-0.0119313270030986));
#21452=CARTESIAN_POINT('Ctrl Pts',(-0.0140253365821976,-0.03140740106837,
-0.011942998392169));
#21453=CARTESIAN_POINT('Ctrl Pts',(-0.0140260695839526,-0.0314076566295594,
-0.01194785171153));
#21454=CARTESIAN_POINT('Ctrl Pts',(-0.0140275544431892,-0.0314081884094914,
-0.0119580112748559));
#21455=CARTESIAN_POINT('Ctrl Pts',(-0.0140283018302413,-0.0314084643816878,
-0.0119633180274747));
#21456=CARTESIAN_POINT('Ctrl Pts',(-0.0140302378378962,-0.0314092026785807,
-0.0119776029958386));
#21457=CARTESIAN_POINT('Ctrl Pts',(-0.0140313751044238,-0.0314096622026436,
-0.0119865880879898));
#21458=CARTESIAN_POINT('Ctrl Pts',(-0.0140363282943189,-0.0314117950472679,
-0.0120286939042389));
#21459=CARTESIAN_POINT('Ctrl Pts',(-0.0140391494611381,-0.031413418910114,
-0.012061924657053));
#21460=CARTESIAN_POINT('Ctrl Pts',(-0.0140422975768346,-0.0314162923121628,
-0.0121220867706215));
#21461=CARTESIAN_POINT('Ctrl Pts',(-0.0140430000004932,-0.0314175525195978,
-0.0121489728247115));
#21462=CARTESIAN_POINT('Ctrl Pts',(-0.014043,-0.0314187998055481,-0.0121758533148708));
#21463=CARTESIAN_POINT('Origin',(-0.0125,-0.0375520664398416,-0.0121758532865581));
#21464=CARTESIAN_POINT('',(-0.014043,-0.0319166517728185,-0.012175853290423));
#21465=CARTESIAN_POINT('',(-0.014043,-0.0318006569328344,-0.0121758532865509));
#21466=CARTESIAN_POINT('',(-0.014043,-0.0375520664398416,-0.012175853286558));
#21467=CARTESIAN_POINT('Ctrl Pts',(-0.014043,-0.0318006569328344,-0.0121758532865438));
#21468=CARTESIAN_POINT('Ctrl Pts',(-0.014043,-0.031800630291104,-0.0121753151222929));
#21469=CARTESIAN_POINT('Ctrl Pts',(-0.0140429997179574,-0.0318006036615213,
-0.0121747769564973));
#21470=CARTESIAN_POINT('Ctrl Pts',(-0.0140429240554956,-0.0317970272351956,
-0.0121024653297101));
#21471=CARTESIAN_POINT('Ctrl Pts',(-0.0140378411364186,-0.0317936999177665,
-0.0120307775798329));
#21472=CARTESIAN_POINT('Ctrl Pts',(-0.014010173087722,-0.0317846413065578,
-0.0118352191775621));
#21473=CARTESIAN_POINT('Ctrl Pts',(-0.0139774172398278,-0.0317789769893868,
-0.0117133701000584));
#21474=CARTESIAN_POINT('Ctrl Pts',(-0.0139234868784111,-0.0317719059281056,
-0.0115801533805521));
#21475=CARTESIAN_POINT('Ctrl Pts',(-0.0139164380903339,-0.031771010882243,
-0.0115635817996873));
#21476=CARTESIAN_POINT('Ctrl Pts',(-0.0139046028958629,-0.0317695513497367,
-0.0115370563120314));
#21477=CARTESIAN_POINT('Ctrl Pts',(-0.013899996738649,-0.0317689930075452,
-0.0115270235760002));
#21478=CARTESIAN_POINT('Ctrl Pts',(-0.0138916235517631,-0.0317679945020514,
-0.0115092901880454));
#21479=CARTESIAN_POINT('Ctrl Pts',(-0.0138878992316142,-0.0317675558367389,
-0.0115015698201503));
#21480=CARTESIAN_POINT('Ctrl Pts',(-0.0138799117831603,-0.031766626197059,
-0.0114853587308294));
#21481=CARTESIAN_POINT('Ctrl Pts',(-0.0138756341846108,-0.0317661347267244,
-0.0114768755719674));
#21482=CARTESIAN_POINT('Ctrl Pts',(-0.0138640274006613,-0.0317648176722115,
-0.0114543767475489));
#21483=CARTESIAN_POINT('Ctrl Pts',(-0.0138565607304269,-0.0317639872469671,
-0.0114404336066681));
#21484=CARTESIAN_POINT('Ctrl Pts',(-0.0138159213544144,-0.0317595527490682,
-0.0113672697233371));
#21485=CARTESIAN_POINT('Ctrl Pts',(-0.0137790857770913,-0.0317558172180877,
-0.0113101777448214));
#21486=CARTESIAN_POINT('Ctrl Pts',(-0.0136808040824151,-0.0317465152106493,
-0.0111778809278317));
#21487=CARTESIAN_POINT('Ctrl Pts',(-0.0136157912680871,-0.0317408619446796,
-0.0111056871540145));
#21488=CARTESIAN_POINT('Ctrl Pts',(-0.0135094033908899,-0.0317326642940279,
-0.0110078553862304));
#21489=CARTESIAN_POINT('Ctrl Pts',(-0.013472894301811,-0.0317300099144168,
-0.0109772742436927));
#21490=CARTESIAN_POINT('Ctrl Pts',(-0.0134271763829065,-0.0317269277677483,
-0.0109424472890075));
#21491=CARTESIAN_POINT('Ctrl Pts',(-0.0134192682859518,-0.031726402955929,
-0.0109365420955482));
#21492=CARTESIAN_POINT('Ctrl Pts',(-0.0134068010642203,-0.0317255892474744,
-0.0109274174788518));
#21493=CARTESIAN_POINT('Ctrl Pts',(-0.0134022803366845,-0.0317252969600848,
-0.0109241463192546));
#21494=CARTESIAN_POINT('Ctrl Pts',(-0.0133942162168097,-0.0317247806297561,
-0.0109183775813838));
#21495=CARTESIAN_POINT('Ctrl Pts',(-0.0133906800132446,-0.0317245559367038,
-0.0109158703874805));
#21496=CARTESIAN_POINT('Ctrl Pts',(-0.0133821331609715,-0.0317240169503172,
-0.0109098645698703));
#21497=CARTESIAN_POINT('Ctrl Pts',(-0.0133771122493237,-0.0317237036638611,
-0.0109063807783821));
#21498=CARTESIAN_POINT('Ctrl Pts',(-0.01336154471605,-0.0317227421597699,
-0.0108957155984358));
#21499=CARTESIAN_POINT('Ctrl Pts',(-0.0133509293759966,-0.0317221003717403,
-0.0108886349619036));
#21500=CARTESIAN_POINT('Ctrl Pts',(-0.0132968948368375,-0.0317188964377486,
-0.0108535534804574));
#21501=CARTESIAN_POINT('Ctrl Pts',(-0.0132521733054764,-0.0317164468002304,
-0.0108276120894787));
#21502=CARTESIAN_POINT('Ctrl Pts',(-0.0131036592332028,-0.0317086819026316,
-0.0107511590444323));
#21503=CARTESIAN_POINT('Ctrl Pts',(-0.0129954912974291,-0.0317035537289001,
-0.0107100267541059));
#21504=CARTESIAN_POINT('Ctrl Pts',(-0.012841333060349,-0.0316959959845422,
-0.0106704436115146));
#21505=CARTESIAN_POINT('Ctrl Pts',(-0.0127984774933241,-0.0316938737939708,
-0.0106613641597208));
#21506=CARTESIAN_POINT('Ctrl Pts',(-0.0127411594453574,-0.0316909800703432,
-0.0106517481108439));
#21507=CARTESIAN_POINT('Ctrl Pts',(-0.0127269909217542,-0.0316902604120932,
-0.0106495736370227));
#21508=CARTESIAN_POINT('Ctrl Pts',(-0.0127037001825489,-0.0316890694806828,
-0.0106463306339442));
#21509=CARTESIAN_POINT('Ctrl Pts',(-0.0126945949243015,-0.0316886019217213,
-0.010645145567928));
#21510=CARTESIAN_POINT('Ctrl Pts',(-0.0126768648209758,-0.0316876874322071,
-0.010642998714074));
#21511=CARTESIAN_POINT('Ctrl Pts',(-0.0126682413588322,-0.0316872407946655,
-0.0106420282814334));
#21512=CARTESIAN_POINT('Ctrl Pts',(-0.0126479001148416,-0.0316861827262866,
-0.010639912803571));
#21513=CARTESIAN_POINT('Ctrl Pts',(-0.0126361766183313,-0.0316855693820485,
-0.0106388290416337));
#21514=CARTESIAN_POINT('Ctrl Pts',(-0.0125968527884696,-0.0316834998003213,
-0.0106356472322416));
#21515=CARTESIAN_POINT('Ctrl Pts',(-0.0125692097402094,-0.0316820246536008,
-0.0106341577813421));
#21516=CARTESIAN_POINT('Ctrl Pts',(-0.0124382744380537,-0.031674939488645,
-0.0106306312862919));
#21517=CARTESIAN_POINT('Ctrl Pts',(-0.0123350002987807,-0.031669038477402,
-0.0106382281837397));
#21518=CARTESIAN_POINT('Ctrl Pts',(-0.012151237794049,-0.0316583054104492,
-0.010670479162199));
#21519=CARTESIAN_POINT('Ctrl Pts',(-0.0120704952807793,-0.0316535128762213,
-0.0106914968401289));
#21520=CARTESIAN_POINT('Ctrl Pts',(-0.011978320373973,-0.0316482187122544,
-0.0107236465618568));
#21521=CARTESIAN_POINT('Ctrl Pts',(-0.0119648669779445,-0.031647450799211,
-0.0107285500422606));
#21522=CARTESIAN_POINT('Ctrl Pts',(-0.0119455658713085,-0.0316463580742347,
-0.0107358908292815));
#21523=CARTESIAN_POINT('Ctrl Pts',(-0.0119396622196268,-0.0316460250643994,
-0.010738177851672));
#21524=CARTESIAN_POINT('Ctrl Pts',(-0.0119292850441425,-0.0316454420928893,
-0.0107422715092035));
#21525=CARTESIAN_POINT('Ctrl Pts',(-0.0119248056701419,-0.0316451912436498,
-0.0107440628835124));
#21526=CARTESIAN_POINT('Ctrl Pts',(-0.0119151927200352,-0.0316446546751647,
-0.0107479596530128));
#21527=CARTESIAN_POINT('Ctrl Pts',(-0.0119100620423893,-0.0316443693588579,
-0.0107500717494829));
#21528=CARTESIAN_POINT('Ctrl Pts',(-0.0118957223472363,-0.0316435746227282,
-0.010756065489688));
#21529=CARTESIAN_POINT('Ctrl Pts',(-0.0118865393314773,-0.0316430688056284,
-0.0107600090550408));
#21530=CARTESIAN_POINT('Ctrl Pts',(-0.0118260182016705,-0.0316397518980771,
-0.0107866987026908));
#21531=CARTESIAN_POINT('Ctrl Pts',(-0.0117759115280193,-0.0316370850688512,
-0.010812145494282));
#21532=CARTESIAN_POINT('Ctrl Pts',(-0.0116275742199918,-0.0316291182848472,
-0.0108979658418662));
#21533=CARTESIAN_POINT('Ctrl Pts',(-0.0115346259594284,-0.031623996726177,
-0.0109666482075573));
#21534=CARTESIAN_POINT('Ctrl Pts',(-0.0114179772714879,-0.0316164399769792,
-0.0110749411839614));
#21535=CARTESIAN_POINT('Ctrl Pts',(-0.0113870617992448,-0.0316143103092429,
-0.0111062043809193));
#21536=CARTESIAN_POINT('Ctrl Pts',(-0.0113478781340771,-0.0316114078491724,
-0.0111493689143198));
#21537=CARTESIAN_POINT('Ctrl Pts',(-0.011338380987994,-0.0316106873466154,
-0.0111601288093045));
#21538=CARTESIAN_POINT('Ctrl Pts',(-0.0113230535894728,-0.0316094953790479,
-0.0111779903080915));
#21539=CARTESIAN_POINT('Ctrl Pts',(-0.0113171341261726,-0.0316090276412316,
-0.0111850144011765));
#21540=CARTESIAN_POINT('Ctrl Pts',(-0.0113057462058952,-0.0316081130660162,
-0.01119877491156));
#21541=CARTESIAN_POINT('Ctrl Pts',(-0.0113002711489813,-0.0316076665246123,
-0.0112055054337023));
#21542=CARTESIAN_POINT('Ctrl Pts',(-0.0112875075440424,-0.0316066091055477,
-0.0112214689773933));
#21543=CARTESIAN_POINT('Ctrl Pts',(-0.0112802673097772,-0.031605996321064,
-0.0112307397910558));
#21544=CARTESIAN_POINT('Ctrl Pts',(-0.0112563863377993,-0.0316039307063774,
-0.011262049874944));
#21545=CARTESIAN_POINT('Ctrl Pts',(-0.0112402320462533,-0.0316024590656478,
-0.0112844520379224));
#21546=CARTESIAN_POINT('Ctrl Pts',(-0.0111665650985857,-0.031595380844297,
-0.0113926153348836));
#21547=CARTESIAN_POINT('Ctrl Pts',(-0.0111171619164245,-0.0315894833894227,
-0.0114835643690004));
#21548=CARTESIAN_POINT('Ctrl Pts',(-0.0110675418461785,-0.0315821068386753,
-0.0116017997303886));
#21549=CARTESIAN_POINT('Ctrl Pts',(-0.0110584301087489,-0.031580668887265,
-0.0116250809976767));
#21550=CARTESIAN_POINT('Ctrl Pts',(-0.0110278663839119,-0.0315755474997315,
-0.0117091366087032));
#21551=CARTESIAN_POINT('Ctrl Pts',(-0.011009658438675,-0.0315719038614914,
-0.0117710257013392));
#21552=CARTESIAN_POINT('Ctrl Pts',(-0.0109930773146484,-0.0315678858214653,
-0.0118439792902322));
#21553=CARTESIAN_POINT('Ctrl Pts',(-0.010990882965122,-0.0315673342759804,
-0.0118541047582145));
#21554=CARTESIAN_POINT('Ctrl Pts',(-0.0109876416896197,-0.0315664883202947,
-0.0118698243430674));
#21555=CARTESIAN_POINT('Ctrl Pts',(-0.0109865234855263,-0.0315661900910179,
-0.0118754032650795));
#21556=CARTESIAN_POINT('Ctrl Pts',(-0.010984518280851,-0.0315656433627924,
-0.0118857029309605));
#21557=CARTESIAN_POINT('Ctrl Pts',(-0.010983622453974,-0.0315653943879511,
-0.0118904216685973));
#21558=CARTESIAN_POINT('Ctrl Pts',(-0.0109816158611639,-0.0315648255243191,
-0.0119012674562572));
#21559=CARTESIAN_POINT('Ctrl Pts',(-0.010980520136464,-0.0315645064845513,
-0.0119073971110363));
#21560=CARTESIAN_POINT('Ctrl Pts',(-0.0109771883120504,-0.0315635085460924,
-0.0119267100421606));
#21561=CARTESIAN_POINT('Ctrl Pts',(-0.0109750863987945,-0.0315628368008368,
-0.0119399161660624));
#21562=CARTESIAN_POINT('Ctrl Pts',(-0.0109649245214153,-0.0315593411971617,
-0.0120095850233701));
#21563=CARTESIAN_POINT('Ctrl Pts',(-0.0109598274102922,-0.0315566538427666,
-0.0120664396776707));
#21564=CARTESIAN_POINT('Ctrl Pts',(-0.0109545142260599,-0.0315494153022565,
-0.0122227950051354));
#21565=CARTESIAN_POINT('Ctrl Pts',(-0.0109607458248166,-0.0315449654078458,
-0.0123222318213382));
#21566=CARTESIAN_POINT('Ctrl Pts',(-0.010984675190863,-0.0315378572209813,
-0.0124713219394031));
#21567=CARTESIAN_POINT('Ctrl Pts',(-0.0109954009256225,-0.0315353746771646,
-0.0125218185770298));
#21568=CARTESIAN_POINT('Ctrl Pts',(-0.0110125450983386,-0.0315320542911416,
-0.0125864129636788));
#21569=CARTESIAN_POINT('Ctrl Pts',(-0.0110166732559227,-0.0315312902798499,
-0.0126010862606229));
#21570=CARTESIAN_POINT('Ctrl Pts',(-0.0110236909792046,-0.0315300448295888,
-0.0126246835458702));
#21571=CARTESIAN_POINT('Ctrl Pts',(-0.011026445765568,-0.031529567811064,
-0.0126336467330491));
#21572=CARTESIAN_POINT('Ctrl Pts',(-0.0110318845674109,-0.031528647916297,
-0.0126507849696059));
#21573=CARTESIAN_POINT('Ctrl Pts',(-0.0110345556072107,-0.0315282054829589,
-0.0126589637859304));
#21574=CARTESIAN_POINT('Ctrl Pts',(-0.0110408889312757,-0.0315271772916329,
-0.0126778207336216));
#21575=CARTESIAN_POINT('Ctrl Pts',(-0.0110446002438786,-0.0315265899214682,
-0.0126884817772992));
#21576=CARTESIAN_POINT('Ctrl Pts',(-0.0110568474233639,-0.0315246981823385,
-0.0127224573921279));
#21577=CARTESIAN_POINT('Ctrl Pts',(-0.0110658288473158,-0.0315233790617733,
-0.0127456062293459));
#21578=CARTESIAN_POINT('Ctrl Pts',(-0.0111179710884246,-0.0315160679038513,
-0.0128709426998285));
#21579=CARTESIAN_POINT('Ctrl Pts',(-0.0111714917336044,-0.0315097234847948,
-0.0129684517790176));
#21580=CARTESIAN_POINT('Ctrl Pts',(-0.0112806622102527,-0.0314987561664895,
-0.013124761480192));
#21581=CARTESIAN_POINT('Ctrl Pts',(-0.0113313406802289,-0.0314941765764891,
-0.0131865207481635));
#21582=CARTESIAN_POINT('Ctrl Pts',(-0.0113965066813918,-0.0314890714234106,
-0.0132544437859607));
#21583=CARTESIAN_POINT('Ctrl Pts',(-0.0114065868246255,-0.03148830165795,
-0.0132646611789313));
#21584=CARTESIAN_POINT('Ctrl Pts',(-0.0114213213747563,-0.0314872068035573,
-0.0132791853217146));
#21585=CARTESIAN_POINT('Ctrl Pts',(-0.0114258617893619,-0.0314868734739981,
-0.013283606085507));
#21586=CARTESIAN_POINT('Ctrl Pts',(-0.0114339070495687,-0.0314862901444335,
-0.0132913433587082));
#21587=CARTESIAN_POINT('Ctrl Pts',(-0.0114374004072367,-0.0314860392531805,
-0.0132946715862134));
#21588=CARTESIAN_POINT('Ctrl Pts',(-0.0114449417030782,-0.0314855028281203,
-0.0133017892228587));
#21589=CARTESIAN_POINT('Ctrl Pts',(-0.0114489944971222,-0.0314852176946538,
-0.013305573241834));
#21590=CARTESIAN_POINT('Ctrl Pts',(-0.0114603962918709,-0.0314844239995374,
-0.0133161044249919));
#21591=CARTESIAN_POINT('Ctrl Pts',(-0.011467790581762,-0.0314839190254278,
-0.0133228023941833));
#21592=CARTESIAN_POINT('Ctrl Pts',(-0.0115168794162522,-0.0314806262338454,
-0.0133664092732175));
#21593=CARTESIAN_POINT('Ctrl Pts',(-0.0115604846098879,-0.031477980269098,
-0.0134011130887091));
#21594=CARTESIAN_POINT('Ctrl Pts',(-0.0116985704139045,-0.0314701005952718,
-0.0134992943016249));
#21595=CARTESIAN_POINT('Ctrl Pts',(-0.0117982678455839,-0.0314650432427232,
-0.0135547508225012));
#21596=CARTESIAN_POINT('Ctrl Pts',(-0.0119451645025708,-0.0314574943013234,
-0.0136163676654415));
#21597=CARTESIAN_POINT('Ctrl Pts',(-0.0119879288441348,-0.0314552901873211,
-0.0136321179503589));
#21598=CARTESIAN_POINT('Ctrl Pts',(-0.0120451693595663,-0.0314523002917368,
-0.0136503665053269));
#21599=CARTESIAN_POINT('Ctrl Pts',(-0.0120590749664324,-0.0314515710219752,
-0.0136545842425752));
#21600=CARTESIAN_POINT('Ctrl Pts',(-0.0120819016179637,-0.0314503682950758,
-0.0136611572370011));
#21601=CARTESIAN_POINT('Ctrl Pts',(-0.0120907880374488,-0.0314498987012237,
-0.0136636300329526));
#21602=CARTESIAN_POINT('Ctrl Pts',(-0.0121080585018323,-0.0314489832053343,
-0.0136682693948805));
#21603=CARTESIAN_POINT('Ctrl Pts',(-0.0121164396775446,-0.0314485376299861,
-0.013670445355758));
#21604=CARTESIAN_POINT('Ctrl Pts',(-0.0121361459330668,-0.0314474867756949,
-0.0136753849156557));
#21605=CARTESIAN_POINT('Ctrl Pts',(-0.0121474847910617,-0.0314468796561892,
-0.0136780909195834));
#21606=CARTESIAN_POINT('Ctrl Pts',(-0.0121851607319519,-0.0314448538103778,
-0.0136866321919951));
#21607=CARTESIAN_POINT('Ctrl Pts',(-0.0122116190984518,-0.0314434172474533,
-0.0136919050659516));
#21608=CARTESIAN_POINT('Ctrl Pts',(-0.0122757551059123,-0.0314399006285472,
-0.0137029470427694));
#21609=CARTESIAN_POINT('Ctrl Pts',(-0.0123135335768134,-0.0314378006839648,
-0.0137080187715643));
#21610=CARTESIAN_POINT('Ctrl Pts',(-0.012457617621782,-0.0314296992537254,
-0.0137219541182271));
#21611=CARTESIAN_POINT('Ctrl Pts',(-0.0125645521885388,-0.0314234725606537,
-0.0137211863448015));
#21612=CARTESIAN_POINT('Ctrl Pts',(-0.0127197598683049,-0.0314146025089491,
-0.0137039263207496));
#21613=CARTESIAN_POINT('Ctrl Pts',(-0.0127686924796418,-0.0314118358566056,
-0.0136960857583644));
#21614=CARTESIAN_POINT('Ctrl Pts',(-0.0128269234237763,-0.031408643907022,
-0.0136838550991895));
#21615=CARTESIAN_POINT('Ctrl Pts',(-0.0128366602484997,-0.0314081136287711,
-0.0136817112742818));
#21616=CARTESIAN_POINT('Ctrl Pts',(-0.0128518354416466,-0.0314072933158411,
-0.0136782154968239));
#21617=CARTESIAN_POINT('Ctrl Pts',(-0.0128572882227633,-0.0314069998045459,
-0.0136769280737221));
#21618=CARTESIAN_POINT('Ctrl Pts',(-0.012866944239757,-0.0314064824055297,
-0.0136745926529453));
#21619=CARTESIAN_POINT('Ctrl Pts',(-0.0128711501188199,-0.0314062578524647,
-0.0136735566461199));
#21620=CARTESIAN_POINT('Ctrl Pts',(-0.0128812487181822,-0.0314057205870529,
-0.0136710239713124));
#21621=CARTESIAN_POINT('Ctrl Pts',(-0.0128871370070363,-0.0314054088625491,
-0.0136695101754966));
#21622=CARTESIAN_POINT('Ctrl Pts',(-0.0129051965450461,-0.0314044571203294,
-0.0136647533541457));
#21623=CARTESIAN_POINT('Ctrl Pts',(-0.0129173374299002,-0.0314038233447224,
-0.0136613959955447));
#21624=CARTESIAN_POINT('Ctrl Pts',(-0.0129457587835721,-0.0314023510811008,
-0.013653160601575));
#21625=CARTESIAN_POINT('Ctrl Pts',(-0.0129620026687948,-0.0314015184722565,
-0.0136481614638394));
#21626=CARTESIAN_POINT('Ctrl Pts',(-0.0130206555641337,-0.0313985335677542,
-0.0136290443927013));
#21627=CARTESIAN_POINT('Ctrl Pts',(-0.0130625305068071,-0.0313964432331087,
-0.0136133533619526));
#21628=CARTESIAN_POINT('Ctrl Pts',(-0.0131982379464647,-0.0313896356981413,
-0.013555662234645));
#21629=CARTESIAN_POINT('Ctrl Pts',(-0.0132885534290213,-0.0313850331117796,
-0.0135061135931963));
#21630=CARTESIAN_POINT('Ctrl Pts',(-0.0134112576859686,-0.0313779840296989,
-0.0134218794208967));
#21631=CARTESIAN_POINT('Ctrl Pts',(-0.013448052116485,-0.0313757558167005,
-0.0133941177908969));
#21632=CARTESIAN_POINT('Ctrl Pts',(-0.0134947858151831,-0.0313727377552565,
-0.0133554561483445));
#21633=CARTESIAN_POINT('Ctrl Pts',(-0.0135058912837954,-0.0313720058249217,
-0.0133460004723073));
#21634=CARTESIAN_POINT('Ctrl Pts',(-0.013523807265752,-0.0313707998273471,
-0.0133303024977436));
#21635=CARTESIAN_POINT('Ctrl Pts',(-0.013530698836923,-0.0313703296649524,
-0.0133241538575348));
#21636=CARTESIAN_POINT('Ctrl Pts',(-0.0135439403209284,-0.0313694138634025,
-0.0133121246016416));
#21637=CARTESIAN_POINT('Ctrl Pts',(-0.0135502967841283,-0.0313689685601055,
-0.0133062516925681));
#21638=CARTESIAN_POINT('Ctrl Pts',(-0.0135650762338339,-0.0313679196056958,
-0.0132923642757343));
#21639=CARTESIAN_POINT('Ctrl Pts',(-0.013573458629085,-0.0313673141332777,
-0.0132843074960202));
#21640=CARTESIAN_POINT('Ctrl Pts',(-0.013600853366855,-0.0313652997611933,
-0.0132573747199841));
#21641=CARTESIAN_POINT('Ctrl Pts',(-0.0136194644230901,-0.0313638733011536,
-0.0132380990352257));
#21642=CARTESIAN_POINT('Ctrl Pts',(-0.0136630699305331,-0.0313603867760978,
-0.0131905170504403));
#21643=CARTESIAN_POINT('Ctrl Pts',(-0.0136875447775516,-0.031358307270234,
-0.0131617596279088));
#21644=CARTESIAN_POINT('Ctrl Pts',(-0.0138019066580386,-0.0313479849574463,
-0.0130169432312744));
#21645=CARTESIAN_POINT('Ctrl Pts',(-0.0138759629044949,-0.0313392533197594,
-0.0128893755103561));
#21646=CARTESIAN_POINT('Ctrl Pts',(-0.0139370121809736,-0.0313303600388513,
-0.0127380926822364));
#21647=CARTESIAN_POINT('Ctrl Pts',(-0.0139428982562188,-0.0313294780530571,
-0.0127228101499231));
#21648=CARTESIAN_POINT('Ctrl Pts',(-0.0139509387763527,-0.031328239789845,
-0.0127009000863227));
#21649=CARTESIAN_POINT('Ctrl Pts',(-0.0139532931812631,-0.031327872779829,
-0.0126943476525835));
#21650=CARTESIAN_POINT('Ctrl Pts',(-0.0139572136048589,-0.0313272542821306,
-0.0126832003773575));
#21651=CARTESIAN_POINT('Ctrl Pts',(-0.0139588024282121,-0.0313270014754814,
-0.0126786137051423));
#21652=CARTESIAN_POINT('Ctrl Pts',(-0.0139620753876551,-0.0313264762451874,
-0.012669019054479));
#21653=CARTESIAN_POINT('Ctrl Pts',(-0.0139637554792521,-0.0313262040545563,
-0.012664009831563));
#21654=CARTESIAN_POINT('Ctrl Pts',(-0.0139681582703751,-0.0313254835558807,
-0.0126506557095259));
#21655=CARTESIAN_POINT('Ctrl Pts',(-0.0139708355850721,-0.0313250378356614,
-0.0126422959264484));
#21656=CARTESIAN_POINT('Ctrl Pts',(-0.0139835680918285,-0.0313228780206909,
-0.0126013393005177));
#21657=CARTESIAN_POINT('Ctrl Pts',(-0.0139926123972976,-0.0313212164221712,
-0.0125684359760995));
#21658=CARTESIAN_POINT('Ctrl Pts',(-0.0140179558701629,-0.0313160286083413,
-0.0124626238067398));
#21659=CARTESIAN_POINT('Ctrl Pts',(-0.0140300569968736,-0.0313126382639009,
-0.0123888184736796));
#21660=CARTESIAN_POINT('Ctrl Pts',(-0.0140409219831004,-0.0313071059622067,
-0.0122683242487341));
#21661=CARTESIAN_POINT('Ctrl Pts',(-0.014043,-0.0313049845530144,-0.0122220872743005));
#21662=CARTESIAN_POINT('Ctrl Pts',(-0.014043,-0.0313028240247934,-0.012175853286558));
#21663=CARTESIAN_POINT('Ctrl Pts',(-0.014043,-0.0314187998055481,-0.0121758533148708));
#21664=CARTESIAN_POINT('Ctrl Pts',(-0.0140429999988588,-0.0314216855929924,
-0.0122380454537156));
#21665=CARTESIAN_POINT('Ctrl Pts',(-0.0140392399449419,-0.0314245042001014,
-0.0123002077166543));
#21666=CARTESIAN_POINT('Ctrl Pts',(-0.0140208889864976,-0.0314314837974405,
-0.0124512110731899));
#21667=CARTESIAN_POINT('Ctrl Pts',(-0.014002275293269,-0.0314356780248151,
-0.012539297740629));
#21668=CARTESIAN_POINT('Ctrl Pts',(-0.0139712207534049,-0.0314409577605894,
-0.012641298972176));
#21669=CARTESIAN_POINT('Ctrl Pts',(-0.0139660757433579,-0.031441796146914,
-0.0126572596414093));
#21670=CARTESIAN_POINT('Ctrl Pts',(-0.0139575355393169,-0.0314431345853968,
-0.012682344994258));
#21671=CARTESIAN_POINT('Ctrl Pts',(-0.0139543122951916,-0.031443628940107,
-0.0126915270601004));
#21672=CARTESIAN_POINT('Ctrl Pts',(-0.0139480856770548,-0.0314445644024562,
-0.012708742027167));
#21673=CARTESIAN_POINT('Ctrl Pts',(-0.0139451017595287,-0.0314450048446786,
-0.0127167815984485));
#21674=CARTESIAN_POINT('Ctrl Pts',(-0.0139382198245729,-0.031446003506652,
-0.0127348601796778));
#21675=CARTESIAN_POINT('Ctrl Pts',(-0.0139342834387855,-0.0314465630044302,
-0.0127448840235487));
#21676=CARTESIAN_POINT('Ctrl Pts',(-0.0139220405319888,-0.0314482688950765,
-0.0127751257354399));
#21677=CARTESIAN_POINT('Ctrl Pts',(-0.0139134092916564,-0.0314494262159711,
-0.0127952084759897));
#21678=CARTESIAN_POINT('Ctrl Pts',(-0.0138656667541817,-0.0314556027049977,
-0.0129000935037362));
#21679=CARTESIAN_POINT('Ctrl Pts',(-0.0138193481733023,-0.0314608691567798,
-0.0129813877187382));
#21680=CARTESIAN_POINT('Ctrl Pts',(-0.013706683963106,-0.0314721789603007,
-0.0131430750946339));
#21681=CARTESIAN_POINT('Ctrl Pts',(-0.0136389643303889,-0.0314782151913641,
-0.0132219731957544));
#21682=CARTESIAN_POINT('Ctrl Pts',(-0.0135543627053837,-0.0314845312773765,
-0.0133025029334424));
#21683=CARTESIAN_POINT('Ctrl Pts',(-0.0135447724057623,-0.0314852313616164,
-0.0133114019573471));
#21684=CARTESIAN_POINT('Ctrl Pts',(-0.0135304805762694,-0.0314862499360126,
-0.0133243292653996));
#21685=CARTESIAN_POINT('Ctrl Pts',(-0.013525866360791,-0.0314865750786379,
-0.0133284527418921));
#21686=CARTESIAN_POINT('Ctrl Pts',(-0.0135179594372508,-0.031487125754598,
-0.0133354336365533));
#21687=CARTESIAN_POINT('Ctrl Pts',(-0.0135146792651424,-0.0314873523150126,
-0.0133383050035641));
#21688=CARTESIAN_POINT('Ctrl Pts',(-0.01350717894198,-0.0314878660443637,
-0.0133448146302843));
#21689=CARTESIAN_POINT('Ctrl Pts',(-0.0135029512197482,-0.0314881525584564,
-0.0133484439640745));
#21690=CARTESIAN_POINT('Ctrl Pts',(-0.0134912567842693,-0.0314889369990052,
-0.0133583736587378));
#21691=CARTESIAN_POINT('Ctrl Pts',(-0.013483749633373,-0.0314894315678469,
-0.0133646262300369));
#21692=CARTESIAN_POINT('Ctrl Pts',(-0.0134410412539979,-0.0314921980381885,
-0.0133995156181787));
#21693=CARTESIAN_POINT('Ctrl Pts',(-0.0134046468821151,-0.031494377009065,
-0.0134266621483671));
#21694=CARTESIAN_POINT('Ctrl Pts',(-0.0132853666425809,-0.0315011482257995,
-0.0135076991616854));
#21695=CARTESIAN_POINT('Ctrl Pts',(-0.0131984798373307,-0.0315055587226969,
-0.0135552522752469));
#21696=CARTESIAN_POINT('Ctrl Pts',(-0.0130448705970116,-0.0315133184102152,
-0.0136210619488648));
#21697=CARTESIAN_POINT('Ctrl Pts',(-0.0129803920588518,-0.0315165622782346,
-0.013643754580357));
#21698=CARTESIAN_POINT('Ctrl Pts',(-0.0128993289897697,-0.0315207376173863,
-0.0136663691636852));
#21699=CARTESIAN_POINT('Ctrl Pts',(-0.012883967019409,-0.0315215327998017,
-0.0136704002166832));
#21700=CARTESIAN_POINT('Ctrl Pts',(-0.0128592813512121,-0.0315228179743021,
-0.0136764721374574));
#21701=CARTESIAN_POINT('Ctrl Pts',(-0.0128499959959254,-0.0315233030360891,
-0.0136786649256138));
#21702=CARTESIAN_POINT('Ctrl Pts',(-0.0128322943177223,-0.0315242311219549,
-0.013682672321702));
#21703=CARTESIAN_POINT('Ctrl Pts',(-0.0128238819549973,-0.0315246736108308,
-0.0136845028792327));
#21704=CARTESIAN_POINT('Ctrl Pts',(-0.0128045985912559,-0.0315256913505688,
-0.0136885302834647));
#21705=CARTESIAN_POINT('Ctrl Pts',(-0.0127937184265435,-0.0315262680758019,
-0.0136906804965072));
#21706=CARTESIAN_POINT('Ctrl Pts',(-0.01276502335477,-0.0315277959497924,
-0.0136960306488351));
#21707=CARTESIAN_POINT('Ctrl Pts',(-0.0127471740453338,-0.0315287532568627,
-0.0136990346759671));
#21708=CARTESIAN_POINT('Ctrl Pts',(-0.0126055737809395,-0.0315364040525736,
-0.0137203114565959));
#21709=CARTESIAN_POINT('Ctrl Pts',(-0.0124800872303128,-0.0315435797212047,
-0.013723784297865));
#21710=CARTESIAN_POINT('Ctrl Pts',(-0.0122769806300937,-0.0315553065791207,
-0.0137046909230675));
#21711=CARTESIAN_POINT('Ctrl Pts',(-0.0121990524657633,-0.0315598178928486,
-0.0136912789580564));
#21712=CARTESIAN_POINT('Ctrl Pts',(-0.0121122597943697,-0.0315646262399087,
-0.013669378581585));
#21713=CARTESIAN_POINT('Ctrl Pts',(-0.0121020581902953,-0.0315651878494193,
-0.0136666928493729));
#21714=CARTESIAN_POINT('Ctrl Pts',(-0.0120864060407903,-0.0315660431511267,
-0.0136624000601014));
#21715=CARTESIAN_POINT('Ctrl Pts',(-0.0120809356730253,-0.0315663408723307,
-0.0136608672140737));
#21716=CARTESIAN_POINT('Ctrl Pts',(-0.0120708318770773,-0.0315668883691417,
-0.0136579757627627));
#21717=CARTESIAN_POINT('Ctrl Pts',(-0.0120661963298796,-0.0315671386014761,
-0.0136566256149808));
#21718=CARTESIAN_POINT('Ctrl Pts',(-0.0120556232049555,-0.0315677072362739,
-0.0136534921787438));
#21719=CARTESIAN_POINT('Ctrl Pts',(-0.0120496899720474,-0.0315680248214863,
-0.0136516948474849));
#21720=CARTESIAN_POINT('Ctrl Pts',(-0.0120308744763391,-0.0315690276065104,
-0.013645871110256));
#21721=CARTESIAN_POINT('Ctrl Pts',(-0.0120180338164882,-0.0315697054688908,
-0.0136417113220724));
#21722=CARTESIAN_POINT('Ctrl Pts',(-0.011909283972561,-0.0315754038128945,
-0.0136048977846261));
#21723=CARTESIAN_POINT('Ctrl Pts',(-0.0118167405790377,-0.0315799811809506,
-0.0135630356141383));
#21724=CARTESIAN_POINT('Ctrl Pts',(-0.0116507180950171,-0.0315887461816521,
-0.0134672590627352));
#21725=CARTESIAN_POINT('Ctrl Pts',(-0.0115765930058636,-0.031592907270975,
-0.0134153396254213));
#21726=CARTESIAN_POINT('Ctrl Pts',(-0.0114882928262972,-0.0315985317671662,
-0.0133411528032266));
#21727=CARTESIAN_POINT('Ctrl Pts',(-0.0114695407594927,-0.0315997681887071,
-0.0133246039272904));
#21728=CARTESIAN_POINT('Ctrl Pts',(-0.0114428755826538,-0.0316015932368798,
-0.013299893216345));
#21729=CARTESIAN_POINT('Ctrl Pts',(-0.0114346369432065,-0.0316021667873117,
-0.0132920877358709));
#21730=CARTESIAN_POINT('Ctrl Pts',(-0.0114202772051401,-0.0316031840721613,
-0.0132781791835554));
#21731=CARTESIAN_POINT('Ctrl Pts',(-0.011414119831395,-0.0316036261341294,
-0.0132721141826644));
#21732=CARTESIAN_POINT('Ctrl Pts',(-0.0114013635139283,-0.0316045544583557,
-0.013259336315536));
#21733=CARTESIAN_POINT('Ctrl Pts',(-0.0113947744096335,-0.0316050411283271,
-0.0132526141661086));
#21734=CARTESIAN_POINT('Ctrl Pts',(-0.0113776456897686,-0.0316063254153682,
-0.0132348167131437));
#21735=CARTESIAN_POINT('Ctrl Pts',(-0.0113672086351464,-0.0316071274270104,
-0.013223644505026));
#21736=CARTESIAN_POINT('Ctrl Pts',(-0.0113222320731733,-0.0316106710319972,
-0.0131740423693049));
#21737=CARTESIAN_POINT('Ctrl Pts',(-0.011289472193382,-0.0316134855826697,
-0.0131340496840499));
#21738=CARTESIAN_POINT('Ctrl Pts',(-0.0112006689691173,-0.0316218155595446,
-0.0130138015137302));
#21739=CARTESIAN_POINT('Ctrl Pts',(-0.0111501738805981,-0.0316274929481046,
-0.0129297664808525));
#21740=CARTESIAN_POINT('Ctrl Pts',(-0.0110828562279666,-0.031636423064715,
-0.0127889953812587));
#21741=CARTESIAN_POINT('Ctrl Pts',(-0.0110607267242149,-0.0316397154109402,
-0.0127350788423439));
#21742=CARTESIAN_POINT('Ctrl Pts',(-0.0110372773487158,-0.0316436002356902,
-0.0126672537134824));
#21743=CARTESIAN_POINT('Ctrl Pts',(-0.011033025996539,-0.0316443246282052,
-0.0126544128249562));
#21744=CARTESIAN_POINT('Ctrl Pts',(-0.011027051346591,-0.0316453714782436,
-0.0126355386036348));
#21745=CARTESIAN_POINT('Ctrl Pts',(-0.0110251952250376,-0.0316457011070212,
-0.0126295483435721));
#21746=CARTESIAN_POINT('Ctrl Pts',(-0.0110219755849809,-0.0316462806238918,
-0.012618929028264));
#21747=CARTESIAN_POINT('Ctrl Pts',(-0.0110205971952142,-0.0316465313568009,
-0.0126143046833669));
#21748=CARTESIAN_POINT('Ctrl Pts',(-0.011017636666745,-0.031647075684922,
-0.0126041995107628));
#21749=CARTESIAN_POINT('Ctrl Pts',(-0.0110160632115682,-0.0316473687820653,
-0.0125987163253028));
#21750=CARTESIAN_POINT('Ctrl Pts',(-0.0110117176444677,-0.0316481894854295,
-0.0125832498706483));
#21751=CARTESIAN_POINT('Ctrl Pts',(-0.0110090155767339,-0.0316487132087248,
-0.0125732470549029));
#21752=CARTESIAN_POINT('Ctrl Pts',(-0.0109906081618817,-0.0316523842815274,
-0.0125022723833809));
#21753=CARTESIAN_POINT('Ctrl Pts',(-0.0109785454291245,-0.0316553510898768,
-0.0124404107412925));
#21754=CARTESIAN_POINT('Ctrl Pts',(-0.0109614573369846,-0.0316613814771096,
-0.0123110872576325));
#21755=CARTESIAN_POINT('Ctrl Pts',(-0.0109570156799674,-0.0316644317685996,
-0.0122436865241268));
#21756=CARTESIAN_POINT('Ctrl Pts',(-0.0109569816722006,-0.0316711948049043,
-0.0120969527910919));
#21757=CARTESIAN_POINT('Ctrl Pts',(-0.010963070016228,-0.0316749233671426,
-0.0120178175974637));
#21758=CARTESIAN_POINT('Ctrl Pts',(-0.0109777527841392,-0.0316796695635056,
-0.0119230919205409));
#21759=CARTESIAN_POINT('Ctrl Pts',(-0.0109805618209704,-0.0316804998709306,
-0.0119067204429781));
#21760=CARTESIAN_POINT('Ctrl Pts',(-0.0109854459026682,-0.0316818329524735,
-0.0118807757495471));
#21761=CARTESIAN_POINT('Ctrl Pts',(-0.0109873487846232,-0.0316823302282132,
-0.0118711712204072));
#21762=CARTESIAN_POINT('Ctrl Pts',(-0.0109910713672093,-0.0316832640090688,
-0.0118532770942604));
#21763=CARTESIAN_POINT('Ctrl Pts',(-0.0109928683066127,-0.031683699766836,
-0.0118449831101408));
#21764=CARTESIAN_POINT('Ctrl Pts',(-0.0109970722828062,-0.0316846868900492,
-0.0118263243261713));
#21765=CARTESIAN_POINT('Ctrl Pts',(-0.0109995182829033,-0.0316852394964143,
-0.0118159688241762));
#21766=CARTESIAN_POINT('Ctrl Pts',(-0.0110071560672459,-0.031686903189005,
-0.011785065433712));
#21767=CARTESIAN_POINT('Ctrl Pts',(-0.0110126641422153,-0.0316880244259015,
-0.0117645989379319));
#21768=CARTESIAN_POINT('Ctrl Pts',(-0.0110410173594783,-0.0316934510274061,
-0.0116672804403995));
#21769=CARTESIAN_POINT('Ctrl Pts',(-0.0110694050539009,-0.0316979340238511,
-0.0115921821460593));
#21770=CARTESIAN_POINT('Ctrl Pts',(-0.0111399017405879,-0.0317074009861696,
-0.0114421569168597));
#21771=CARTESIAN_POINT('Ctrl Pts',(-0.01118269381291,-0.0317123820749236,
-0.0113678420665893));
#21772=CARTESIAN_POINT('Ctrl Pts',(-0.0112532272501905,-0.0317193527880609,
-0.0112659780185449));
#21773=CARTESIAN_POINT('Ctrl Pts',(-0.0112761921383354,-0.0317214701386228,
-0.0112353161852541));
#21774=CARTESIAN_POINT('Ctrl Pts',(-0.0113062256179998,-0.0317240272589316,
-0.0111981819475763));
#21775=CARTESIAN_POINT('Ctrl Pts',(-0.011312243238261,-0.0317245297064263,
-0.0111908799844202));
#21776=CARTESIAN_POINT('Ctrl Pts',(-0.0113218308849708,-0.0317253141558594,
-0.0111794616901454));
#21777=CARTESIAN_POINT('Ctrl Pts',(-0.0113253561033934,-0.0317255992391111,
-0.0111753082376082));
#21778=CARTESIAN_POINT('Ctrl Pts',(-0.01133207872757,-0.0317261364439579,
-0.0111674720663748));
#21779=CARTESIAN_POINT('Ctrl Pts',(-0.0113352716623891,-0.0317263888622535,
-0.0111637857573716));
#21780=CARTESIAN_POINT('Ctrl Pts',(-0.011342896161655,-0.0317269852962187,
-0.0111550669867109));
#21781=CARTESIAN_POINT('Ctrl Pts',(-0.0113473431960032,-0.0317273281753524,
-0.0111500481110629));
#21782=CARTESIAN_POINT('Ctrl Pts',(-0.0113625144457699,-0.0317284817601491,
-0.0111331492301612));
#21783=CARTESIAN_POINT('Ctrl Pts',(-0.0113733910411831,-0.0317292818058187,
-0.0111214067838658));
#21784=CARTESIAN_POINT('Ctrl Pts',(-0.0114005710316521,-0.0317312220403453,
-0.0110929638574415));
#21785=CARTESIAN_POINT('Ctrl Pts',(-0.0114170746473165,-0.0317323499411187,
-0.0110764596620695));
#21786=CARTESIAN_POINT('Ctrl Pts',(-0.0114897944134372,-0.0317371412862598,
-0.0110069644607968));
#21787=CARTESIAN_POINT('Ctrl Pts',(-0.0115495740244434,-0.0317406407346818,
-0.0109578597792837));
#21788=CARTESIAN_POINT('Ctrl Pts',(-0.0116880512975171,-0.0317483843806724,
-0.0108605389232706));
#21789=CARTESIAN_POINT('Ctrl Pts',(-0.0117678951791015,-0.0317526346948226,
-0.0108144815196708));
#21790=CARTESIAN_POINT('Ctrl Pts',(-0.0118712875394283,-0.0317582209022481,
-0.0107665797076639));
#21791=CARTESIAN_POINT('Ctrl Pts',(-0.0118914099420664,-0.0317593108955528,
-0.0107577737898283));
#21792=CARTESIAN_POINT('Ctrl Pts',(-0.0119216871275012,-0.0317609581386278,
-0.0107452870948034));
#21793=CARTESIAN_POINT('Ctrl Pts',(-0.0119317041149455,-0.0317615042593862,
-0.0107412783715227));
#21794=CARTESIAN_POINT('Ctrl Pts',(-0.011949758379731,-0.0317624909408469,
-0.0107342719574853));
#21795=CARTESIAN_POINT('Ctrl Pts',(-0.0119577802259509,-0.0317629301730841,
-0.0107312355926018));
#21796=CARTESIAN_POINT('Ctrl Pts',(-0.0119749439893212,-0.0317638718940798,
-0.0107249020033856));
#21797=CARTESIAN_POINT('Ctrl Pts',(-0.0119840925476679,-0.0317643750033485,
-0.0107216239596289));
#21798=CARTESIAN_POINT('Ctrl Pts',(-0.0120090515854803,-0.0317657509490294,
-0.0107129459846599));
#21799=CARTESIAN_POINT('Ctrl Pts',(-0.0120249194718407,-0.0317666293757518,
-0.0107077161738364));
#21800=CARTESIAN_POINT('Ctrl Pts',(-0.0121246045041788,-0.0317721721395204,
-0.010676646821809));
#21801=CARTESIAN_POINT('Ctrl Pts',(-0.0122104013007253,-0.0317770630400579,
-0.0106577391190128));
#21802=CARTESIAN_POINT('Ctrl Pts',(-0.0123820202042009,-0.0317869496649744,
-0.0106350001679799));
#21803=CARTESIAN_POINT('Ctrl Pts',(-0.0124674965099922,-0.0317919203460436,
-0.0106308318749435));
#21804=CARTESIAN_POINT('Ctrl Pts',(-0.0125913970206836,-0.0317988969046917,
-0.0106350804242895));
#21805=CARTESIAN_POINT('Ctrl Pts',(-0.0126298556022816,-0.0318010285394772,
-0.0106378440581973));
#21806=CARTESIAN_POINT('Ctrl Pts',(-0.0126775947549223,-0.0318036000286029,
-0.0106430783709083));
#21807=CARTESIAN_POINT('Ctrl Pts',(-0.0126870071505291,-0.0318041033853816,
-0.0106441982426557));
#21808=CARTESIAN_POINT('Ctrl Pts',(-0.0127018158172239,-0.0318048889279331,
-0.0106460987008032));
#21809=CARTESIAN_POINT('Ctrl Pts',(-0.0127072191454741,-0.0318051742088032,
-0.0106468212580266));
#21810=CARTESIAN_POINT('Ctrl Pts',(-0.0127174478545807,-0.0318057115568389,
-0.0106482443040263));
#21811=CARTESIAN_POINT('Ctrl Pts',(-0.0127222738468022,-0.0318059639233734,
-0.0106489390419921));
#21812=CARTESIAN_POINT('Ctrl Pts',(-0.0127337215038839,-0.0318065599275467,
-0.0106506424418905));
#21813=CARTESIAN_POINT('Ctrl Pts',(-0.0127403401075631,-0.0318069024333957,
-0.0106516713755119));
#21814=CARTESIAN_POINT('Ctrl Pts',(-0.0127627051048666,-0.031808053377305,
-0.0106552975609974));
#21815=CARTESIAN_POINT('Ctrl Pts',(-0.0127784183023889,-0.031808851221472,
-0.010658096068466));
#21816=CARTESIAN_POINT('Ctrl Pts',(-0.0128169063445851,-0.0318107850220818,
-0.0106655686193845));
#21817=CARTESIAN_POINT('Ctrl Pts',(-0.012839624779767,-0.0318119087968367,
-0.0106705146189658));
#21818=CARTESIAN_POINT('Ctrl Pts',(-0.0129367571694401,-0.0318166695232632,
-0.0106939722459075));
#21819=CARTESIAN_POINT('Ctrl Pts',(-0.013009849350703,-0.031820144561209,
-0.0107175038186367));
#21820=CARTESIAN_POINT('Ctrl Pts',(-0.0131668980918235,-0.0318278993658513,
-0.0107813231004393));
#21821=CARTESIAN_POINT('Ctrl Pts',(-0.0132495690237774,-0.0318321861072869,
-0.0108239613746075));
#21822=CARTESIAN_POINT('Ctrl Pts',(-0.0133463750261516,-0.0318378106396406,
-0.0108855131817872));
#21823=CARTESIAN_POINT('Ctrl Pts',(-0.0133645964665641,-0.0318388972158917,
-0.01089765097047));
#21824=CARTESIAN_POINT('Ctrl Pts',(-0.013391391948244,-0.0318405402915505,
-0.0109163353195115));
#21825=CARTESIAN_POINT('Ctrl Pts',(-0.013400165969161,-0.0318410857470344,
-0.0109225910095268));
#21826=CARTESIAN_POINT('Ctrl Pts',(-0.0134158039776208,-0.0318420717059085,
-0.0109339895168248));
#21827=CARTESIAN_POINT('Ctrl Pts',(-0.013422692017339,-0.0318425108891388,
-0.0109390986685371));
#21828=CARTESIAN_POINT('Ctrl Pts',(-0.0134373008046071,-0.0318434530307015,
-0.0109501245995892));
#21829=CARTESIAN_POINT('Ctrl Pts',(-0.0134450088862328,-0.031843956615434,
-0.0109560574792675));
#21830=CARTESIAN_POINT('Ctrl Pts',(-0.0134658350799753,-0.0318453352274491,
-0.0109724032046639));
#21831=CARTESIAN_POINT('Ctrl Pts',(-0.0134788403150553,-0.0318462158815942,
-0.0109829571850283));
#21832=CARTESIAN_POINT('Ctrl Pts',(-0.0135599560775883,-0.0318518367961169,
-0.0110510038017946));
#21833=CARTESIAN_POINT('Ctrl Pts',(-0.0136231399884212,-0.0318568115473902,
-0.0111140878365509));
#21834=CARTESIAN_POINT('Ctrl Pts',(-0.0137371225708579,-0.0318669267327057,
-0.0112495145873098));
#21835=CARTESIAN_POINT('Ctrl Pts',(-0.0137878748009157,-0.0318720434887797,
-0.0113214796170112));
#21836=CARTESIAN_POINT('Ctrl Pts',(-0.0138499070741362,-0.0318789373447697,
-0.0114276364890068));
#21837=CARTESIAN_POINT('Ctrl Pts',(-0.0138665555018071,-0.0318808691789927,
-0.0114584943213541));
#21838=CARTESIAN_POINT('Ctrl Pts',(-0.0138862393816572,-0.0318832380413681,
-0.0114981553964777));
#21839=CARTESIAN_POINT('Ctrl Pts',(-0.013890265281936,-0.031883727492543,
-0.0115064531763914));
#21840=CARTESIAN_POINT('Ctrl Pts',(-0.0138965281904415,-0.0318844963049612,
-0.0115196619091663));
#21841=CARTESIAN_POINT('Ctrl Pts',(-0.0138988141917251,-0.0318847785531938,
-0.0115245492337199));
#21842=CARTESIAN_POINT('Ctrl Pts',(-0.0139031249124826,-0.0318853137806134,
-0.0115338926690531));
#21843=CARTESIAN_POINT('Ctrl Pts',(-0.0139051541117647,-0.0318855670177228,
-0.0115383465204142));
#21844=CARTESIAN_POINT('Ctrl Pts',(-0.0139099595100629,-0.0318861699647982,
-0.0115490282139574));
#21845=CARTESIAN_POINT('Ctrl Pts',(-0.013912715715472,-0.0318865184664609,
-0.0115552650154181));
#21846=CARTESIAN_POINT('Ctrl Pts',(-0.013922078927995,-0.031887712405295,
-0.0115768379581493));
#21847=CARTESIAN_POINT('Ctrl Pts',(-0.0139284784774628,-0.0318885461455529,
-0.0115922634278809));
#21848=CARTESIAN_POINT('Ctrl Pts',(-0.0139437284609508,-0.0318905856554026,
-0.0116307768201803));
#21849=CARTESIAN_POINT('Ctrl Pts',(-0.0139522769493644,-0.0318917774295723,
-0.0116539797495911));
#21850=CARTESIAN_POINT('Ctrl Pts',(-0.0139882901032485,-0.0318970719356118,
-0.0117594791351609));
#21851=CARTESIAN_POINT('Ctrl Pts',(-0.0140093433701723,-0.0319009749002342,
-0.0118438004972352));
#21852=CARTESIAN_POINT('Ctrl Pts',(-0.0140363806581955,-0.0319087461953,
-0.0120109363637244));
#21853=CARTESIAN_POINT('Ctrl Pts',(-0.0140430000004134,-0.031912595402268,
-0.0120933357057804));
#21854=CARTESIAN_POINT('Ctrl Pts',(-0.014043,-0.0319166517728185,-0.012175853294288));
#21855=CARTESIAN_POINT('Origin',(-0.0125,-0.0375520664398416,-0.0121758532865581));
#21856=CARTESIAN_POINT('',(-0.014043,-0.0324174341340783,-0.0121758532914128));
#21857=CARTESIAN_POINT('',(-0.014043,-0.0323021764224865,-0.0121758532515513));
#21858=CARTESIAN_POINT('',(-0.014043,-0.0375520664398416,-0.012175853286558));
#21859=CARTESIAN_POINT('Ctrl Pts',(-0.014043,-0.0323021764244909,-0.0121758532514363));
#21860=CARTESIAN_POINT('Ctrl Pts',(-0.0140429999996933,-0.0323014024090168,
-0.0121623792514412));
#21861=CARTESIAN_POINT('Ctrl Pts',(-0.0140428235103971,-0.0323006271566412,
-0.0121489018304193));
#21862=CARTESIAN_POINT('Ctrl Pts',(-0.0140408270881201,-0.0322962438293193,
-0.0120727329270992));
#21863=CARTESIAN_POINT('Ctrl Pts',(-0.0140353633656632,-0.032292635035969,
-0.0120101972794149));
#21864=CARTESIAN_POINT('Ctrl Pts',(-0.0140230358114081,-0.0322879765861664,
-0.0119275701132655));
#21865=CARTESIAN_POINT('Ctrl Pts',(-0.0140195463323506,-0.0322868284354249,
-0.0119070380506838));
#21866=CARTESIAN_POINT('Ctrl Pts',(-0.0140128878450054,-0.032284900661059,
-0.0118721507694607));
#21867=CARTESIAN_POINT('Ctrl Pts',(-0.0140099274416961,-0.0322841121881339,
-0.0118577589574257));
#21868=CARTESIAN_POINT('Ctrl Pts',(-0.0140053688660552,-0.0322829922003959,
-0.0118370976558387));
#21869=CARTESIAN_POINT('Ctrl Pts',(-0.0140039362113176,-0.032282652052595,
-0.0118307928926249));
#21870=CARTESIAN_POINT('Ctrl Pts',(-0.0140013647676637,-0.0322820618640116,
-0.0118197969211683));
#21871=CARTESIAN_POINT('Ctrl Pts',(-0.0140002435303095,-0.0322818108450363,
-0.0118151017753191));
#21872=CARTESIAN_POINT('Ctrl Pts',(-0.013997789552853,-0.0322812748217816,
-0.01180503516218));
#21873=CARTESIAN_POINT('Ctrl Pts',(-0.0139964499356728,-0.0322809902103484,
-0.0117996655436832));
#21874=CARTESIAN_POINT('Ctrl Pts',(-0.0139926912207524,-0.0322802128617021,
-0.011784937242925));
#21875=CARTESIAN_POINT('Ctrl Pts',(-0.0139902129889699,-0.0322797234015583,
-0.0117755937579562));
#21876=CARTESIAN_POINT('Ctrl Pts',(-0.0139760053679398,-0.0322770374793962,
-0.0117239897731068));
#21877=CARTESIAN_POINT('Ctrl Pts',(-0.013962565230283,-0.032274927781438,
-0.0116822177737148));
#21878=CARTESIAN_POINT('Ctrl Pts',(-0.0139190434010339,-0.0322690209717205,
-0.0115644277510888));
#21879=CARTESIAN_POINT('Ctrl Pts',(-0.0138846801153873,-0.0322653423961703,
-0.0114901511835274));
#21880=CARTESIAN_POINT('Ctrl Pts',(-0.0138061657954547,-0.0322579859731393,
-0.011350676282501));
#21881=CARTESIAN_POINT('Ctrl Pts',(-0.0137625961580761,-0.0322543240921222,
-0.0112854401602769));
#21882=CARTESIAN_POINT('Ctrl Pts',(-0.0137013501291463,-0.0322494488460696,
-0.0112073260525811));
#21883=CARTESIAN_POINT('Ctrl Pts',(-0.0136881015250762,-0.0322484086226143,
-0.0111911188811897));
#21884=CARTESIAN_POINT('Ctrl Pts',(-0.0136676780585777,-0.0322468235214271,
-0.0111671469333451));
#21885=CARTESIAN_POINT('Ctrl Pts',(-0.013660746145708,-0.0322462885816627,
-0.0111591778548133));
#21886=CARTESIAN_POINT('Ctrl Pts',(-0.0136480718860771,-0.0322453156526887,
-0.0111449058425988));
#21887=CARTESIAN_POINT('Ctrl Pts',(-0.0136423580375394,-0.0322448788703348,
-0.0111385781070625));
#21888=CARTESIAN_POINT('Ctrl Pts',(-0.0136299642480799,-0.0322439352084256,
-0.0111250793635263));
#21889=CARTESIAN_POINT('Ctrl Pts',(-0.0136232678644398,-0.0322434276324282,
-0.0111179240176503));
#21890=CARTESIAN_POINT('Ctrl Pts',(-0.013604933054889,-0.0322420437799935,
-0.0110987028936592));
#21891=CARTESIAN_POINT('Ctrl Pts',(-0.0135931656490724,-0.032241161906209,
-0.011086762446262));
#21892=CARTESIAN_POINT('Ctrl Pts',(-0.0135145892371655,-0.0322353122326807,
-0.0110095872392964));
#21893=CARTESIAN_POINT('Ctrl Pts',(-0.0134421802690433,-0.0322300853874455,
-0.0109503494476973));
#21894=CARTESIAN_POINT('Ctrl Pts',(-0.0132962289054131,-0.0322199963196308,
-0.0108515651732669));
#21895=CARTESIAN_POINT('Ctrl Pts',(-0.0132239530049224,-0.0322151795230815,
-0.010810711575507));
#21896=CARTESIAN_POINT('Ctrl Pts',(-0.0131268248095656,-0.0322091751821878,
-0.0107657031799728));
#21897=CARTESIAN_POINT('Ctrl Pts',(-0.0131046682162367,-0.0322078358229432,
-0.0107560613594998));
#21898=CARTESIAN_POINT('Ctrl Pts',(-0.0130671014424623,-0.0322056259069295,
-0.0107407525663575));
#21899=CARTESIAN_POINT('Ctrl Pts',(-0.0130518110852945,-0.0322047430254511,
-0.0107348041230554));
#21900=CARTESIAN_POINT('Ctrl Pts',(-0.0130300954901301,-0.0322035153834349,
-0.0107267523971341));
#21901=CARTESIAN_POINT('Ctrl Pts',(-0.0130237473259522,-0.0322031596364759,
-0.0107244459149776));
#21902=CARTESIAN_POINT('Ctrl Pts',(-0.0130127983454962,-0.0322025516975174,
-0.010720549005675));
#21903=CARTESIAN_POINT('Ctrl Pts',(-0.0130082048110785,-0.0322022983446181,
-0.0107189385445465));
#21904=CARTESIAN_POINT('Ctrl Pts',(-0.0129985127033996,-0.0322017674475736,
-0.0107155919772538));
#21905=CARTESIAN_POINT('Ctrl Pts',(-0.0129934125866443,-0.0322014901870418,
-0.0107138608009521));
#21906=CARTESIAN_POINT('Ctrl Pts',(-0.0129795343760125,-0.0322007411634398,
-0.0107092308958848));
#21907=CARTESIAN_POINT('Ctrl Pts',(-0.0129707389993778,-0.0322002723613871,
-0.0107063842473956));
#21908=CARTESIAN_POINT('Ctrl Pts',(-0.0129279224990572,-0.032198016373534,
-0.0106929504496126));
#21909=CARTESIAN_POINT('Ctrl Pts',(-0.0128935650285831,-0.0321962858672358,
-0.010683464129016));
#21910=CARTESIAN_POINT('Ctrl Pts',(-0.0127737697465406,-0.0321904305936913,
-0.0106548134393784));
#21911=CARTESIAN_POINT('Ctrl Pts',(-0.0126870491266767,-0.0321864932091093,
-0.0106417325660733));
#21912=CARTESIAN_POINT('Ctrl Pts',(-0.0125109318388377,-0.0321783922995229,
-0.0106303309326174));
#21913=CARTESIAN_POINT('Ctrl Pts',(-0.012421856794486,-0.0321742379998419,
-0.0106322697170178));
#21914=CARTESIAN_POINT('Ctrl Pts',(-0.0123168511923568,-0.0321690070947061,
-0.0106436704194866));
#21915=CARTESIAN_POINT('Ctrl Pts',(-0.0123002815129674,-0.032168172158224,
-0.0106457420741262));
#21916=CARTESIAN_POINT('Ctrl Pts',(-0.0122741546431794,-0.0321668392922129,
-0.0106494402451697));
#21917=CARTESIAN_POINT('Ctrl Pts',(-0.0122645733314575,-0.0321663470123645,
-0.0106508886390163));
#21918=CARTESIAN_POINT('Ctrl Pts',(-0.0122465765331201,-0.0321654155456725,
-0.0106537828389171));
#21919=CARTESIAN_POINT('Ctrl Pts',(-0.0122381581429432,-0.0321649770190096,
-0.0106552084433648));
#21920=CARTESIAN_POINT('Ctrl Pts',(-0.012219197687725,-0.0321639828298705,
-0.0106585813982888));
#21921=CARTESIAN_POINT('Ctrl Pts',(-0.0122086632869483,-0.0321634259017085,
-0.0106605688798174));
#21922=CARTESIAN_POINT('Ctrl Pts',(-0.0121775280171883,-0.0321617660248295,
-0.0106667797179403));
#21923=CARTESIAN_POINT('Ctrl Pts',(-0.0121569923994884,-0.0321606531911222,
-0.0106713145059951));
#21924=CARTESIAN_POINT('Ctrl Pts',(-0.012028020395348,-0.0321535475888209,
-0.0107025724913517));
#21925=CARTESIAN_POINT('Ctrl Pts',(-0.0119226761109214,-0.0321471850232166,
-0.0107405794132459));
#21926=CARTESIAN_POINT('Ctrl Pts',(-0.0117657791738965,-0.0321371385022699,
-0.0108172743186234));
#21927=CARTESIAN_POINT('Ctrl Pts',(-0.011710931187045,-0.0321335130317843,
-0.0108483789565857));
#21928=CARTESIAN_POINT('Ctrl Pts',(-0.0116406414486539,-0.0321288356149218,
-0.0108941404923349));
#21929=CARTESIAN_POINT('Ctrl Pts',(-0.0116233786649854,-0.0321276844641987,
-0.0109058848175271));
#21930=CARTESIAN_POINT('Ctrl Pts',(-0.0115943592308539,-0.0321257522141839,
-0.0109265012690223));
#21931=CARTESIAN_POINT('Ctrl Pts',(-0.0115824817568368,-0.0321249622150257,
-0.0109351978263089));
#21932=CARTESIAN_POINT('Ctrl Pts',(-0.0115655649451977,-0.0321238404745172,
-0.0109479599722));
#21933=CARTESIAN_POINT('Ctrl Pts',(-0.0115604242233197,-0.0321235000641672,
-0.0109518891425114));
#21934=CARTESIAN_POINT('Ctrl Pts',(-0.0115514911714856,-0.0321229095813506,
-0.0109588063240946));
#21935=CARTESIAN_POINT('Ctrl Pts',(-0.0115476879231135,-0.0321226585276164,
-0.0109617799703976));
#21936=CARTESIAN_POINT('Ctrl Pts',(-0.0115395571341245,-0.0321221226115552,
-0.0109681989087729));
#21937=CARTESIAN_POINT('Ctrl Pts',(-0.0115352341138763,-0.0321218381400629,
-0.0109716496569232));
#21938=CARTESIAN_POINT('Ctrl Pts',(-0.0115234173981948,-0.0321210615560551,
-0.010981186548432));
#21939=CARTESIAN_POINT('Ctrl Pts',(-0.0115159620002614,-0.0321205727100189,
-0.0109873199814207));
#21940=CARTESIAN_POINT('Ctrl Pts',(-0.0114751411846417,-0.0321178992648421,
-0.0110215500197178));
#21941=CARTESIAN_POINT('Ctrl Pts',(-0.0114429186950757,-0.0321158004714033,
-0.0110509838181382));
#21942=CARTESIAN_POINT('Ctrl Pts',(-0.0113539269842558,-0.032109895319126,
-0.0111394800000965));
#21943=CARTESIAN_POINT('Ctrl Pts',(-0.0113005548730207,-0.0321062092793998,
-0.0112017458049318));
#21944=CARTESIAN_POINT('Ctrl Pts',(-0.0112062339021968,-0.0320988418406193,
-0.0113313608100745));
#21945=CARTESIAN_POINT('Ctrl Pts',(-0.0111649973353384,-0.0320951766149079,
-0.0113981871873302));
#21946=CARTESIAN_POINT('Ctrl Pts',(-0.0111194116557756,-0.0320902971958638,
-0.0114864598123865));
#21947=CARTESIAN_POINT('Ctrl Pts',(-0.011110182906361,-0.0320892565078004,
-0.0115052595706263));
#21948=CARTESIAN_POINT('Ctrl Pts',(-0.0110968787278661,-0.0320876708385675,
-0.0115338164565803));
#21949=CARTESIAN_POINT('Ctrl Pts',(-0.0110925161102953,-0.0320871358063374,
-0.0115434375306079));
#21950=CARTESIAN_POINT('Ctrl Pts',(-0.0110848116882396,-0.0320861627790461,
-0.0115609030997182));
#21951=CARTESIAN_POINT('Ctrl Pts',(-0.0110814354390259,-0.0320857259919911,
-0.0115687319868926));
#21952=CARTESIAN_POINT('Ctrl Pts',(-0.0110743187512896,-0.0320847823987675,
-0.0115856177494684));
#21953=CARTESIAN_POINT('Ctrl Pts',(-0.0110705993703399,-0.032084274897052,
-0.0115946830480476));
#21954=CARTESIAN_POINT('Ctrl Pts',(-0.0110607537182774,-0.0320828914462587,
-0.0116193463606848));
#21955=CARTESIAN_POINT('Ctrl Pts',(-0.011054794920006,-0.0320820099052575,
-0.0116350094414325));
#21956=CARTESIAN_POINT('Ctrl Pts',(-0.0110177761448494,-0.0320762323051437,
-0.0117372987639338));
#21957=CARTESIAN_POINT('Ctrl Pts',(-0.0109942680790685,-0.0320710852195581,
-0.0118264470815429));
#21958=CARTESIAN_POINT('Ctrl Pts',(-0.0109647616807814,-0.0320610157007253,
-0.0119999402523358));
#21959=CARTESIAN_POINT('Ctrl Pts',(-0.0109574635849771,-0.032056133265962,
-0.0120837456160181));
#21960=CARTESIAN_POINT('Ctrl Pts',(-0.0109568933609971,-0.0320500572486341,
-0.0121920443636418));
#21961=CARTESIAN_POINT('Ctrl Pts',(-0.0109573401127474,-0.0320487088891805,
-0.0122163604111844));
#21962=CARTESIAN_POINT('Ctrl Pts',(-0.0109590536773698,-0.0320464858426147,
-0.0122571251699337));
#21963=CARTESIAN_POINT('Ctrl Pts',(-0.0109600098025389,-0.032045598654852,
-0.0122735821097014));
#21964=CARTESIAN_POINT('Ctrl Pts',(-0.0109617301546598,-0.0320443661384221,
-0.0122967692483317));
#21965=CARTESIAN_POINT('Ctrl Pts',(-0.0109622752140964,-0.0320440097099208,
-0.0123035140599565));
#21966=CARTESIAN_POINT('Ctrl Pts',(-0.0109632887936613,-0.0320434009845412,
-0.012315106224637));
#21967=CARTESIAN_POINT('Ctrl Pts',(-0.0109637359201621,-0.032043147518766,
-0.0123199553054482));
#21968=CARTESIAN_POINT('Ctrl Pts',(-0.0109647253659352,-0.0320426167946495,
-0.0123301573491021));
#21969=CARTESIAN_POINT('Ctrl Pts',(-0.0109652727324225,-0.0320423398155694,
-0.0123355096725717));
#21970=CARTESIAN_POINT('Ctrl Pts',(-0.0109668338688409,-0.0320415923790633,
-0.0123500244361822));
#21971=CARTESIAN_POINT('Ctrl Pts',(-0.010967901783508,-0.032041124861347,
-0.0123591809659832));
#21972=CARTESIAN_POINT('Ctrl Pts',(-0.0109734549035827,-0.0320388866200802,
-0.0124033507051559));
#21973=CARTESIAN_POINT('Ctrl Pts',(-0.0109790589215706,-0.0320371715013044,
-0.01243821482079));
#21974=CARTESIAN_POINT('Ctrl Pts',(-0.0110027495082845,-0.0320313180628234,
-0.0125589906133852));
#21975=CARTESIAN_POINT('Ctrl Pts',(-0.0110269641510058,-0.0320273702158028,
-0.0126435287443692));
#21976=CARTESIAN_POINT('Ctrl Pts',(-0.0110899706560847,-0.0320192526330271,
-0.0128087834626587));
#21977=CARTESIAN_POINT('Ctrl Pts',(-0.0111288488893611,-0.0320150923741797,
-0.0128891034036025));
#21978=CARTESIAN_POINT('Ctrl Pts',(-0.0111829827757266,-0.0320098545022367,
-0.0129799637173531));
#21979=CARTESIAN_POINT('Ctrl Pts',(-0.0111917635861749,-0.0320090193762505,
-0.0129941719360176));
#21980=CARTESIAN_POINT('Ctrl Pts',(-0.0112060009354054,-0.0320076862766123,
-0.0130163943831706));
#21981=CARTESIAN_POINT('Ctrl Pts',(-0.0112113054498348,-0.0320071939560945,
-0.0130245047256277));
#21982=CARTESIAN_POINT('Ctrl Pts',(-0.0112214264970593,-0.0320062624552239,
-0.013039665590713));
#21983=CARTESIAN_POINT('Ctrl Pts',(-0.0112262258540188,-0.0320058239356048,
-0.0130467271697072));
#21984=CARTESIAN_POINT('Ctrl Pts',(-0.0112371820506617,-0.0320048298206117,
-0.0130625633413006));
#21985=CARTESIAN_POINT('Ctrl Pts',(-0.0112433721724092,-0.0320042729603208,
-0.0130713142792607));
#21986=CARTESIAN_POINT('Ctrl Pts',(-0.0112623915357128,-0.0320025760020515,
-0.0130976162162919));
#21987=CARTESIAN_POINT('Ctrl Pts',(-0.011275500610095,-0.0320014250975602,
-0.0131149607290215));
#21988=CARTESIAN_POINT('Ctrl Pts',(-0.0113491114112831,-0.0319950598003242,
-0.0132081919729491));
#21989=CARTESIAN_POINT('Ctrl Pts',(-0.0114162954365855,-0.0319895757749732,
-0.0132785079835967));
#21990=CARTESIAN_POINT('Ctrl Pts',(-0.0115452768988058,-0.031979773896115,
-0.0133902561919174));
#21991=CARTESIAN_POINT('Ctrl Pts',(-0.0116043083131546,-0.0319755120036411,
-0.0134344269360474));
#21992=CARTESIAN_POINT('Ctrl Pts',(-0.0116854032086831,-0.0319701192544387,
-0.0134865012690919));
#21993=CARTESIAN_POINT('Ctrl Pts',(-0.0117048071894857,-0.031968861450865,
-0.0134983639854986));
#21994=CARTESIAN_POINT('Ctrl Pts',(-0.0117380292250366,-0.0319667711180667,
-0.0135176787747676));
#21995=CARTESIAN_POINT('Ctrl Pts',(-0.0117517113655891,-0.0319659278084603,
-0.0135253566246823));
#21996=CARTESIAN_POINT('Ctrl Pts',(-0.0117713445580545,-0.0319647451036616,
-0.0135359835309754));
#21997=CARTESIAN_POINT('Ctrl Pts',(-0.011777200816211,-0.031964395739545,
-0.0135391046859483));
#21998=CARTESIAN_POINT('Ctrl Pts',(-0.0117873716285336,-0.0319637951248527,
-0.0135444413635362));
#21999=CARTESIAN_POINT('Ctrl Pts',(-0.0117916767836761,-0.0319635427881837,
-0.0135466744797905));
#22000=CARTESIAN_POINT('Ctrl Pts',(-0.0118008351341862,-0.0319630100786934,
-0.0135513703188797));
#22001=CARTESIAN_POINT('Ctrl Pts',(-0.0118056908919372,-0.03196273003183,
-0.013553827698524));
#22002=CARTESIAN_POINT('Ctrl Pts',(-0.0118190602724995,-0.0319619652660586,
-0.0135605050023124));
#22003=CARTESIAN_POINT('Ctrl Pts',(-0.0118276001633642,-0.0319614837230102,
-0.0135646721209505));
#22004=CARTESIAN_POINT('Ctrl Pts',(-0.0118716424635831,-0.0319590331655217,
-0.013585661491315));
#22005=CARTESIAN_POINT('Ctrl Pts',(-0.0119077418968354,-0.0319571333865021,
-0.0136012034711843));
#22006=CARTESIAN_POINT('Ctrl Pts',(-0.0120236538055205,-0.0319512561800969,
-0.0136459419296564));
#22007=CARTESIAN_POINT('Ctrl Pts',(-0.0121053042773844,-0.0319474337372591,
-0.0136699359365906));
#22008=CARTESIAN_POINT('Ctrl Pts',(-0.0122741850631011,-0.0319395143527983,
-0.0137047441389993));
#22009=CARTESIAN_POINT('Ctrl Pts',(-0.0123611914895947,-0.0319354237535049,
-0.0137150834938936));
#22010=CARTESIAN_POINT('Ctrl Pts',(-0.0124652440825787,-0.0319302672733225,
-0.0137185517071799));
#22011=CARTESIAN_POINT('Ctrl Pts',(-0.012481897348991,-0.0319294344280181,
-0.0137188369733155));
#22012=CARTESIAN_POINT('Ctrl Pts',(-0.0125082324792094,-0.0319281041401937,
-0.0137188616942558));
#22013=CARTESIAN_POINT('Ctrl Pts',(-0.0125179131024213,-0.0319276123093079,
-0.0137187796733674));
#22014=CARTESIAN_POINT('Ctrl Pts',(-0.0125361302775812,-0.0319266812190894,
-0.0137184538588422));
#22015=CARTESIAN_POINT('Ctrl Pts',(-0.0125446668504504,-0.0319262426138277,
-0.0137182302803985));
#22016=CARTESIAN_POINT('Ctrl Pts',(-0.012563928827658,-0.0319252476018939,
-0.0137175657525926));
#22017=CARTESIAN_POINT('Ctrl Pts',(-0.0125746522955975,-0.0319246899210072,
-0.0137170837202814));
#22018=CARTESIAN_POINT('Ctrl Pts',(-0.0126064345943363,-0.0319230256569791,
-0.0137153226009946));
#22019=CARTESIAN_POINT('Ctrl Pts',(-0.0126274725934355,-0.031921909111367,
-0.0137137234928307));
#22020=CARTESIAN_POINT('Ctrl Pts',(-0.0127582702136378,-0.0319148721889959,
-0.0137010792155449));
#22021=CARTESIAN_POINT('Ctrl Pts',(-0.0128665996690467,-0.0319085921787821,
-0.0136787223706112));
#22022=CARTESIAN_POINT('Ctrl Pts',(-0.0130324786803932,-0.0318985703388443,
-0.0136254750177988));
#22023=CARTESIAN_POINT('Ctrl Pts',(-0.0130920834450007,-0.0318948885563024,
-0.0136021683154359));
#22024=CARTESIAN_POINT('Ctrl Pts',(-0.0131691645023182,-0.0318901471835159,
-0.0135663607653334));
#22025=CARTESIAN_POINT('Ctrl Pts',(-0.0131880741132712,-0.0318889859838773,
-0.0135571013694842));
#22026=CARTESIAN_POINT('Ctrl Pts',(-0.0132199560174419,-0.0318870387537765,
-0.0135406725924551));
#22027=CARTESIAN_POINT('Ctrl Pts',(-0.0132330250925264,-0.0318862436531303,
-0.0135336981415434));
#22028=CARTESIAN_POINT('Ctrl Pts',(-0.013251670079468,-0.0318851160569593,
-0.013523400378333));
#22029=CARTESIAN_POINT('Ctrl Pts',(-0.0132573282642186,-0.0318847747715767,
-0.0135202285972891));
#22030=CARTESIAN_POINT('Ctrl Pts',(-0.0132671643151485,-0.0318841833068554,
-0.0135146330441754));
#22031=CARTESIAN_POINT('Ctrl Pts',(-0.0132713510550923,-0.0318839321360027,
-0.013512225195068));
#22032=CARTESIAN_POINT('Ctrl Pts',(-0.0132803003765,-0.0318833965713724,
-0.013507022251915));
#22033=CARTESIAN_POINT('Ctrl Pts',(-0.0132850593136585,-0.0318831125617741,
-0.0135042212204468));
#22034=CARTESIAN_POINT('Ctrl Pts',(-0.0132980610852545,-0.03188233850035,
-0.013496474317329));
#22035=CARTESIAN_POINT('Ctrl Pts',(-0.0133062730271159,-0.031881851680172,
-0.0134914767955324));
#22036=CARTESIAN_POINT('Ctrl Pts',(-0.0133508280585645,-0.0318792187936029,
-0.0134637881742982));
#22037=CARTESIAN_POINT('Ctrl Pts',(-0.0133862633597354,-0.0318771554557466,
-0.0134396659599712));
#22038=CARTESIAN_POINT('Ctrl Pts',(-0.0134867964851076,-0.0318712556472463,
-0.0133649182943407));
#22039=CARTESIAN_POINT('Ctrl Pts',(-0.0135488972606294,-0.0318675453688137,
-0.013310515586894));
#22040=CARTESIAN_POINT('Ctrl Pts',(-0.0136611935207123,-0.0318601421039148,
-0.0131950036282095));
#22041=CARTESIAN_POINT('Ctrl Pts',(-0.0137116321733821,-0.0318564659579765,
-0.0131344896602007));
#22042=CARTESIAN_POINT('Ctrl Pts',(-0.0137693929830662,-0.0318515729131813,
-0.0130533100132674));
#22043=CARTESIAN_POINT('Ctrl Pts',(-0.0137812017001961,-0.0318505307102753,
-0.0130359759540137));
#22044=CARTESIAN_POINT('Ctrl Pts',(-0.0137984248661999,-0.0318489431890256,
-0.0130095520284163));
#22045=CARTESIAN_POINT('Ctrl Pts',(-0.0138041053777642,-0.0318484078554346,
-0.0130006380353296));
#22046=CARTESIAN_POINT('Ctrl Pts',(-0.0138142017696548,-0.0318474345075051,
-0.0129844294462429));
#22047=CARTESIAN_POINT('Ctrl Pts',(-0.0138186496473569,-0.0318469977049215,
-0.0129771552277894));
#22048=CARTESIAN_POINT('Ctrl Pts',(-0.0138280767564826,-0.0318460543346053,
-0.0129614467266122));
#22049=CARTESIAN_POINT('Ctrl Pts',(-0.0138330364100274,-0.0318455470742361,
-0.0129530011796582));
#22050=CARTESIAN_POINT('Ctrl Pts',(-0.0138462531932358,-0.0318441649282978,
-0.0129299961686877));
#22051=CARTESIAN_POINT('Ctrl Pts',(-0.0138543542076786,-0.0318432844684109,
-0.0129153489236433));
#22052=CARTESIAN_POINT('Ctrl Pts',(-0.0139061215541963,-0.0318374308466215,
-0.0128180447586783));
#22053=CARTESIAN_POINT('Ctrl Pts',(-0.0139424311107755,-0.0318321979428736,
-0.0127317091060275));
#22054=CARTESIAN_POINT('Ctrl Pts',(-0.0139910963525862,-0.0318229885074964,
-0.0125783767836752));
#22055=CARTESIAN_POINT('Ctrl Pts',(-0.0140072568250182,-0.0318190829830428,
-0.0125128553779215));
#22056=CARTESIAN_POINT('Ctrl Pts',(-0.0140278290876955,-0.031812422048736,
-0.0123973822912105));
#22057=CARTESIAN_POINT('Ctrl Pts',(-0.0140341920576218,-0.0318096367507819,
-0.0123478776869965));
#22058=CARTESIAN_POINT('Ctrl Pts',(-0.0140389177835271,-0.0318064415575806,
-0.0122884405341281));
#22059=CARTESIAN_POINT('Ctrl Pts',(-0.0140395977153843,-0.0318059240643805,
-0.0122787256205836));
#22060=CARTESIAN_POINT('Ctrl Pts',(-0.0140405172755869,-0.031805122299086,
-0.0122635214099575));
#22061=CARTESIAN_POINT('Ctrl Pts',(-0.0140408196282058,-0.0318048347066493,
-0.0122580363226576));
#22062=CARTESIAN_POINT('Ctrl Pts',(-0.0140413330832879,-0.031804297025581,
-0.0122477192516973));
#22063=CARTESIAN_POINT('Ctrl Pts',(-0.0140415507622473,-0.0318040465978552,
-0.0122428878919822));
#22064=CARTESIAN_POINT('Ctrl Pts',(-0.0140420046998314,-0.0318034664649263,
-0.0122316365662889));
#22065=CARTESIAN_POINT('Ctrl Pts',(-0.0140422235856369,-0.0318031377252097,
-0.0122252160593249));
#22066=CARTESIAN_POINT('Ctrl Pts',(-0.0140428007586163,-0.0318020831670447,
-0.012204484510068));
#22067=CARTESIAN_POINT('Ctrl Pts',(-0.0140430000000001,-0.0318013656520773,
-0.0121901694497616));
#22068=CARTESIAN_POINT('Ctrl Pts',(-0.014043,-0.0318006569328344,-0.0121758532865438));
#22069=CARTESIAN_POINT('Ctrl Pts',(-0.014043,-0.0319166517728185,-0.012175853294288));
#22070=CARTESIAN_POINT('Ctrl Pts',(-0.0140429999999704,-0.0319169422534939,
-0.0121817624597713));
#22071=CARTESIAN_POINT('Ctrl Pts',(-0.0140429660548091,-0.0319172337445512,
-0.0121876722341942));
#22072=CARTESIAN_POINT('Ctrl Pts',(-0.0140427051512635,-0.0319183575977179,
-0.0122103777823771));
#22073=CARTESIAN_POINT('Ctrl Pts',(-0.0140422379333357,-0.0319191969743863,
-0.0122271685248212));
#22074=CARTESIAN_POINT('Ctrl Pts',(-0.0140410627718577,-0.0319205413333712,
-0.0122537713290109));
#22075=CARTESIAN_POINT('Ctrl Pts',(-0.01404053494283,-0.0319210406534681,
-0.012263590235529));
#22076=CARTESIAN_POINT('Ctrl Pts',(-0.0140393719069067,-0.0319219803902146,
-0.012281949790573));
#22077=CARTESIAN_POINT('Ctrl Pts',(-0.0140387593723613,-0.0319224200743601,
-0.012290491526098));
#22078=CARTESIAN_POINT('Ctrl Pts',(-0.0140372278659085,-0.0319234101772051,
-0.0123096154226401));
#22079=CARTESIAN_POINT('Ctrl Pts',(-0.0140362706686662,-0.03192396178414,
-0.0123201940145537));
#22080=CARTESIAN_POINT('Ctrl Pts',(-0.0140330862384887,-0.0319256194078617,
-0.012351752990122));
#22081=CARTESIAN_POINT('Ctrl Pts',(-0.0140305379026275,-0.0319267354658688,
-0.0123726978684155));
#22082=CARTESIAN_POINT('Ctrl Pts',(-0.0140163573164733,-0.0319321145826708,
-0.0124721867527332));
#22083=CARTESIAN_POINT('Ctrl Pts',(-0.0139991047897372,-0.0319365516829508,
-0.0125497986723084));
#22084=CARTESIAN_POINT('Ctrl Pts',(-0.0139514649066583,-0.031945879745736,
-0.0127060959049457));
#22085=CARTESIAN_POINT('Ctrl Pts',(-0.0139204468957665,-0.0319507665606939,
-0.0127843253274699));
#22086=CARTESIAN_POINT('Ctrl Pts',(-0.0138652568777996,-0.0319577884795798,
-0.0128959677289772));
#22087=CARTESIAN_POINT('Ctrl Pts',(-0.0138458731720214,-0.0319600340530743,
-0.0129315761544118));
#22088=CARTESIAN_POINT('Ctrl Pts',(-0.0138201805120936,-0.0319627204035708,
-0.0129746429565677));
#22089=CARTESIAN_POINT('Ctrl Pts',(-0.0138151752260996,-0.031963231396606,
-0.0129828574100301));
#22090=CARTESIAN_POINT('Ctrl Pts',(-0.0138071972516023,-0.0319640261151596,
-0.0129956791193369));
#22091=CARTESIAN_POINT('Ctrl Pts',(-0.0138042763461494,-0.031964313052479,
-0.0130003181223142));
#22092=CARTESIAN_POINT('Ctrl Pts',(-0.0137987156101211,-0.0319648516270746,
-0.0130090462121896));
#22093=CARTESIAN_POINT('Ctrl Pts',(-0.0137960811021365,-0.0319651035859133,
-0.0130131384615522));
#22094=CARTESIAN_POINT('Ctrl Pts',(-0.0137898083069323,-0.0319656961064391,
-0.0130227816064802));
#22095=CARTESIAN_POINT('Ctrl Pts',(-0.0137861534562582,-0.0319660355748878,
-0.0130283216659042));
#22096=CARTESIAN_POINT('Ctrl Pts',(-0.0137737921095495,-0.0319671652006882,
-0.0130467986470862));
#22097=CARTESIAN_POINT('Ctrl Pts',(-0.013764925022248,-0.0319679452898744,
-0.0130596275126013));
#22098=CARTESIAN_POINT('Ctrl Pts',(-0.0137427744656077,-0.0319698274324029,
-0.0130906583301425));
#22099=CARTESIAN_POINT('Ctrl Pts',(-0.0137292836388706,-0.031970918139689,
-0.0131087082895254));
#22100=CARTESIAN_POINT('Ctrl Pts',(-0.0136708955153006,-0.031975440632618,
-0.0131833608826115));
#22101=CARTESIAN_POINT('Ctrl Pts',(-0.0136224453854206,-0.0319787263198167,
-0.0132370721023809));
#22102=CARTESIAN_POINT('Ctrl Pts',(-0.0134992967630453,-0.0319865425461815,
-0.0133556850161962));
#22103=CARTESIAN_POINT('Ctrl Pts',(-0.0134217799183298,-0.0319910816732149,
-0.0134171898733728));
#22104=CARTESIAN_POINT('Ctrl Pts',(-0.0133206694192779,-0.0319969898729515,
-0.0134826906383517));
#22105=CARTESIAN_POINT('Ctrl Pts',(-0.0133021657511994,-0.0319980696954103,
-0.0134941295127196));
#22106=CARTESIAN_POINT('Ctrl Pts',(-0.0132741667858537,-0.0319997045317629,
-0.0135106305426203));
#22107=CARTESIAN_POINT('Ctrl Pts',(-0.0132648499467091,-0.0320002486689731,
-0.0135159909985312));
#22108=CARTESIAN_POINT('Ctrl Pts',(-0.0132480023222733,-0.0320012331992971,
-0.0135254513872195));
#22109=CARTESIAN_POINT('Ctrl Pts',(-0.0132404918790416,-0.0320016722887083,
-0.0135295867465001));
#22110=CARTESIAN_POINT('Ctrl Pts',(-0.0132243723881314,-0.0320026152795823,
-0.0135382880928566));
#22111=CARTESIAN_POINT('Ctrl Pts',(-0.013215753795921,-0.0320031198192404,
-0.0135428355307223));
#22112=CARTESIAN_POINT('Ctrl Pts',(-0.0131921329600889,-0.0320045037901023,
-0.013555013993079));
#22113=CARTESIAN_POINT('Ctrl Pts',(-0.0131770483068297,-0.0320053889219412,
-0.0135624815167361));
#22114=CARTESIAN_POINT('Ctrl Pts',(-0.013078484710178,-0.032011182453819,
-0.0136092827796161));
#22115=CARTESIAN_POINT('Ctrl Pts',(-0.0129917537958947,-0.032016343456613,
-0.0136413015193974));
#22116=CARTESIAN_POINT('Ctrl Pts',(-0.0128127401473149,-0.0320269541029228,
-0.0136896979822628));
#22117=CARTESIAN_POINT('Ctrl Pts',(-0.0127207672858566,-0.0320323822922919,
-0.0137058188526549));
#22118=CARTESIAN_POINT('Ctrl Pts',(-0.0126001934017919,-0.0320391054182371,
-0.0137158478645137));
#22119=CARTESIAN_POINT('Ctrl Pts',(-0.0125724269560706,-0.0320406258176822,
-0.0137174033299859));
#22120=CARTESIAN_POINT('Ctrl Pts',(-0.0125361078259006,-0.0320425652275291,
-0.0137184543202629));
#22121=CARTESIAN_POINT('Ctrl Pts',(-0.0125275814496023,-0.0320430169774265,
-0.0137186303263275));
#22122=CARTESIAN_POINT('Ctrl Pts',(-0.0125138114984911,-0.0320437403275864,
-0.013718800378684));
#22123=CARTESIAN_POINT('Ctrl Pts',(-0.0125085687592662,-0.0320440142790308,
-0.0137188384013834));
#22124=CARTESIAN_POINT('Ctrl Pts',(-0.0124983601186337,-0.0320445447452104,
-0.0137188604055981));
#22125=CARTESIAN_POINT('Ctrl Pts',(-0.0124933943547235,-0.0320448013974494,
-0.0137188471376502));
#22126=CARTESIAN_POINT('Ctrl Pts',(-0.0124812066377706,-0.0320454280943007,
-0.013718755736726));
#22127=CARTESIAN_POINT('Ctrl Pts',(-0.0124739849020089,-0.0320457966692349,
-0.0137186508688197));
#22128=CARTESIAN_POINT('Ctrl Pts',(-0.0124473971903043,-0.032047144279301,
-0.0137180780409634));
#22129=CARTESIAN_POINT('Ctrl Pts',(-0.0124280390797191,-0.032048107201025,
-0.0137172960974338));
#22130=CARTESIAN_POINT('Ctrl Pts',(-0.0123783766262372,-0.0320505420554229,
-0.0137143523908195));
#22131=CARTESIAN_POINT('Ctrl Pts',(-0.0123481114512134,-0.0320519919471633,
-0.0137116598435217));
#22132=CARTESIAN_POINT('Ctrl Pts',(-0.0122505129668877,-0.0320566112387483,
-0.0137000633715691));
#22133=CARTESIAN_POINT('Ctrl Pts',(-0.0121836818544641,-0.0320596898314799,
-0.0136876084454355));
#22134=CARTESIAN_POINT('Ctrl Pts',(-0.0120229158364813,-0.0320672850412203,
-0.0136465158741246));
#22135=CARTESIAN_POINT('Ctrl Pts',(-0.011930484834166,-0.0320718285865343,
-0.0136132494119354));
#22136=CARTESIAN_POINT('Ctrl Pts',(-0.0118266446090333,-0.0320775108559329,
-0.013564278175693));
#22137=CARTESIAN_POINT('Ctrl Pts',(-0.0118115702840447,-0.0320783502771295,
-0.0135568658330794));
#22138=CARTESIAN_POINT('Ctrl Pts',(-0.0117878682210418,-0.032079694691472,
-0.01354472655373));
#22139=CARTESIAN_POINT('Ctrl Pts',(-0.011779159296538,-0.0320801940215883,
-0.0135401605710662));
#22140=CARTESIAN_POINT('Ctrl Pts',(-0.0117629486601084,-0.0320811337671448,
-0.0135314629862703));
#22141=CARTESIAN_POINT('Ctrl Pts',(-0.0117554365231385,-0.0320815734499467,
-0.013527351551659));
#22142=CARTESIAN_POINT('Ctrl Pts',(-0.0117386846254669,-0.0320825635364429,
-0.0135180010858926));
#22143=CARTESIAN_POINT('Ctrl Pts',(-0.0117294640141239,-0.0320831151282,
-0.0135127287862278));
#22144=CARTESIAN_POINT('Ctrl Pts',(-0.0117020938763298,-0.0320847726599055,
-0.0134967014523874));
#22145=CARTESIAN_POINT('Ctrl Pts',(-0.0116841102276577,-0.0320858886394198,
-0.0134856692580569));
#22146=CARTESIAN_POINT('Ctrl Pts',(-0.0115995562540498,-0.03209126703914,
-0.0134313819550415));
#22147=CARTESIAN_POINT('Ctrl Pts',(-0.0115361712344603,-0.0320957034469407,
-0.0133834055945569));
#22148=CARTESIAN_POINT('Ctrl Pts',(-0.0114138978568064,-0.032105029388017,
-0.0132750737526457));
#22149=CARTESIAN_POINT('Ctrl Pts',(-0.0113556848857642,-0.0321099147532679,
-0.0132143360332975));
#22150=CARTESIAN_POINT('Ctrl Pts',(-0.0112771204596531,-0.0321169374722964,
-0.0131176916970582));
#22151=CARTESIAN_POINT('Ctrl Pts',(-0.0112527855390189,-0.0321191850388395,
-0.0130852214994991));
#22152=CARTESIAN_POINT('Ctrl Pts',(-0.0112242949873362,-0.0321218733759114,
-0.0130439075950904));
#22153=CARTESIAN_POINT('Ctrl Pts',(-0.0112189071713629,-0.0321223844833262,
-0.0130359362683328));
#22154=CARTESIAN_POINT('Ctrl Pts',(-0.0112105667440473,-0.03212317933925,
-0.0130233442506023));
#22155=CARTESIAN_POINT('Ctrl Pts',(-0.011207563687886,-0.0321234663013213,
-0.0130187574546923));
#22156=CARTESIAN_POINT('Ctrl Pts',(-0.011201940978569,-0.0321240048945783,
-0.0130100687640944));
#22157=CARTESIAN_POINT('Ctrl Pts',(-0.0111993162298553,-0.0321242568476558,
-0.0130059703966385));
#22158=CARTESIAN_POINT('Ctrl Pts',(-0.0111931584837095,-0.0321248493176249,
-0.0129962545830056));
#22159=CARTESIAN_POINT('Ctrl Pts',(-0.0111896422235246,-0.0321251887418385,
-0.0129906265904009));
#22160=CARTESIAN_POINT('Ctrl Pts',(-0.0111779880860844,-0.0321263180594005,
-0.0129717028290849));
#22161=CARTESIAN_POINT('Ctrl Pts',(-0.0111700151646058,-0.0321270978920825,
-0.0129583060759418));
#22162=CARTESIAN_POINT('Ctrl Pts',(-0.0111510234573555,-0.0321289792913082,
-0.0129252653659614));
#22163=CARTESIAN_POINT('Ctrl Pts',(-0.0111402289115818,-0.0321300695235784,
-0.0129054962441676));
#22164=CARTESIAN_POINT('Ctrl Pts',(-0.011096674195217,-0.0321345886825178,
-0.0128214039259133));
#22165=CARTESIAN_POINT('Ctrl Pts',(-0.0110680141644286,-0.0321378717271535,
-0.0127550567583075));
#22166=CARTESIAN_POINT('Ctrl Pts',(-0.0110113731883091,-0.032145688809762,
-0.0125937088234088));
#22167=CARTESIAN_POINT('Ctrl Pts',(-0.0109876766916429,-0.0321502314013961,
-0.0124975504302443));
#22168=CARTESIAN_POINT('Ctrl Pts',(-0.0109701803805182,-0.0321561435539088,
-0.0123782737419149));
#22169=CARTESIAN_POINT('Ctrl Pts',(-0.0109674790815342,-0.0321572233199449,
-0.012356689357217));
#22170=CARTESIAN_POINT('Ctrl Pts',(-0.0109641260040787,-0.0321588580874549,
-0.0123243645636871));
#22171=CARTESIAN_POINT('Ctrl Pts',(-0.0109631287621924,-0.0321594022136373,
-0.0123136622906007));
#22172=CARTESIAN_POINT('Ctrl Pts',(-0.0109615372199236,-0.0321603867320347,
-0.0122944061499693));
#22173=CARTESIAN_POINT('Ctrl Pts',(-0.0109609022454603,-0.0321608258206849,
-0.0122858560371255));
#22174=CARTESIAN_POINT('Ctrl Pts',(-0.0109596978758653,-0.0321617688187711,
-0.0122675774786374));
#22175=CARTESIAN_POINT('Ctrl Pts',(-0.010959149322553,-0.0321622733665018,
-0.0122578480728074));
#22176=CARTESIAN_POINT('Ctrl Pts',(-0.0109579047110446,-0.0321636573826688,
-0.0122313008497113));
#22177=CARTESIAN_POINT('Ctrl Pts',(-0.0109573916382353,-0.0321645425523657,
-0.0122144761339798));
#22178=CARTESIAN_POINT('Ctrl Pts',(-0.0109558501300154,-0.0321703376501135,
-0.0121053470060591));
#22179=CARTESIAN_POINT('Ctrl Pts',(-0.0109628316203562,-0.0321755003490587,
-0.0120131296779549));
#22180=CARTESIAN_POINT('Ctrl Pts',(-0.0109933409255827,-0.0321861156027621,
-0.0118301368019082));
#22181=CARTESIAN_POINT('Ctrl Pts',(-0.0110169770976427,-0.0321915467249982,
-0.0117397510100458));
#22182=CARTESIAN_POINT('Ctrl Pts',(-0.0110580443883101,-0.0321982683749375,
-0.0116259602098475));
#22183=CARTESIAN_POINT('Ctrl Pts',(-0.0110681629142342,-0.0321997850792603,
-0.0116001266821526));
#22184=CARTESIAN_POINT('Ctrl Pts',(-0.0110822933137908,-0.0322017205603752,
-0.0115667314981259));
#22185=CARTESIAN_POINT('Ctrl Pts',(-0.0110856786444253,-0.0322021719189494,
-0.0115589118704271));
#22186=CARTESIAN_POINT('Ctrl Pts',(-0.0110912507092514,-0.0322028947967239,
-0.0115463281434806));
#22187=CARTESIAN_POINT('Ctrl Pts',(-0.0110933972028274,-0.0322031686617601,
-0.0115415465448679));
#22188=CARTESIAN_POINT('Ctrl Pts',(-0.0110976251436653,-0.0322036990882563,
-0.0115322552518551));
#22189=CARTESIAN_POINT('Ctrl Pts',(-0.0110997040558569,-0.0322039557858975,
-0.0115277445478319));
#22190=CARTESIAN_POINT('Ctrl Pts',(-0.0111048614540886,-0.0322045827758229,
-0.0115166949823676));
#22191=CARTESIAN_POINT('Ctrl Pts',(-0.0111079642141444,-0.0322049515951886,
-0.0115101674694237));
#22192=CARTESIAN_POINT('Ctrl Pts',(-0.0111195667612765,-0.0322063011771879,
-0.0114861941946474));
#22193=CARTESIAN_POINT('Ctrl Pts',(-0.0111283498874238,-0.0322072657648647,
-0.0114688867928833));
#22194=CARTESIAN_POINT('Ctrl Pts',(-0.0111517487311405,-0.0322097058792018,
-0.0114248573387118));
#22195=CARTESIAN_POINT('Ctrl Pts',(-0.0111668335932105,-0.0322111592442367,
-0.0113983933818991));
#22196=CARTESIAN_POINT('Ctrl Pts',(-0.011218245431407,-0.032215799021166,
-0.0113141015688734));
#22197=CARTESIAN_POINT('Ctrl Pts',(-0.0112576293993007,-0.0322188937404567,
-0.0112582331258105));
#22198=CARTESIAN_POINT('Ctrl Pts',(-0.0113569037998826,-0.0322261176008592,
-0.0111355676082758));
#22199=CARTESIAN_POINT('Ctrl Pts',(-0.0114191674707024,-0.0322302625613331,
-0.0110710174130741));
#22200=CARTESIAN_POINT('Ctrl Pts',(-0.0115030776349032,-0.0322357192888351,
-0.010997944910605));
#22201=CARTESIAN_POINT('Ctrl Pts',(-0.0115197846167669,-0.0322367993157329,
-0.0109840059441173));
#22202=CARTESIAN_POINT('Ctrl Pts',(-0.0115451780432855,-0.0322384344015361,
-0.0109637148521648));
#22203=CARTESIAN_POINT('Ctrl Pts',(-0.0115536456085968,-0.0322389785787183,
-0.0109570924767839));
#22204=CARTESIAN_POINT('Ctrl Pts',(-0.0115689899199205,-0.032239963152296,
-0.0109453482116252));
#22205=CARTESIAN_POINT('Ctrl Pts',(-0.0115758415173753,-0.0322404022444899,
-0.0109401941087521));
#22206=CARTESIAN_POINT('Ctrl Pts',(-0.0115905710423415,-0.0322413452093064,
-0.0109293048845732));
#22207=CARTESIAN_POINT('Ctrl Pts',(-0.0115984610302843,-0.0322418497197641,
-0.010923586770301));
#22208=CARTESIAN_POINT('Ctrl Pts',(-0.0116201238511323,-0.0322432335266724,
-0.0109081979051512));
#22209=CARTESIAN_POINT('Ctrl Pts',(-0.0116340013053723,-0.032244118521495,
-0.0108986773261174));
#22210=CARTESIAN_POINT('Ctrl Pts',(-0.0117248834550524,-0.0322499064025573,
-0.0108384902259258));
#22211=CARTESIAN_POINT('Ctrl Pts',(-0.0118061304776674,-0.0322550612853422,
-0.0107945906897392));
#22212=CARTESIAN_POINT('Ctrl Pts',(-0.0119762458062526,-0.0322656553284739,
-0.0107214873447004));
#22213=CARTESIAN_POINT('Ctrl Pts',(-0.01206483966933,-0.0322710729570748,
-0.0106925681206186));
#22214=CARTESIAN_POINT('Ctrl Pts',(-0.0121828310401409,-0.0322778014209382,
-0.0106655423719038));
#22215=CARTESIAN_POINT('Ctrl Pts',(-0.0122103299047898,-0.0322793351559365,
-0.0106600278907194));
#22216=CARTESIAN_POINT('Ctrl Pts',(-0.0122463948042114,-0.0322812887332433,
-0.0106538130206249));
#22217=CARTESIAN_POINT('Ctrl Pts',(-0.0122548364234306,-0.0322817418870856,
-0.0106524304976524));
#22218=CARTESIAN_POINT('Ctrl Pts',(-0.0122684756223713,-0.0322824669319866,
-0.0106503130514614));
#22219=CARTESIAN_POINT('Ctrl Pts',(-0.0122736661062311,-0.0322827411934426,
-0.0106495343433195));
#22220=CARTESIAN_POINT('Ctrl Pts',(-0.0122837717217313,-0.0322832718039773,
-0.0106480709207708));
#22221=CARTESIAN_POINT('Ctrl Pts',(-0.0122886863140448,-0.0322835282952914,
-0.01064738341375));
#22222=CARTESIAN_POINT('Ctrl Pts',(-0.0123007441942925,-0.0322841539498816,
-0.0106457558933926));
#22223=CARTESIAN_POINT('Ctrl Pts',(-0.0123078910134248,-0.0322845216549992,
-0.0106448421664524));
#22224=CARTESIAN_POINT('Ctrl Pts',(-0.0123341540218158,-0.0322858622687672,
-0.0106416712165045));
#22225=CARTESIAN_POINT('Ctrl Pts',(-0.0123533062680993,-0.0322868192813766,
-0.0106397216108868));
#22226=CARTESIAN_POINT('Ctrl Pts',(-0.0124024935538336,-0.0322892355134744,
-0.010635642960321));
#22227=CARTESIAN_POINT('Ctrl Pts',(-0.0124325641655228,-0.0322906731164171,
-0.0106340336040558));
#22228=CARTESIAN_POINT('Ctrl Pts',(-0.0125292533641203,-0.0322952207938548,
-0.0106316933225697));
#22229=CARTESIAN_POINT('Ctrl Pts',(-0.0125958796663092,-0.0322982431290773,
-0.0106343950511176));
#22230=CARTESIAN_POINT('Ctrl Pts',(-0.0127612711648686,-0.0323058529334065,
-0.0106518696511979));
#22231=CARTESIAN_POINT('Ctrl Pts',(-0.0128591577506311,-0.0323104675815919,
-0.0106719278231339));
#22232=CARTESIAN_POINT('Ctrl Pts',(-0.0129705046211916,-0.0323162338886589,
-0.0107062418997138));
#22233=CARTESIAN_POINT('Ctrl Pts',(-0.0129865049967269,-0.0323170748592469,
-0.0107114608913793));
#22234=CARTESIAN_POINT('Ctrl Pts',(-0.0130117205299129,-0.0323184212001292,
-0.0107201445478324));
#22235=CARTESIAN_POINT('Ctrl Pts',(-0.0130209936233605,-0.0323189208791938,
-0.0107234375501757));
#22236=CARTESIAN_POINT('Ctrl Pts',(-0.013038275914345,-0.0323198609326567,
-0.0107297615315659));
#22237=CARTESIAN_POINT('Ctrl Pts',(-0.013046292635808,-0.0323203005697546,
-0.0107327709341124));
#22238=CARTESIAN_POINT('Ctrl Pts',(-0.0130641871037121,-0.0323212900913802,
-0.0107396588294172));
#22239=CARTESIAN_POINT('Ctrl Pts',(-0.0130740506592899,-0.0323218411579902,
-0.010743572783411));
#22240=CARTESIAN_POINT('Ctrl Pts',(-0.0131033543346783,-0.0323234955058182,
-0.0107555520867022));
#22241=CARTESIAN_POINT('Ctrl Pts',(-0.0131226700925024,-0.0323246087694194,
-0.0107639135398794));
#22242=CARTESIAN_POINT('Ctrl Pts',(-0.0132136337266458,-0.0323299624000507,
-0.0108055197128482));
#22243=CARTESIAN_POINT('Ctrl Pts',(-0.0132828221127666,-0.0323343748988194,
-0.0108438344934591));
#22244=CARTESIAN_POINT('Ctrl Pts',(-0.0134181972058184,-0.0323436271259771,
-0.0109330037934953));
#22245=CARTESIAN_POINT('Ctrl Pts',(-0.0134838165852728,-0.0323484619563676,
-0.0109842720454189));
#22246=CARTESIAN_POINT('Ctrl Pts',(-0.0135757289940174,-0.0323555134702802,
-0.0110688745059318));
#22247=CARTESIAN_POINT('Ctrl Pts',(-0.0136053122046139,-0.0323578315518118,
-0.011098411707659));
#22248=CARTESIAN_POINT('Ctrl Pts',(-0.013640153666218,-0.0323605833376665,
-0.0111361465028885));
#22249=CARTESIAN_POINT('Ctrl Pts',(-0.0136465801365082,-0.0323610918480808,
-0.0111432378798205));
#22250=CARTESIAN_POINT('Ctrl Pts',(-0.01365661317641,-0.0323618865789594,
-0.011154518130326));
#22251=CARTESIAN_POINT('Ctrl Pts',(-0.0136602638261778,-0.0323621759315623,
-0.0111586672678074));
#22252=CARTESIAN_POINT('Ctrl Pts',(-0.0136670800446404,-0.0323627163734295,
-0.0111664986674117));
#22253=CARTESIAN_POINT('Ctrl Pts',(-0.0136702505251697,-0.032362967811008,
-0.0111701762576503));
#22254=CARTESIAN_POINT('Ctrl Pts',(-0.0136776591715056,-0.0323635556007237,
-0.0111788523739204));
#22255=CARTESIAN_POINT('Ctrl Pts',(-0.0136818829145273,-0.0323638909071585,
-0.0111838630026428));
#22256=CARTESIAN_POINT('Ctrl Pts',(-0.0136957348818779,-0.0323649918051742,
-0.0112005096625076));
#22257=CARTESIAN_POINT('Ctrl Pts',(-0.0137052244605922,-0.0323657480149955,
-0.011212260465689));
#22258=CARTESIAN_POINT('Ctrl Pts',(-0.0137278523818071,-0.0323675613209275,
-0.0112411376347031));
#22259=CARTESIAN_POINT('Ctrl Pts',(-0.0137408070774015,-0.0323686081332972,
-0.0112584042739884));
#22260=CARTESIAN_POINT('Ctrl Pts',(-0.0137923220884857,-0.0323728321358293,
-0.0113301539952048));
#22261=CARTESIAN_POINT('Ctrl Pts',(-0.0138276919353843,-0.0323758820507518,
-0.0113868420124714));
#22262=CARTESIAN_POINT('Ctrl Pts',(-0.0139095396231259,-0.032383787597368,
-0.0115392012996929));
#22263=CARTESIAN_POINT('Ctrl Pts',(-0.0139500007379712,-0.032388642164868,
-0.0116376867040619));
#22264=CARTESIAN_POINT('Ctrl Pts',(-0.0139860484821259,-0.0323948962800243,
-0.0117599659943611));
#22265=CARTESIAN_POINT('Ctrl Pts',(-0.0139916454875632,-0.0323959533441385,
-0.0117805103782178));
#22266=CARTESIAN_POINT('Ctrl Pts',(-0.0139994382659481,-0.0323975673383834,
-0.011811641058401));
#22267=CARTESIAN_POINT('Ctrl Pts',(-0.0140019509509674,-0.0323981140334458,
-0.0118221457891512));
#22268=CARTESIAN_POINT('Ctrl Pts',(-0.0140062609982421,-0.0323991013395911,
-0.0118410393193961));
#22269=CARTESIAN_POINT('Ctrl Pts',(-0.0140080990893304,-0.0323995406150394,
-0.0118494184228482));
#22270=CARTESIAN_POINT('Ctrl Pts',(-0.0140118687026241,-0.0324004819773254,
-0.0118673142784492));
#22271=CARTESIAN_POINT('Ctrl Pts',(-0.0140137804400154,-0.0324009846796224,
-0.011876834780237));
#22272=CARTESIAN_POINT('Ctrl Pts',(-0.0140187298901506,-0.0324023583439381,
-0.0119027480668268));
#22273=CARTESIAN_POINT('Ctrl Pts',(-0.0140215919319507,-0.0324032348650724,
-0.0119191727391614));
#22274=CARTESIAN_POINT('Ctrl Pts',(-0.014036712830561,-0.0324083904766337,
-0.0120151170314925));
#22275=CARTESIAN_POINT('Ctrl Pts',(-0.0140430000005061,-0.0324128571794188,
-0.0120954324537772));
#22276=CARTESIAN_POINT('Ctrl Pts',(-0.014043,-0.0324174341340783,-0.0121758532962676));
#22277=CARTESIAN_POINT('Origin',(-0.0125,-0.0375520664398416,-0.0121758532865581));
#22278=CARTESIAN_POINT('',(-0.014043,-0.0329194567307744,-0.012175853286558));
#22279=CARTESIAN_POINT('',(-0.014043,-0.0328035263970765,-0.012175853286558));
#22280=CARTESIAN_POINT('',(-0.014043,-0.0375520664398416,-0.012175853286558));
#22281=CARTESIAN_POINT('',(-0.0140429999983096,-0.0328035227368026,-0.0121757810608236));
#22282=CARTESIAN_POINT('Ctrl Pts',(-0.014043,-0.0328035263970765,-0.012175853286558));
#22283=CARTESIAN_POINT('Ctrl Pts',(-0.014043,-0.0328035250082943,-0.0121758258822526));
#22284=CARTESIAN_POINT('Ctrl Pts',(-0.0140429999992699,-0.0328035236194892,
-0.0121757984779469));
#22285=CARTESIAN_POINT('Ctrl Pts',(-0.0140429999978098,-0.0328035222306614,
-0.0121757710736408));
#22286=CARTESIAN_POINT('Ctrl Pts',(-0.0140429999983096,-0.0328035227368026,
-0.0121757810608236));
#22287=CARTESIAN_POINT('Ctrl Pts',(-0.0140429997244644,-0.032803226248909,
-0.0121699307479627));
#22288=CARTESIAN_POINT('Ctrl Pts',(-0.0140429662544466,-0.0328029292367222,
-0.0121640905248185));
#22289=CARTESIAN_POINT('Ctrl Pts',(-0.0140428326113774,-0.0328023317104684,
-0.0121523831128644));
#22290=CARTESIAN_POINT('Ctrl Pts',(-0.0140427323894257,-0.0328020317059399,
-0.0121465260101399));
#22291=CARTESIAN_POINT('Ctrl Pts',(-0.0140423926184721,-0.0328012658944575,
-0.0121316290106755));
#22292=CARTESIAN_POINT('Ctrl Pts',(-0.0140421069495067,-0.0328007986457035,
-0.0121225904693319));
#22293=CARTESIAN_POINT('Ctrl Pts',(-0.0140411769421325,-0.0327996020335943,
-0.0120995748553997));
#22294=CARTESIAN_POINT('Ctrl Pts',(-0.0140404219178594,-0.0327988692188615,
-0.0120856032807187));
#22295=CARTESIAN_POINT('Ctrl Pts',(-0.014036550875133,-0.0327958427418227,
-0.0120284165045126));
#22296=CARTESIAN_POINT('Ctrl Pts',(-0.0140318055634194,-0.0327934986844895,
-0.0119853344806585));
#22297=CARTESIAN_POINT('Ctrl Pts',(-0.0140199972636875,-0.0327891861370116,
-0.0119081486292883));
#22298=CARTESIAN_POINT('Ctrl Pts',(-0.0140135806720148,-0.0327872363642042,
-0.011873974482153));
#22299=CARTESIAN_POINT('Ctrl Pts',(-0.0139837811262394,-0.0327794733027683,
-0.0117403299865484));
#22300=CARTESIAN_POINT('Ctrl Pts',(-0.0139516989191298,-0.0327734991223908,
-0.0116430715414537));
#22301=CARTESIAN_POINT('Ctrl Pts',(-0.0139001588968634,-0.0327663675661505,
-0.0115269917098509));
#22302=CARTESIAN_POINT('Ctrl Pts',(-0.013889529205442,-0.0327649887308705,
-0.0115045299815642));
#22303=CARTESIAN_POINT('Ctrl Pts',(-0.0138708348424866,-0.0327627213181017,
-0.0114673751691735));
#22304=CARTESIAN_POINT('Ctrl Pts',(-0.013863065111816,-0.0327618196361788,
-0.0114525394169333));
#22305=CARTESIAN_POINT('Ctrl Pts',(-0.0138517984869085,-0.0327605707356656,
-0.0114318531459254));
#22306=CARTESIAN_POINT('Ctrl Pts',(-0.0138485022640765,-0.0327602120316526,
-0.0114258952839585));
#22307=CARTESIAN_POINT('Ctrl Pts',(-0.0138427778257623,-0.0327596006749833,
-0.011415708241936));
#22308=CARTESIAN_POINT('Ctrl Pts',(-0.0138403688191471,-0.0327593468267121,
-0.0114114684297682));
#22309=CARTESIAN_POINT('Ctrl Pts',(-0.0138352689187748,-0.0327588166531116,
-0.0114025909371715));
#22310=CARTESIAN_POINT('Ctrl Pts',(-0.0138325739117848,-0.0327585405927337,
-0.0113979557883235));
#22311=CARTESIAN_POINT('Ctrl Pts',(-0.0138252227961144,-0.0327577983336406,
-0.0113854629012682));
#22312=CARTESIAN_POINT('Ctrl Pts',(-0.0138205209230791,-0.0327573350055703,
-0.0113776321894092));
#22313=CARTESIAN_POINT('Ctrl Pts',(-0.013797749268969,-0.0327551425741716,
-0.0113404591951907));
#22314=CARTESIAN_POINT('Ctrl Pts',(-0.0137787683345102,-0.0327534664295224,
-0.0113116841417433));
#22315=CARTESIAN_POINT('Ctrl Pts',(-0.013707724800304,-0.0327476163614296,
-0.0112114558279984));
#22316=CARTESIAN_POINT('Ctrl Pts',(-0.0136505067409734,-0.0327436410706501,
-0.0111438660428199));
#22317=CARTESIAN_POINT('Ctrl Pts',(-0.0135243824325406,-0.0327354796503313,
-0.0110184903610312));
#22318=CARTESIAN_POINT('Ctrl Pts',(-0.0134555945387388,-0.0327313036492548,
-0.0109610754836151));
#22319=CARTESIAN_POINT('Ctrl Pts',(-0.0133685166019989,-0.0327260473694893,
-0.0109003897604941));
#22320=CARTESIAN_POINT('Ctrl Pts',(-0.0133546516847554,-0.0327252117478388,
-0.0108910580637586));
#22321=CARTESIAN_POINT('Ctrl Pts',(-0.0133325099890432,-0.0327238780371024,
-0.0108766727468868));
#22322=CARTESIAN_POINT('Ctrl Pts',(-0.0133243322634616,-0.0327233856101872,
-0.010871468653743));
#22323=CARTESIAN_POINT('Ctrl Pts',(-0.0133088603065355,-0.0327224540197819,
-0.0108618263086129));
#22324=CARTESIAN_POINT('Ctrl Pts',(-0.0133015771911879,-0.032722015518471,
-0.0108573708646372));
#22325=CARTESIAN_POINT('Ctrl Pts',(-0.0132850706713883,-0.0327210215969352,
-0.0108474603234615));
#22326=CARTESIAN_POINT('Ctrl Pts',(-0.0132758267262926,-0.0327204649138006,
-0.0108420404412043));
#22327=CARTESIAN_POINT('Ctrl Pts',(-0.0132476748534127,-0.0327187690472513,
-0.0108259261865134));
#22328=CARTESIAN_POINT('Ctrl Pts',(-0.0132285973984482,-0.0327176190776858,
-0.010815534710689));
#22329=CARTESIAN_POINT('Ctrl Pts',(-0.0131303402214902,-0.0327116905567254,
-0.0107646740380959));
#22330=CARTESIAN_POINT('Ctrl Pts',(-0.0130479976322164,-0.0327066898361415,
-0.0107307060445875));
#22331=CARTESIAN_POINT('Ctrl Pts',(-0.0128868339071897,-0.032697006236147,
-0.0106799863916181));
#22332=CARTESIAN_POINT('Ctrl Pts',(-0.0128087131819163,-0.0326923591923312,
-0.0106619329192578));
#22333=CARTESIAN_POINT('Ctrl Pts',(-0.0127060641022901,-0.0326865408525819,
-0.0106464905632975));
#22334=CARTESIAN_POINT('Ctrl Pts',(-0.0126825053440603,-0.0326852253882661,
-0.0106435006341352));
#22335=CARTESIAN_POINT('Ctrl Pts',(-0.0126427753067765,-0.032683050396092,
-0.010639387683986));
#22336=CARTESIAN_POINT('Ctrl Pts',(-0.0126266387098334,-0.0326821790053556,
-0.0106379735727623));
#22337=CARTESIAN_POINT('Ctrl Pts',(-0.0126037793719043,-0.0326809643850252,
-0.0106363325813264));
#22338=CARTESIAN_POINT('Ctrl Pts',(-0.0125970733164945,-0.0326806104690602,
-0.0106358951915498));
#22339=CARTESIAN_POINT('Ctrl Pts',(-0.012585510544212,-0.0326800046388432,
-0.0106352168632663));
#22340=CARTESIAN_POINT('Ctrl Pts',(-0.012580655196328,-0.0326797515851657,
-0.0106349550473385));
#22341=CARTESIAN_POINT('Ctrl Pts',(-0.0125704036744945,-0.032679220204491,
-0.0106344508415677));
#22342=CARTESIAN_POINT('Ctrl Pts',(-0.0125650073885619,-0.0326789421729556,
-0.0106342138293644));
#22343=CARTESIAN_POINT('Ctrl Pts',(-0.0125503014755309,-0.0326781887991145,
-0.0106336452793051));
#22344=CARTESIAN_POINT('Ctrl Pts',(-0.0125409897741537,-0.0326777164765595,
-0.0106333696974533));
#22345=CARTESIAN_POINT('Ctrl Pts',(-0.0124951126938798,-0.0326754101701503,
-0.0106324276977446));
#22346=CARTESIAN_POINT('Ctrl Pts',(-0.0124585317443909,-0.032673635977473,
-0.0106329770171757));
#22347=CARTESIAN_POINT('Ctrl Pts',(-0.0123352407819245,-0.0326677753268966,
-0.010639217255425));
#22348=CARTESIAN_POINT('Ctrl Pts',(-0.0122490006785074,-0.0326638676144234,
-0.010650928101743));
#22349=CARTESIAN_POINT('Ctrl Pts',(-0.0120777731806125,-0.0326558138624723,
-0.0106891069510247));
#22350=CARTESIAN_POINT('Ctrl Pts',(-0.0119931714857072,-0.0326516763249778,
-0.010715780421183));
#22351=CARTESIAN_POINT('Ctrl Pts',(-0.0118959055696372,-0.0326464650123408,
-0.0107559246356871));
#22352=CARTESIAN_POINT('Ctrl Pts',(-0.0118805854294431,-0.0326456306145429,
-0.0107625405056147));
#22353=CARTESIAN_POINT('Ctrl Pts',(-0.0118565455573148,-0.0326442984126594,
-0.0107733878743638));
#22354=CARTESIAN_POINT('Ctrl Pts',(-0.0118477530101154,-0.0326438062484429,
-0.0107774553779504));
#22355=CARTESIAN_POINT('Ctrl Pts',(-0.0118312840929762,-0.032642874878877,
-0.0107852631448178));
#22356=CARTESIAN_POINT('Ctrl Pts',(-0.0118235993105306,-0.0326424363321358,
-0.0107889848681468));
#22357=CARTESIAN_POINT('Ctrl Pts',(-0.011806333575241,-0.0326414419318973,
-0.010797524265604));
#22358=CARTESIAN_POINT('Ctrl Pts',(-0.0117967712285257,-0.0326408848105252,
-0.0108023783920016));
#22359=CARTESIAN_POINT('Ctrl Pts',(-0.0117679565917114,-0.0326391862427176,
-0.0108173853401912));
#22360=CARTESIAN_POINT('Ctrl Pts',(-0.0117488683643744,-0.0326380339597172,
-0.0108278459002554));
#22361=CARTESIAN_POINT('Ctrl Pts',(-0.0116527594557584,-0.0326320908328485,
-0.0108831898943557));
#22362=CARTESIAN_POINT('Ctrl Pts',(-0.0115795205881838,-0.0326270766925603,
-0.0109342780358299));
#22363=CARTESIAN_POINT('Ctrl Pts',(-0.0114498302371968,-0.0326173926887576,
-0.0110425550282222));
#22364=CARTESIAN_POINT('Ctrl Pts',(-0.0113926136139859,-0.0326127594332519,
-0.0110983945447478));
#22365=CARTESIAN_POINT('Ctrl Pts',(-0.0113243403033009,-0.0326069562425437,
-0.0111762356619507));
#22366=CARTESIAN_POINT('Ctrl Pts',(-0.011309118951816,-0.0326056427589277,
-0.0111944188541949));
#22367=CARTESIAN_POINT('Ctrl Pts',(-0.0112842253070289,-0.0326034706658091,
-0.0112255887597121));
#22368=CARTESIAN_POINT('Ctrl Pts',(-0.011274327606889,-0.0326026002313648,
-0.011238389686991));
#22369=CARTESIAN_POINT('Ctrl Pts',(-0.0112606079694354,-0.032601386695724,
-0.0112567224382293));
#22370=CARTESIAN_POINT('Ctrl Pts',(-0.0112566183136278,-0.0326010329329584,
-0.0112621267918926));
#22371=CARTESIAN_POINT('Ctrl Pts',(-0.0112498020408711,-0.0326004272789098,
-0.0112714873757067));
#22372=CARTESIAN_POINT('Ctrl Pts',(-0.0112469586225496,-0.0326001742499973,
-0.0112754311930397));
#22373=CARTESIAN_POINT('Ctrl Pts',(-0.011240994894217,-0.0325996428275759,
-0.0112837858380411));
#22374=CARTESIAN_POINT('Ctrl Pts',(-0.0112378790635814,-0.0325993647305307,
-0.0112881996758034));
#22375=CARTESIAN_POINT('Ctrl Pts',(-0.0112294507906448,-0.0325986109868777,
-0.0113002731385966));
#22376=CARTESIAN_POINT('Ctrl Pts',(-0.0112241843916177,-0.0325981383650359,
-0.0113079647968963));
#22377=CARTESIAN_POINT('Ctrl Pts',(-0.0111985554069844,-0.032595827662577,
-0.0113461337935123));
#22378=CARTESIAN_POINT('Ctrl Pts',(-0.0111792122399681,-0.0325940496495128,
-0.011377284237655));
#22379=CARTESIAN_POINT('Ctrl Pts',(-0.0111178553037901,-0.0325881885176848,
-0.011484433144876));
#22380=CARTESIAN_POINT('Ctrl Pts',(-0.0110811477855629,-0.0325842833984268,
-0.0115632802324847));
#22381=CARTESIAN_POINT('Ctrl Pts',(-0.0110208009578662,-0.0325762337584024,
-0.0117279086460154));
#22382=CARTESIAN_POINT('Ctrl Pts',(-0.0109975465615405,-0.0325720976757051,
-0.0118134782931668));
#22383=CARTESIAN_POINT('Ctrl Pts',(-0.0109787793125266,-0.0325668880632285,
-0.011916980649851));
#22384=CARTESIAN_POINT('Ctrl Pts',(-0.0109760689136149,-0.0325660537125726,
-0.0119334456987578));
#22385=CARTESIAN_POINT('Ctrl Pts',(-0.0109722078318142,-0.0325647215688092,
-0.0119595342189157));
#22386=CARTESIAN_POINT('Ctrl Pts',(-0.0109708798368436,-0.0325642294147125,
-0.0119691303579224));
#22387=CARTESIAN_POINT('Ctrl Pts',(-0.010968551528085,-0.032563298053641,
-0.0119872068316185));
#22388=CARTESIAN_POINT('Ctrl Pts',(-0.0109675310725281,-0.0325628595051369,
-0.0119956842284084));
#22389=CARTESIAN_POINT('Ctrl Pts',(-0.0109653878181927,-0.0325618650863954,
-0.0120148270245111));
#22390=CARTESIAN_POINT('Ctrl Pts',(-0.0109643057519314,-0.0325613079480914,
-0.0120254964635249));
#22391=CARTESIAN_POINT('Ctrl Pts',(-0.0109614296813406,-0.0325596468470826,
-0.0120571376949412));
#22392=CARTESIAN_POINT('Ctrl Pts',(-0.0109599535229632,-0.0325585329777989,
-0.0120781352913499));
#22393=CARTESIAN_POINT('Ctrl Pts',(-0.0109533742755317,-0.0325514455818761,
-0.0122103330444433));
#22394=CARTESIAN_POINT('Ctrl Pts',(-0.0109598889094037,-0.0325451049800559,
-0.0123217669462785));
#22395=CARTESIAN_POINT('Ctrl Pts',(-0.0109888058462719,-0.0325350650839862,
-0.0124938796035878));
#22396=CARTESIAN_POINT('Ctrl Pts',(-0.0110031091522276,-0.0325314247238606,
-0.0125555465236941));
#22397=CARTESIAN_POINT('Ctrl Pts',(-0.0110271277663615,-0.0325267303830084,
-0.0126362163418378));
#22398=CARTESIAN_POINT('Ctrl Pts',(-0.0110335057639658,-0.032525576563121,
-0.0126561464117112));
#22399=CARTESIAN_POINT('Ctrl Pts',(-0.0110450660151565,-0.0325236403323662,
-0.0126898897568675));
#22400=CARTESIAN_POINT('Ctrl Pts',(-0.0110500445025095,-0.0325228489765341,
-0.0127037694537943));
#22401=CARTESIAN_POINT('Ctrl Pts',(-0.0110574944376209,-0.0325217256783336,
-0.0127236384829956));
#22402=CARTESIAN_POINT('Ctrl Pts',(-0.0110598057005549,-0.0325213850348982,
-0.0127296865662819));
#22403=CARTESIAN_POINT('Ctrl Pts',(-0.0110639068894313,-0.0325207942907258,
-0.0127402192046221));
#22404=CARTESIAN_POINT('Ctrl Pts',(-0.0110656798977015,-0.0325205432059915,
-0.0127447101736816));
#22405=CARTESIAN_POINT('Ctrl Pts',(-0.0110695283732042,-0.0325200073844477,
-0.0127543258374588));
#22406=CARTESIAN_POINT('Ctrl Pts',(-0.0110716103251592,-0.0325197230366926,
-0.0127594477569554));
#22407=CARTESIAN_POINT('Ctrl Pts',(-0.0110773987902469,-0.0325189471285778,
-0.0127734717092702));
#22408=CARTESIAN_POINT('Ctrl Pts',(-0.0110811613476847,-0.0325184588253497,
-0.0127823504991152));
#22409=CARTESIAN_POINT('Ctrl Pts',(-0.0111023185562571,-0.0325157963382542,
-0.0128310021143866));
#22410=CARTESIAN_POINT('Ctrl Pts',(-0.011121303723076,-0.0325137071229543,
-0.0128700654705278));
#22411=CARTESIAN_POINT('Ctrl Pts',(-0.0111808480780025,-0.032507803420902,
-0.0129804745734806));
#22412=CARTESIAN_POINT('Ctrl Pts',(-0.0112254798547442,-0.0325041108284196,
-0.013049453122762));
#22413=CARTESIAN_POINT('Ctrl Pts',(-0.0113276439434469,-0.0324963929152494,
-0.0131827341911131));
#22414=CARTESIAN_POINT('Ctrl Pts',(-0.0113855001258628,-0.0324923704458758,
-0.0132464212615704));
#22415=CARTESIAN_POINT('Ctrl Pts',(-0.011460501472027,-0.0324872934748917,
-0.0133162775856155));
#22416=CARTESIAN_POINT('Ctrl Pts',(-0.011472834962371,-0.0324864629990781,
-0.0133273986525901));
#22417=CARTESIAN_POINT('Ctrl Pts',(-0.0114926307967935,-0.0324851356325864,
-0.0133446773993336));
#22418=CARTESIAN_POINT('Ctrl Pts',(-0.0114999758491315,-0.0324846443105656,
-0.0133509678385413));
#22419=CARTESIAN_POINT('Ctrl Pts',(-0.0115139184607852,-0.032483713644786,
-0.0133626831587809));
#22420=CARTESIAN_POINT('Ctrl Pts',(-0.0115205028986772,-0.0324832749481566,
-0.0133681231268906));
#22421=CARTESIAN_POINT('Ctrl Pts',(-0.0115354762927348,-0.0324822789926153,
-0.013380286176647));
#22422=CARTESIAN_POINT('Ctrl Pts',(-0.011543890970961,-0.0324817204497219,
-0.0133869767671743));
#22423=CARTESIAN_POINT('Ctrl Pts',(-0.011569086375589,-0.0324800511541379,
-0.0134065836508996));
#22424=CARTESIAN_POINT('Ctrl Pts',(-0.0115860633531154,-0.0324789303497482,
-0.0134192426668818));
#22425=CARTESIAN_POINT('Ctrl Pts',(-0.0116915941436823,-0.0324719851637537,
-0.0134946033438365));
#22426=CARTESIAN_POINT('Ctrl Pts',(-0.011786285673404,-0.0324658143181881,
-0.013548160498309));
#22427=CARTESIAN_POINT('Ctrl Pts',(-0.0119456088858079,-0.0324558243318147,
-0.0136172938886583));
#22428=CARTESIAN_POINT('Ctrl Pts',(-0.0120070114391975,-0.0324520667593339,
-0.0136394322758185));
#22429=CARTESIAN_POINT('Ctrl Pts',(-0.0120900727109608,-0.0324472395209694,
-0.0136635567748357));
#22430=CARTESIAN_POINT('Ctrl Pts',(-0.0121106345482471,-0.0324460649912443,
-0.0136690701732354));
#22431=CARTESIAN_POINT('Ctrl Pts',(-0.0121458068770551,-0.0324440979176854,
-0.0136777252120749));
#22432=CARTESIAN_POINT('Ctrl Pts',(-0.0121603606636426,-0.0324432960755124,
-0.0136810832366418));
#22433=CARTESIAN_POINT('Ctrl Pts',(-0.0121813230510829,-0.0324421607483455,
-0.0136856004017363));
#22434=CARTESIAN_POINT('Ctrl Pts',(-0.0121876934003862,-0.0324418183126306,
-0.0136869310279051));
#22435=CARTESIAN_POINT('Ctrl Pts',(-0.0121988085144354,-0.0324412255542373,
-0.013689179438025));
#22436=CARTESIAN_POINT('Ctrl Pts',(-0.0122035494616066,-0.0324409742265764,
-0.0136901152956575));
#22437=CARTESIAN_POINT('Ctrl Pts',(-0.0122137054581072,-0.0324404391109127,
-0.0136920705514625));
#22438=CARTESIAN_POINT('Ctrl Pts',(-0.0122191216327169,-0.0324401556984485,
-0.0136930832308128));
#22439=CARTESIAN_POINT('Ctrl Pts',(-0.0122339492827184,-0.0324393848949003,
-0.0136957734827298));
#22440=CARTESIAN_POINT('Ctrl Pts',(-0.0122433712510885,-0.0324389006907258,
-0.0136973926652461));
#22441=CARTESIAN_POINT('Ctrl Pts',(-0.0122941413774278,-0.0324363186966429,
-0.0137056325802603));
#22442=CARTESIAN_POINT('Ctrl Pts',(-0.0123357340323474,-0.0324342998576002,
-0.0137106560996469));
#22443=CARTESIAN_POINT('Ctrl Pts',(-0.0124603304710097,-0.0324284066491825,
-0.0137205806679845));
#22444=CARTESIAN_POINT('Ctrl Pts',(-0.0125435793494546,-0.0324246660088853,
-0.0137204756885645));
#22445=CARTESIAN_POINT('Ctrl Pts',(-0.0127051396550983,-0.0324172177402809,
-0.0137071944590896));
#22446=CARTESIAN_POINT('Ctrl Pts',(-0.012783243030385,-0.0324135277774321,
-0.0136946883165602));
#22447=CARTESIAN_POINT('Ctrl Pts',(-0.0128804727332715,-0.0324086174898915,
-0.0136713568852446));
#22448=CARTESIAN_POINT('Ctrl Pts',(-0.0129008019995967,-0.0324075733750139,
-0.0136660372410511));
#22449=CARTESIAN_POINT('Ctrl Pts',(-0.0129311921174884,-0.0324059835165886,
-0.0136574180833613));
#22450=CARTESIAN_POINT('Ctrl Pts',(-0.0129413384001461,-0.0324054478030911,
-0.0136544273626967));
#22451=CARTESIAN_POINT('Ctrl Pts',(-0.0129596066641425,-0.0324044740507557,
-0.0136488378149771));
#22452=CARTESIAN_POINT('Ctrl Pts',(-0.0129677394254137,-0.0324040372284005,
-0.0136462755159603));
#22453=CARTESIAN_POINT('Ctrl Pts',(-0.0129851617722922,-0.0324030941378602,
-0.0136406272856353));
#22454=CARTESIAN_POINT('Ctrl Pts',(-0.0129944440342363,-0.0324025871806956,
-0.0136375201106764));
#22455=CARTESIAN_POINT('Ctrl Pts',(-0.0130194928668625,-0.0324012066730194,
-0.0136288692764909));
#22456=CARTESIAN_POINT('Ctrl Pts',(-0.0130351996469986,-0.0324003275702542,
-0.0136231575440893));
#22457=CARTESIAN_POINT('Ctrl Pts',(-0.0131324138541097,-0.0323948006898061,
-0.0135860069610628));
#22458=CARTESIAN_POINT('Ctrl Pts',(-0.0132112105052648,-0.0323899285015497,
-0.013547952614839));
#22459=CARTESIAN_POINT('Ctrl Pts',(-0.0133619244911491,-0.03237992469363,
-0.0134586819281539));
#22460=CARTESIAN_POINT('Ctrl Pts',(-0.0134335328699816,-0.0323748114634214,
-0.0134075511645289));
#22461=CARTESIAN_POINT('Ctrl Pts',(-0.013519319976915,-0.0323684844588378,
-0.0133344961086026));
#22462=CARTESIAN_POINT('Ctrl Pts',(-0.0135378465294945,-0.0323671054819359,
-0.0133179308216092));
#22463=CARTESIAN_POINT('Ctrl Pts',(-0.0135681763908311,-0.0323648378633378,
-0.01328946392179));
#22464=CARTESIAN_POINT('Ctrl Pts',(-0.0135802002123302,-0.0323639361143729,
-0.0132778047351143));
#22465=CARTESIAN_POINT('Ctrl Pts',(-0.0135968426480222,-0.0323626871381552,
-0.0132611327743329));
#22466=CARTESIAN_POINT('Ctrl Pts',(-0.0136016211373579,-0.0323623284236823,
-0.0132562820136126));
#22467=CARTESIAN_POINT('Ctrl Pts',(-0.013609766483034,-0.0323617170548982,
-0.0132479032535201));
#22468=CARTESIAN_POINT('Ctrl Pts',(-0.0136131489844963,-0.032361463204849,
-0.0132443906603794));
#22469=CARTESIAN_POINT('Ctrl Pts',(-0.0136202154902349,-0.0323609330336838,
-0.0132369824026247));
#22470=CARTESIAN_POINT('Ctrl Pts',(-0.0136238959011567,-0.0323606569774543,
-0.0132330835124756));
#22471=CARTESIAN_POINT('Ctrl Pts',(-0.0136337905808048,-0.0323599147417337,
-0.0132224913961231));
#22472=CARTESIAN_POINT('Ctrl Pts',(-0.0136399659577281,-0.0323594514325772,
-0.013215761953922));
#22473=CARTESIAN_POINT('Ctrl Pts',(-0.0136691515799494,-0.0323572591902006,
-0.0131833853204877));
#22474=CARTESIAN_POINT('Ctrl Pts',(-0.0136913596375806,-0.032355583205021,
-0.0131570254128175));
#22475=CARTESIAN_POINT('Ctrl Pts',(-0.0137673233547661,-0.0323497331482562,
-0.0130604738930858));
#22476=CARTESIAN_POINT('Ctrl Pts',(-0.0138159115028095,-0.0323457577434689,
-0.0129864338199178));
#22477=CARTESIAN_POINT('Ctrl Pts',(-0.0139003702802725,-0.0323375961407567,
-0.012829926416516));
#22478=CARTESIAN_POINT('Ctrl Pts',(-0.0139359188354758,-0.0323334200739767,
-0.0127476779122721));
#22479=CARTESIAN_POINT('Ctrl Pts',(-0.0139694163163981,-0.0323281637173709,
-0.0126469625995437));
#22480=CARTESIAN_POINT('Ctrl Pts',(-0.0139744325090918,-0.032327328093665,
-0.0126310203375714));
#22481=CARTESIAN_POINT('Ctrl Pts',(-0.0139819473688683,-0.0323259943803933,
-0.0126057078580092));
#22482=CARTESIAN_POINT('Ctrl Pts',(-0.0139846184244454,-0.0323255019530356,
-0.0125963899495029));
#22483=CARTESIAN_POINT('Ctrl Pts',(-0.0139894767132811,-0.0323245703622555,
-0.0125788185640078));
#22484=CARTESIAN_POINT('Ctrl Pts',(-0.0139916835854576,-0.0323241318610183,
-0.0125705708706653));
#22485=CARTESIAN_POINT('Ctrl Pts',(-0.0139965056315262,-0.0323231379402778,
-0.0125519313608952));
#22486=CARTESIAN_POINT('Ctrl Pts',(-0.0139990812110588,-0.0323225812578732,
-0.0125415298349163));
#22487=CARTESIAN_POINT('Ctrl Pts',(-0.0140063846163501,-0.0323209228120207,
-0.0125106601955618));
#22488=CARTESIAN_POINT('Ctrl Pts',(-0.014010802899698,-0.0323198111887906,
-0.0124901219903299));
#22489=CARTESIAN_POINT('Ctrl Pts',(-0.0140335651968874,-0.0323134072121081,
-0.0123727010909512));
#22490=CARTESIAN_POINT('Ctrl Pts',(-0.0140430000022424,-0.032307835615159,
-0.0122743679938294));
#22491=CARTESIAN_POINT('Ctrl Pts',(-0.014043,-0.0323021764244909,-0.0121758532514363));
#22492=CARTESIAN_POINT('',(-0.0140429999980935,-0.0329194527355552,-0.0121757765831131));
#22493=CARTESIAN_POINT('Ctrl Pts',(-0.014043,-0.0324174341340783,-0.0121758532962676));
#22494=CARTESIAN_POINT('Ctrl Pts',(-0.0140429999999617,-0.0324177808943133,
-0.0121819461576369));
#22495=CARTESIAN_POINT('Ctrl Pts',(-0.0140429639115131,-0.0324181282307381,
-0.0121880396273339));
#22496=CARTESIAN_POINT('Ctrl Pts',(-0.0140419046234089,-0.0324232318073101,
-0.0122774465068135));
#22497=CARTESIAN_POINT('Ctrl Pts',(-0.0140341711796612,-0.0324280773472333,
-0.0123605416903952));
#22498=CARTESIAN_POINT('Ctrl Pts',(-0.0140125876239106,-0.0324351230456924,
-0.0124835094666267));
#22499=CARTESIAN_POINT('Ctrl Pts',(-0.0140037591473482,-0.0324374264332629,
-0.0125241098010196));
#22500=CARTESIAN_POINT('Ctrl Pts',(-0.0139908971430643,-0.0324401636230692,
-0.012573554180475));
#22501=CARTESIAN_POINT('Ctrl Pts',(-0.0139884058274866,-0.032440671318938,
-0.0125827788251411));
#22502=CARTESIAN_POINT('Ctrl Pts',(-0.0139843394442716,-0.0324414650629874,
-0.0125972983218125));
#22503=CARTESIAN_POINT('Ctrl Pts',(-0.0139828213964599,-0.0324417542309827,
-0.0126026087336661));
#22504=CARTESIAN_POINT('Ctrl Pts',(-0.013979914969254,-0.0324422945272259,
-0.0126125731846274));
#22505=CARTESIAN_POINT('Ctrl Pts',(-0.0139785331325594,-0.032442546001343,
-0.0126172288203762));
#22506=CARTESIAN_POINT('Ctrl Pts',(-0.0139752332176127,-0.0324431341391227,
-0.0126281573643367));
#22507=CARTESIAN_POINT('Ctrl Pts',(-0.0139732970943684,-0.032443469753171,
-0.0126344246548958));
#22508=CARTESIAN_POINT('Ctrl Pts',(-0.0139667605406211,-0.0324445727557668,
-0.0126551149007491));
#22509=CARTESIAN_POINT('Ctrl Pts',(-0.013961987693389,-0.032445330713125,
-0.0126694828998101));
#22510=CARTESIAN_POINT('Ctrl Pts',(-0.0139498766783522,-0.0324471490320271,
-0.0127042238135634));
#22511=CARTESIAN_POINT('Ctrl Pts',(-0.0139423195314849,-0.0324481990344315,
-0.0127245173354993));
#22512=CARTESIAN_POINT('Ctrl Pts',(-0.0139095917812991,-0.0324524441066034,
-0.0128070476695066));
#22513=CARTESIAN_POINT('Ctrl Pts',(-0.0138807987633129,-0.0324555106095279,
-0.0128677717206334));
#22514=CARTESIAN_POINT('Ctrl Pts',(-0.0137967414498903,-0.0324634090795341,
-0.0130187504035597));
#22515=CARTESIAN_POINT('Ctrl Pts',(-0.0137360007520845,-0.0324682410838825,
-0.0131055380670655));
#22516=CARTESIAN_POINT('Ctrl Pts',(-0.0136529287288984,-0.0324744695459774,
-0.0132015522961771));
#22517=CARTESIAN_POINT('Ctrl Pts',(-0.013638653784388,-0.0324755274946351,
-0.0132173765057506));
#22518=CARTESIAN_POINT('Ctrl Pts',(-0.0136166542635667,-0.0324771425786297,
-0.0132407706529972));
#22519=CARTESIAN_POINT('Ctrl Pts',(-0.0136091700568949,-0.0324776894577568,
-0.0132485636476857));
#22520=CARTESIAN_POINT('Ctrl Pts',(-0.0135955978805996,-0.0324786769642786,
-0.0132624018944978));
#22521=CARTESIAN_POINT('Ctrl Pts',(-0.0135895401288239,-0.0324791162537408,
-0.0132684762302694));
#22522=CARTESIAN_POINT('Ctrl Pts',(-0.0135765197807536,-0.0324800575018689,
-0.0132813162702421));
#22523=CARTESIAN_POINT('Ctrl Pts',(-0.0135695433750145,-0.0324805600743814,
-0.0132880673890639));
#22524=CARTESIAN_POINT('Ctrl Pts',(-0.0135504227140547,-0.0324819330113688,
-0.0133062243259164));
#22525=CARTESIAN_POINT('Ctrl Pts',(-0.0135381569252161,-0.0324828089250301,
-0.0133174997878952));
#22526=CARTESIAN_POINT('Ctrl Pts',(-0.0134613172970779,-0.0324882683933732,
-0.013385873039758));
#22527=CARTESIAN_POINT('Ctrl Pts',(-0.0133922442729897,-0.0324930702459721,
-0.0134376675824383));
#22528=CARTESIAN_POINT('Ctrl Pts',(-0.0132491825625166,-0.0325027046666989,
-0.0135272987180643));
#22529=CARTESIAN_POINT('Ctrl Pts',(-0.0131757362757509,-0.0325075102839964,
-0.013565479022581));
#22530=CARTESIAN_POINT('Ctrl Pts',(-0.0130604591241145,-0.0325145767457728,
-0.0136140944927583));
#22531=CARTESIAN_POINT('Ctrl Pts',(-0.0130206644780057,-0.0325169340987139,
-0.0136289744986511));
#22532=CARTESIAN_POINT('Ctrl Pts',(-0.0129711636299716,-0.0325197253521151,
-0.0136451886263051));
#22533=CARTESIAN_POINT('Ctrl Pts',(-0.0129619953984455,-0.0325202364941967,
-0.0136480970733859));
#22534=CARTESIAN_POINT('Ctrl Pts',(-0.0129475067367539,-0.0325210344126728,
-0.0136525446501887));
#22535=CARTESIAN_POINT('Ctrl Pts',(-0.0129422043352802,-0.0325213243611548,
-0.0136541411443886));
#22536=CARTESIAN_POINT('Ctrl Pts',(-0.0129322388107494,-0.0325218652763522,
-0.0136570832362048));
#22537=CARTESIAN_POINT('Ctrl Pts',(-0.0129275779324979,-0.0325221165992554,
-0.0136584353804902));
#22538=CARTESIAN_POINT('Ctrl Pts',(-0.0129166273318506,-0.0325227032802055,
-0.0136615562690325));
#22539=CARTESIAN_POINT('Ctrl Pts',(-0.012910332668483,-0.0325230376050304,
-0.0136633070807751));
#22540=CARTESIAN_POINT('Ctrl Pts',(-0.0128895613395232,-0.0325241318068259,
-0.0136689425739873));
#22541=CARTESIAN_POINT('Ctrl Pts',(-0.0128750387855278,-0.0325248824584113,
-0.0136726564126512));
#22542=CARTESIAN_POINT('Ctrl Pts',(-0.0128396904560963,-0.0325266798456656,
-0.0136811492180981));
#22543=CARTESIAN_POINT('Ctrl Pts',(-0.0128188147461368,-0.0325277165349856,
-0.013685708470305));
#22544=CARTESIAN_POINT('Ctrl Pts',(-0.0127335509036351,-0.0325318742835031,
-0.013702482713648));
#22545=CARTESIAN_POINT('Ctrl Pts',(-0.0126685072039677,-0.0325348720916436,
-0.0137110241936687));
#22546=CARTESIAN_POINT('Ctrl Pts',(-0.0124954567473541,-0.0325428006478178,
-0.0137226145925197));
#22547=CARTESIAN_POINT('Ctrl Pts',(-0.0123873503650151,-0.0325477264178684,
-0.0137185129836419));
#22548=CARTESIAN_POINT('Ctrl Pts',(-0.0122595450338619,-0.0325540614977239,
-0.0137001502063682));
#22549=CARTESIAN_POINT('Ctrl Pts',(-0.0122385965895038,-0.0325551155661509,
-0.0136966977535008));
#22550=CARTESIAN_POINT('Ctrl Pts',(-0.0122071204858661,-0.0325567258693322,
-0.013690840737277));
#22551=CARTESIAN_POINT('Ctrl Pts',(-0.0121965354970523,-0.0325572719404621,
-0.0136887560175417));
#22552=CARTESIAN_POINT('Ctrl Pts',(-0.0121775757708738,-0.0325582585679991,
-0.0136848149109564));
#22553=CARTESIAN_POINT('Ctrl Pts',(-0.012169192949372,-0.0325586977965608,
-0.0136829993507281));
#22554=CARTESIAN_POINT('Ctrl Pts',(-0.0121513448073806,-0.032559639548806,
-0.0136789777025424));
#22555=CARTESIAN_POINT('Ctrl Pts',(-0.0121418843504614,-0.0325601426934379,
-0.0136767518937284));
#22556=CARTESIAN_POINT('Ctrl Pts',(-0.0121162167577163,-0.0325615188373242,
-0.0136704564597074));
#22557=CARTESIAN_POINT('Ctrl Pts',(-0.0121000540087729,-0.0325623974296017,
-0.01366621277227));
#22558=CARTESIAN_POINT('Ctrl Pts',(-0.0119994044083191,-0.0325679458533994,
-0.0136380310854544));
#22559=CARTESIAN_POINT('Ctrl Pts',(-0.0119170322623532,-0.0325728428169011,
-0.0136071829817816));
#22560=CARTESIAN_POINT('Ctrl Pts',(-0.0117604114638662,-0.0325827462484919,
-0.0135327570164667));
#22561=CARTESIAN_POINT('Ctrl Pts',(-0.011686276429226,-0.0325877277857869,
-0.0134896390262423));
#22562=CARTESIAN_POINT('Ctrl Pts',(-0.0115847225035555,-0.0325946982489978,
-0.0134186652507507));
#22563=CARTESIAN_POINT('Ctrl Pts',(-0.0115541690903881,-0.0325968149861419,
-0.0133955740710582));
#22564=CARTESIAN_POINT('Ctrl Pts',(-0.0115171739800513,-0.0325993714889418,
-0.0133653874487364));
#22565=CARTESIAN_POINT('Ctrl Pts',(-0.0115098986709613,-0.032599873897062,
-0.0133593387640804));
#22566=CARTESIAN_POINT('Ctrl Pts',(-0.0114985226211263,-0.0326006582991061,
-0.0133497023973405));
#22567=CARTESIAN_POINT('Ctrl Pts',(-0.0114943845729975,-0.0326009433737483,
-0.0133461593533875));
#22568=CARTESIAN_POINT('Ctrl Pts',(-0.0114865776302015,-0.0326014805723252,
-0.013339402978093));
#22569=CARTESIAN_POINT('Ctrl Pts',(-0.0114829051272995,-0.0326017329928445,
-0.0133361941004829));
#22570=CARTESIAN_POINT('Ctrl Pts',(-0.0114742191309836,-0.0326023294453778,
-0.0133285317221074));
#22571=CARTESIAN_POINT('Ctrl Pts',(-0.0114692192928218,-0.0326026723406502,
-0.0133240628074794));
#22572=CARTESIAN_POINT('Ctrl Pts',(-0.0114523844923257,-0.0326038260397585,
-0.0133088170751233));
#22573=CARTESIAN_POINT('Ctrl Pts',(-0.0114406877850518,-0.0326046261807342,
-0.013297888431824));
#22574=CARTESIAN_POINT('Ctrl Pts',(-0.0114123585830405,-0.0326065666939424,
-0.0132705815181657));
#22575=CARTESIAN_POINT('Ctrl Pts',(-0.0113959233188129,-0.0326076947734705,
-0.0132540037973761));
#22576=CARTESIAN_POINT('Ctrl Pts',(-0.0113267243139725,-0.0326124874498326,
-0.0131809624494235));
#22577=CARTESIAN_POINT('Ctrl Pts',(-0.0112778649772784,-0.0326159879599315,
-0.0131209498722869));
#22578=CARTESIAN_POINT('Ctrl Pts',(-0.0111811589440617,-0.0326237311146279,
-0.0129820567978842));
#22579=CARTESIAN_POINT('Ctrl Pts',(-0.011135467511743,-0.0326279798353588,
-0.0129020453472362));
#22580=CARTESIAN_POINT('Ctrl Pts',(-0.0110880260708171,-0.0326335643731067,
-0.0127984776858735));
#22581=CARTESIAN_POINT('Ctrl Pts',(-0.0110793058263517,-0.0326346545212671,
-0.0127783145082686));
#22582=CARTESIAN_POINT('Ctrl Pts',(-0.0110669486024995,-0.0326363019531987,
-0.012747980119422));
#22583=CARTESIAN_POINT('Ctrl Pts',(-0.0110629829701518,-0.0326368481040948,
-0.0127379453333044));
#22584=CARTESIAN_POINT('Ctrl Pts',(-0.0110560543977237,-0.0326378348183345,
-0.0127198603339765));
#22585=CARTESIAN_POINT('Ctrl Pts',(-0.0110530527060399,-0.0326382740528369,
-0.0127118253889376));
#22586=CARTESIAN_POINT('Ctrl Pts',(-0.0110467934629567,-0.0326392157549688,
-0.0126946347371269));
#22587=CARTESIAN_POINT('Ctrl Pts',(-0.0110435551126964,-0.032639718842843,
-0.0126854724749631));
#22588=CARTESIAN_POINT('Ctrl Pts',(-0.0110349857874414,-0.0326410946685077,
-0.0126604783112454));
#22589=CARTESIAN_POINT('Ctrl Pts',(-0.0110298251291063,-0.0326419729949649,
-0.0126445897550293));
#22590=CARTESIAN_POINT('Ctrl Pts',(-0.0109992051731233,-0.0326475123413992,
-0.0125448326862552));
#22591=CARTESIAN_POINT('Ctrl Pts',(-0.010980676026657,-0.0326523995820292,
-0.012459017216906));
#22592=CARTESIAN_POINT('Ctrl Pts',(-0.0109586794845246,-0.0326622760399338,
-0.0122874761640966));
#22593=CARTESIAN_POINT('Ctrl Pts',(-0.010954865690689,-0.0326672401449363,
-0.0122020950875256));
#22594=CARTESIAN_POINT('Ctrl Pts',(-0.0109596091936112,-0.0326742203875233,
-0.0120781663327876));
#22595=CARTESIAN_POINT('Ctrl Pts',(-0.0109625437130375,-0.0326763610460147,
-0.0120395624830163));
#22596=CARTESIAN_POINT('Ctrl Pts',(-0.0109680016151335,-0.0326789416044001,
-0.0119916794927017));
#22597=CARTESIAN_POINT('Ctrl Pts',(-0.0109691632003269,-0.0326794455302104,
-0.0119822616048896));
#22598=CARTESIAN_POINT('Ctrl Pts',(-0.0109711290972703,-0.0326802317568371,
-0.0119674486216061));
#22599=CARTESIAN_POINT('Ctrl Pts',(-0.0109718752432203,-0.0326805171613873,
-0.0119620461980114));
#22600=CARTESIAN_POINT('Ctrl Pts',(-0.0109733426014132,-0.0326810545994463,
-0.011951822142272));
#22601=CARTESIAN_POINT('Ctrl Pts',(-0.0109740580350851,-0.0326813069339909,
-0.0119469998700646));
#22602=CARTESIAN_POINT('Ctrl Pts',(-0.0109758099470793,-0.0326819026710148,
-0.0119355649553286));
#22603=CARTESIAN_POINT('Ctrl Pts',(-0.0109768666299908,-0.0326822449446563,
-0.0119289554536394));
#22604=CARTESIAN_POINT('Ctrl Pts',(-0.0109805835797715,-0.0326833942479967,
-0.0119066386306476));
#22605=CARTESIAN_POINT('Ctrl Pts',(-0.0109834441573704,-0.0326841907247585,
-0.0118909652339224));
#22606=CARTESIAN_POINT('Ctrl Pts',(-0.0109910637827476,-0.032686120532288,
-0.0118525912815925));
#22607=CARTESIAN_POINT('Ctrl Pts',(-0.0109960929496927,-0.0326872417471431,
-0.0118299479481645));
#22608=CARTESIAN_POINT('Ctrl Pts',(-0.0110198547796943,-0.032691983580424,
-0.0117333102471039));
#22609=CARTESIAN_POINT('Ctrl Pts',(-0.0110435536591722,-0.0326954435644003,
-0.01166064502976));
#22610=CARTESIAN_POINT('Ctrl Pts',(-0.0111079724699095,-0.0327032047436342,
-0.0115036770522244));
#22611=CARTESIAN_POINT('Ctrl Pts',(-0.0111511710667793,-0.0327075133650244,
-0.0114207241683673));
#22612=CARTESIAN_POINT('Ctrl Pts',(-0.0112134049155082,-0.0327131612647455,
-0.0113237970705941));
#22613=CARTESIAN_POINT('Ctrl Pts',(-0.011225602763543,-0.0327142461164853,
-0.0113056588654261));
#22614=CARTESIAN_POINT('Ctrl Pts',(-0.0112443793212655,-0.0327158870886356,
-0.0112789800078663));
#22615=CARTESIAN_POINT('Ctrl Pts',(-0.0112506691681248,-0.0327164322079441,
-0.0112702388919093));
#22616=CARTESIAN_POINT('Ctrl Pts',(-0.0112621311625699,-0.0327174178021129,
-0.0112546566306558));
#22617=CARTESIAN_POINT('Ctrl Pts',(-0.0112672698573007,-0.0327178569610101,
-0.0112477913657454));
#22618=CARTESIAN_POINT('Ctrl Pts',(-0.0112783615668921,-0.0327187993171647,
-0.0112332275715205));
#22619=CARTESIAN_POINT('Ctrl Pts',(-0.0112843307023872,-0.0327193031438145,
-0.011225541836087));
#22620=CARTESIAN_POINT('Ctrl Pts',(-0.0113007828619445,-0.0327206831129039,
-0.0112047670588319));
#22621=CARTESIAN_POINT('Ctrl Pts',(-0.0113114069942638,-0.0327215649008488,
-0.0111917918847195));
#22622=CARTESIAN_POINT('Ctrl Pts',(-0.0113803126264655,-0.0327272273863249,
-0.0111103820167889));
#22623=CARTESIAN_POINT('Ctrl Pts',(-0.0114442609884801,-0.0327322468603228,
-0.0110469866249132));
#22624=CARTESIAN_POINT('Ctrl Pts',(-0.0115819114031304,-0.0327424810909635,
-0.0109325055699087));
#22625=CARTESIAN_POINT('Ctrl Pts',(-0.0116552824548097,-0.0327476727498928,
-0.010881537712132));
#22626=CARTESIAN_POINT('Ctrl Pts',(-0.0117615386664768,-0.0327545259767972,
-0.0108206289413296));
#22627=CARTESIAN_POINT('Ctrl Pts',(-0.0117909630646408,-0.0327563581860617,
-0.010805004976924));
#22628=CARTESIAN_POINT('Ctrl Pts',(-0.0118290012093397,-0.0327586233443108,
-0.0107863600026639));
#22629=CARTESIAN_POINT('Ctrl Pts',(-0.0118371656007931,-0.0327591036113302,
-0.0107824468383063));
#22630=CARTESIAN_POINT('Ctrl Pts',(-0.0118502163364397,-0.0327598613609656,
-0.0107763323319675));
#22631=CARTESIAN_POINT('Ctrl Pts',(-0.0118550804041916,-0.032760141596235,
-0.0107740842512208));
#22632=CARTESIAN_POINT('Ctrl Pts',(-0.0118644225726241,-0.0327606755157795,
-0.0107698253961913));
#22633=CARTESIAN_POINT('Ctrl Pts',(-0.0118688986597354,-0.0327609294298043,
-0.0107678106049485));
#22634=CARTESIAN_POINT('Ctrl Pts',(-0.0118796947980605,-0.0327615374383849,
-0.0107630128345269));
#22635=CARTESIAN_POINT('Ctrl Pts',(-0.0118860241395326,-0.0327618902689997,
-0.0107602508237543));
#22636=CARTESIAN_POINT('Ctrl Pts',(-0.0119082266795699,-0.03276311603792,
-0.0107507389588601));
#22637=CARTESIAN_POINT('Ctrl Pts',(-0.0119241948405835,-0.032763976425662,
-0.01074421262814));
#22638=CARTESIAN_POINT('Ctrl Pts',(-0.0119643539121354,-0.0327660955354746,
-0.0107285799143478));
#22639=CARTESIAN_POINT('Ctrl Pts',(-0.0119886709526783,-0.0327673388034294,
-0.01071981081942));
#22640=CARTESIAN_POINT('Ctrl Pts',(-0.0121037832715948,-0.032773087197665,
-0.0106815393746914));
#22641=CARTESIAN_POINT('Ctrl Pts',(-0.0121969719264597,-0.0327773579174847,
-0.0106598923281588));
#22642=CARTESIAN_POINT('Ctrl Pts',(-0.0123691074703633,-0.0327853693868554,
-0.0106364247099558));
#22643=CARTESIAN_POINT('Ctrl Pts',(-0.012447332898459,-0.032789053757119,
-0.0106317685655158));
#22644=CARTESIAN_POINT('Ctrl Pts',(-0.0125421513020828,-0.0327937494306661,
-0.0106333399669067));
#22645=CARTESIAN_POINT('Ctrl Pts',(-0.0125587284274799,-0.0327945785354581,
-0.0106338821394445));
#22646=CARTESIAN_POINT('Ctrl Pts',(-0.0125850671367133,-0.0327959101214111,
-0.0106351689126419));
#22647=CARTESIAN_POINT('Ctrl Pts',(-0.0125948361536064,-0.032796407125762,
-0.0106357393764921));
#22648=CARTESIAN_POINT('Ctrl Pts',(-0.0126130664320088,-0.0327973406722879,
-0.0106369780442519));
#22649=CARTESIAN_POINT('Ctrl Pts',(-0.0126215289170978,-0.0327977764707723,
-0.0106376232166725));
#22650=CARTESIAN_POINT('Ctrl Pts',(-0.0126405959430574,-0.0327987640530906,
-0.0106392351927735));
#22651=CARTESIAN_POINT('Ctrl Pts',(-0.012651196591259,-0.0327993170826376,
-0.0106402420178862));
#22652=CARTESIAN_POINT('Ctrl Pts',(-0.0126829024536885,-0.0328009833492266,
-0.0106435848497243));
#22653=CARTESIAN_POINT('Ctrl Pts',(-0.0127039701414622,-0.0328021067835447,
-0.0106462468042387));
#22654=CARTESIAN_POINT('Ctrl Pts',(-0.0128046186569758,-0.0328075536333466,
-0.010661080274502));
#22655=CARTESIAN_POINT('Ctrl Pts',(-0.0128832112915167,-0.0328120562245261,
-0.0106790312885555));
#22656=CARTESIAN_POINT('Ctrl Pts',(-0.0130421918661889,-0.0328215700421989,
-0.0107286888424951));
#22657=CARTESIAN_POINT('Ctrl Pts',(-0.0131220551897563,-0.0328265784254938,
-0.0107611786217417));
#22658=CARTESIAN_POINT('Ctrl Pts',(-0.0132322551602566,-0.0328335270169368,
-0.0108171553750811));
#22659=CARTESIAN_POINT('Ctrl Pts',(-0.0132650886670807,-0.0328356007848239,
-0.0108353692798452));
#22660=CARTESIAN_POINT('Ctrl Pts',(-0.0133052833941123,-0.0328381139623187,
-0.0108596252708577));
#22661=CARTESIAN_POINT('Ctrl Pts',(-0.0133132949983306,-0.0328386135641192,
-0.0108645604937411));
#22662=CARTESIAN_POINT('Ctrl Pts',(-0.0133258634042756,-0.0328393945915308,
-0.0108724622515164));
#22663=CARTESIAN_POINT('Ctrl Pts',(-0.0133304504072629,-0.0328396790554818,
-0.0108753800359229));
#22664=CARTESIAN_POINT('Ctrl Pts',(-0.0133391259879381,-0.032840215815753,
-0.010880963177334));
#22665=CARTESIAN_POINT('Ctrl Pts',(-0.0133432174288135,-0.0328404684003856,
-0.0108836237455743));
#22666=CARTESIAN_POINT('Ctrl Pts',(-0.0133529201297948,-0.0328410661999849,
-0.0108899988878199));
#22667=CARTESIAN_POINT('Ctrl Pts',(-0.013358519897868,-0.0328414102633424,
-0.010893730877907));
#22668=CARTESIAN_POINT('Ctrl Pts',(-0.0133774740956578,-0.032842572257485,
-0.0109065428477252));
#22669=CARTESIAN_POINT('Ctrl Pts',(-0.0133907107283158,-0.0328433793163547,
-0.0109157960593147));
#22670=CARTESIAN_POINT('Ctrl Pts',(-0.0134229456072659,-0.0328453400896089,
-0.0109390920326783));
#22671=CARTESIAN_POINT('Ctrl Pts',(-0.0134417716285728,-0.0328464811728091,
-0.0109533667694848));
#22672=CARTESIAN_POINT('Ctrl Pts',(-0.0135221867171937,-0.0328513717640358,
-0.0110173017218181));
#22673=CARTESIAN_POINT('Ctrl Pts',(-0.0135802355540582,-0.0328549504506304,
-0.0110712266880717));
#22674=CARTESIAN_POINT('Ctrl Pts',(-0.013700364442488,-0.0328630579585532,
-0.0112013896027806));
#22675=CARTESIAN_POINT('Ctrl Pts',(-0.013759813755502,-0.0328676008757561,
-0.0112795715416857));
#22676=CARTESIAN_POINT('Ctrl Pts',(-0.0138202878194713,-0.0328732816843213,
-0.0113771226022248));
#22677=CARTESIAN_POINT('Ctrl Pts',(-0.013828896551105,-0.0328741203482622,
-0.0113915290162322));
#22678=CARTESIAN_POINT('Ctrl Pts',(-0.0138421723004847,-0.032875463821008,
-0.0114145917419387));
#22679=CARTESIAN_POINT('Ctrl Pts',(-0.0138469946144851,-0.0328759629805441,
-0.0114231573810236));
#22680=CARTESIAN_POINT('Ctrl Pts',(-0.0138558645071177,-0.0328769025759237,
-0.0114392707862286));
#22681=CARTESIAN_POINT('Ctrl Pts',(-0.0138599317404098,-0.0328773422814102,
-0.0114468073353758));
#22682=CARTESIAN_POINT('Ctrl Pts',(-0.013868904590534,-0.0328783326456948,
-0.0114637703285601));
#22683=CARTESIAN_POINT('Ctrl Pts',(-0.013873775959069,-0.0328788844954938,
-0.0114732143154514));
#22684=CARTESIAN_POINT('Ctrl Pts',(-0.0138880372903935,-0.0328805435929272,
-0.0115015776912613));
#22685=CARTESIAN_POINT('Ctrl Pts',(-0.0138971364804514,-0.0328816609083075,
-0.0115206398151141));
#22686=CARTESIAN_POINT('Ctrl Pts',(-0.0139386436631161,-0.032887051523899,
-0.0116123931994035));
#22687=CARTESIAN_POINT('Ctrl Pts',(-0.0139657830044827,-0.0328914997311912,
-0.0116873245635427));
#22688=CARTESIAN_POINT('Ctrl Pts',(-0.0140183362770819,-0.0329027411556628,
-0.0118770741745044));
#22689=CARTESIAN_POINT('Ctrl Pts',(-0.0140366543374166,-0.0329096254192521,
-0.0119933458369967));
#22690=CARTESIAN_POINT('Ctrl Pts',(-0.0140422074617452,-0.0329167382459104,
-0.0121244821376552));
#22691=CARTESIAN_POINT('Ctrl Pts',(-0.0140426082344107,-0.0329174845899751,
-0.0121384004940174));
#22692=CARTESIAN_POINT('Ctrl Pts',(-0.0140428857751294,-0.0329184474911976,
-0.012156597996416));
#22693=CARTESIAN_POINT('Ctrl Pts',(-0.0140429332088814,-0.0329186727920838,
-0.0121608734644583));
#22694=CARTESIAN_POINT('Ctrl Pts',(-0.0140429874690276,-0.032919083176937,
-0.012168694850362));
#22695=CARTESIAN_POINT('Ctrl Pts',(-0.0140429998218256,-0.0329192680377374,
-0.0121722307005113));
#22696=CARTESIAN_POINT('Ctrl Pts',(-0.0140429999980935,-0.0329194527355552,
-0.0121757765831131));
#22697=CARTESIAN_POINT('Ctrl Pts',(-0.0140429999975648,-0.0329194522153789,
-0.0121757665966515));
#22698=CARTESIAN_POINT('Ctrl Pts',(-0.0140429999990012,-0.032919453720546,
-0.012175795493288));
#22699=CARTESIAN_POINT('Ctrl Pts',(-0.014043,-0.0329194552256883,-0.012175824389923));
#22700=CARTESIAN_POINT('Ctrl Pts',(-0.014043,-0.0329194567307744,-0.012175853286558));
#22701=CARTESIAN_POINT('Origin',(-0.0125,-0.0375520664398416,-0.0121758532865581));
#22702=CARTESIAN_POINT('',(-0.014043,-0.0334176320149228,-0.0121758533032418));
#22703=CARTESIAN_POINT('',(-0.014043,-0.0333016781458831,-0.0121758532817056));
#22704=CARTESIAN_POINT('',(-0.014043,-0.0375520664398416,-0.012175853286558));
#22705=CARTESIAN_POINT('Ctrl Pts',(-0.014043,-0.033301678145883,-0.0121758532768531));
#22706=CARTESIAN_POINT('Ctrl Pts',(-0.014042999999241,-0.033296152169727,
-0.0120551830319892));
#22707=CARTESIAN_POINT('Ctrl Pts',(-0.0140288457417181,-0.0332906903108907,
-0.0119349225769698));
#22708=CARTESIAN_POINT('Ctrl Pts',(-0.0139966325516127,-0.0332838656524112,
-0.0118000014907481));
#22709=CARTESIAN_POINT('Ctrl Pts',(-0.0139921423245643,-0.0332829702098229,
-0.0117825533799734));
#22710=CARTESIAN_POINT('Ctrl Pts',(-0.0139844089798668,-0.0332815101562521,
-0.0117545447263159));
#22711=CARTESIAN_POINT('Ctrl Pts',(-0.0139813561101524,-0.0332809516970285,
-0.011743933167611));
#22712=CARTESIAN_POINT('Ctrl Pts',(-0.0139757314063109,-0.0332799530605089,
-0.0117251435179896));
#22713=CARTESIAN_POINT('Ctrl Pts',(-0.0139732047965941,-0.0332795143826616,
-0.0117169523142201));
#22714=CARTESIAN_POINT('Ctrl Pts',(-0.0139677346345415,-0.0332785847981094,
-0.0116997290599259));
#22715=CARTESIAN_POINT('Ctrl Pts',(-0.0139647756697856,-0.0332780933963267,
-0.0116907023117127));
#22716=CARTESIAN_POINT('Ctrl Pts',(-0.0139566703640938,-0.0332767767238189,
-0.0116667261811201));
#22717=CARTESIAN_POINT('Ctrl Pts',(-0.0139513773794409,-0.0332759466169526,
-0.0116518278707558));
#22718=CARTESIAN_POINT('Ctrl Pts',(-0.0139221889122559,-0.0332715180028544,
-0.0115735070654471));
#22719=CARTESIAN_POINT('Ctrl Pts',(-0.013894365681829,-0.0332677884639099,
-0.0115116358488667));
#22720=CARTESIAN_POINT('Ctrl Pts',(-0.0138174143498841,-0.0332585334771182,
-0.011366824163526));
#22721=CARTESIAN_POINT('Ctrl Pts',(-0.0137644127396292,-0.0332529236212528,
-0.0112862647760647));
#22722=CARTESIAN_POINT('Ctrl Pts',(-0.0136740383076148,-0.0332447201061352,
-0.0111734466349453));
#22723=CARTESIAN_POINT('Ctrl Pts',(-0.0136420623434125,-0.0332420227577066,
-0.0111371620818609));
#22724=CARTESIAN_POINT('Ctrl Pts',(-0.0136015312225119,-0.0332388977514583,
-0.0110953087936099));
#22725=CARTESIAN_POINT('Ctrl Pts',(-0.0135945604091944,-0.0332383700911428,
-0.0110882481394156));
#22726=CARTESIAN_POINT('Ctrl Pts',(-0.0135835550348256,-0.0332375529407202,
-0.0110773139134795));
#22727=CARTESIAN_POINT('Ctrl Pts',(-0.0135795668106827,-0.0332372600152216,
-0.0110733943209213));
#22728=CARTESIAN_POINT('Ctrl Pts',(-0.0135724503514152,-0.03323674313081,
-0.0110664759746853));
#22729=CARTESIAN_POINT('Ctrl Pts',(-0.0135693307625849,-0.0332365185138221,
-0.0110634686871448));
#22730=CARTESIAN_POINT('Ctrl Pts',(-0.0135617929739524,-0.0332359804373121,
-0.011056263262125));
#22731=CARTESIAN_POINT('Ctrl Pts',(-0.0135573625317489,-0.0332356679746439,
-0.0110520781216601));
#22732=CARTESIAN_POINT('Ctrl Pts',(-0.0135436433875685,-0.0332347116196893,
-0.01103927153246));
#22733=CARTESIAN_POINT('Ctrl Pts',(-0.0135342729675937,-0.0332340740578503,
-0.0110307379857063));
#22734=CARTESIAN_POINT('Ctrl Pts',(-0.0134867184240696,-0.0332309098259927,
-0.0109884905393795));
#22735=CARTESIAN_POINT('Ctrl Pts',(-0.0134469836643739,-0.0332284925796322,
-0.0109565640261634));
#22736=CARTESIAN_POINT('Ctrl Pts',(-0.0133142590940587,-0.033220866288037,
-0.0108603308489456));
#22737=CARTESIAN_POINT('Ctrl Pts',(-0.0132157712838526,-0.0332158413491706,
-0.0108042521872334));
#22738=CARTESIAN_POINT('Ctrl Pts',(-0.0130694227664543,-0.0332082935853901,
-0.0107410145810245));
#22739=CARTESIAN_POINT('Ctrl Pts',(-0.0130259984901731,-0.033206048986665,
-0.0107245333712017));
#22740=CARTESIAN_POINT('Ctrl Pts',(-0.0129680087563431,-0.0332030117683303,
-0.0107054687749478));
#22741=CARTESIAN_POINT('Ctrl Pts',(-0.0129540541024748,-0.0332022780351559,
-0.0107010998626277));
#22742=CARTESIAN_POINT('Ctrl Pts',(-0.0129311800476335,-0.0332010698260814,
-0.0106942939019389));
#22743=CARTESIAN_POINT('Ctrl Pts',(-0.0129222969583428,-0.0332005992834258,
-0.0106917374832196));
#22744=CARTESIAN_POINT('Ctrl Pts',(-0.012905056972069,-0.0331996832850976,
-0.0106869433878798));
#22745=CARTESIAN_POINT('Ctrl Pts',(-0.0128967031576967,-0.0331992381715063,
-0.0106846958711251));
#22746=CARTESIAN_POINT('Ctrl Pts',(-0.0128770990768917,-0.0331981905139784,
-0.0106795979697089));
#22747=CARTESIAN_POINT('Ctrl Pts',(-0.0128658347779109,-0.0331975861617243,
-0.0106768040571065));
#22748=CARTESIAN_POINT('Ctrl Pts',(-0.012828587192449,-0.0331955795278258,
-0.0106680102706161));
#22749=CARTESIAN_POINT('Ctrl Pts',(-0.0128024808630634,-0.033194159870343,
-0.0106625571120584));
#22750=CARTESIAN_POINT('Ctrl Pts',(-0.0127393392062007,-0.0331906935492558,
-0.0106510670502018));
#22751=CARTESIAN_POINT('Ctrl Pts',(-0.0127022005491562,-0.0331886277416685,
-0.0106456993854977));
#22752=CARTESIAN_POINT('Ctrl Pts',(-0.0125228879134571,-0.0331785426351897,
-0.0106264253128829));
#22753=CARTESIAN_POINT('Ctrl Pts',(-0.0123794560510369,-0.0331700629168765,
-0.0106309536660835));
#22754=CARTESIAN_POINT('Ctrl Pts',(-0.0122193872987455,-0.0331611545540931,
-0.0106584576307248));
#22755=CARTESIAN_POINT('Ctrl Pts',(-0.0122001368681476,-0.0331600940283299,
-0.0106621441876746));
#22756=CARTESIAN_POINT('Ctrl Pts',(-0.0121736682899321,-0.0331586557360306,
-0.0106677378483833));
#22757=CARTESIAN_POINT('Ctrl Pts',(-0.0121663866318791,-0.0331582621475538,
-0.0106693319010822));
#22758=CARTESIAN_POINT('Ctrl Pts',(-0.0121547273851938,-0.0331576356276604,
-0.0106719729469641));
#22759=CARTESIAN_POINT('Ctrl Pts',(-0.0121503424172609,-0.0331574008367902,
-0.0106729864161349));
#22760=CARTESIAN_POINT('Ctrl Pts',(-0.0121410762691838,-0.0331569065573037,
-0.0106751707914174));
#22761=CARTESIAN_POINT('Ctrl Pts',(-0.0121361962496979,-0.0331566473516613,
-0.0106763463582545));
#22762=CARTESIAN_POINT('Ctrl Pts',(-0.0121239753659187,-0.0331560008153209,
-0.0106793534651212));
#22763=CARTESIAN_POINT('Ctrl Pts',(-0.0121166419780126,-0.0331556151921408,
-0.0106812152459307));
#22764=CARTESIAN_POINT('Ctrl Pts',(-0.012087969008273,-0.0331541155907492,
-0.0106887195791152));
#22765=CARTESIAN_POINT('Ctrl Pts',(-0.0120667369238895,-0.0331530228913737,
-0.0106947660502066));
#22766=CARTESIAN_POINT('Ctrl Pts',(-0.0120105755842982,-0.0331501626028183,
-0.0107120708379579));
#22767=CARTESIAN_POINT('Ctrl Pts',(-0.0119759049515203,-0.0331484280663903,
-0.0107241232949017));
#22768=CARTESIAN_POINT('Ctrl Pts',(-0.0118429268132295,-0.0331417856479386,
-0.0107757359221877));
#22769=CARTESIAN_POINT('Ctrl Pts',(-0.011748369474188,-0.0331370647311215,
-0.0108241409225991));
#22770=CARTESIAN_POINT('Ctrl Pts',(-0.0116147830261486,-0.0331295780527243,
-0.0109109085821144));
#22771=CARTESIAN_POINT('Ctrl Pts',(-0.0115715905166981,-0.0331270148741966,
-0.0109422612457511));
#22772=CARTESIAN_POINT('Ctrl Pts',(-0.0115182038036025,-0.0331236049908651,
-0.0109854081652544));
#22773=CARTESIAN_POINT('Ctrl Pts',(-0.0115064415724431,-0.0331228377457005,
-0.0109952072821043));
#22774=CARTESIAN_POINT('Ctrl Pts',(-0.0114877022356755,-0.0331215883127571,
-0.0110112973921178));
#22775=CARTESIAN_POINT('Ctrl Pts',(-0.0114806332307526,-0.0331211105987463,
-0.0110174800394696));
#22776=CARTESIAN_POINT('Ctrl Pts',(-0.0114671999910074,-0.0331201902407994,
-0.0110294471211287));
#22777=CARTESIAN_POINT('Ctrl Pts',(-0.011460826800954,-0.0331197480501957,
-0.0110352210000202));
#22778=CARTESIAN_POINT('Ctrl Pts',(-0.0114462227531703,-0.0331187217275783,
-0.0110486757271219));
#22779=CARTESIAN_POINT('Ctrl Pts',(-0.0114380270948717,-0.0331181360022596,
-0.011056393918768));
#22780=CARTESIAN_POINT('Ctrl Pts',(-0.0114121546808937,-0.0331162551347873,
-0.0110812988605483));
#22781=CARTESIAN_POINT('Ctrl Pts',(-0.0113948056805476,-0.0331149454778611,
-0.0110988192799597));
#22782=CARTESIAN_POINT('Ctrl Pts',(-0.0113113018554094,-0.0331083951899383,
-0.0111872909957439));
#22783=CARTESIAN_POINT('Ctrl Pts',(-0.0112515282733817,-0.0331028933737157,
-0.0112639473365652));
#22784=CARTESIAN_POINT('Ctrl Pts',(-0.0111485094637647,-0.0330918868883044,
-0.011425351829882));
#22785=CARTESIAN_POINT('Ctrl Pts',(-0.0111050893947673,-0.0330864133788897,
-0.0115095156814365));
#22786=CARTESIAN_POINT('Ctrl Pts',(-0.0110644683691668,-0.033080544567881,
-0.0116099132101176));
#22787=CARTESIAN_POINT('Ctrl Pts',(-0.0110594667646659,-0.0330798051885138,
-0.0116227680698562));
#22788=CARTESIAN_POINT('Ctrl Pts',(-0.0110524208953178,-0.0330787401342785,
-0.0116416212705606));
#22789=CARTESIAN_POINT('Ctrl Pts',(-0.0110502402635295,-0.0330784069972564,
-0.0116475675490016));
#22790=CARTESIAN_POINT('Ctrl Pts',(-0.0110464631061732,-0.0330778238832217,
-0.0116580668689895));
#22791=CARTESIAN_POINT('Ctrl Pts',(-0.0110448512311633,-0.0330775730171807,
-0.0116626142207783));
#22792=CARTESIAN_POINT('Ctrl Pts',(-0.0110414320188788,-0.033077036505556,
-0.0116724059589919));
#22793=CARTESIAN_POINT('Ctrl Pts',(-0.0110396316109885,-0.0330767512618778,
-0.0116776525866035));
#22794=CARTESIAN_POINT('Ctrl Pts',(-0.0110346690425709,-0.0330759569394036,
-0.0116923722431352));
#22795=CARTESIAN_POINT('Ctrl Pts',(-0.0110315704470788,-0.0330754514572935,
-0.0117018665860989));
#22796=CARTESIAN_POINT('Ctrl Pts',(-0.011011718255126,-0.0330721441819817,
-0.0117647590981194));
#22797=CARTESIAN_POINT('Ctrl Pts',(-0.0109977867187983,-0.0330694856854163,
-0.0118190096687034));
#22798=CARTESIAN_POINT('Ctrl Pts',(-0.0109644113418268,-0.0330615558892467,
-0.0119862633187186));
#22799=CARTESIAN_POINT('Ctrl Pts',(-0.0109545743677489,-0.0330564620125295,
-0.0121007706075571));
#22800=CARTESIAN_POINT('Ctrl Pts',(-0.0109586460915655,-0.0330489090233292,
-0.0122599315010698));
#22801=CARTESIAN_POINT('Ctrl Pts',(-0.010961722743937,-0.0330467476622815,
-0.0123044754470868));
#22802=CARTESIAN_POINT('Ctrl Pts',(-0.0109683424438608,-0.0330438081090372,
-0.0123631557808283));
#22803=CARTESIAN_POINT('Ctrl Pts',(-0.0109701604180367,-0.0330430839848228,
-0.0123774666025577));
#22804=CARTESIAN_POINT('Ctrl Pts',(-0.0109734662095251,-0.0330418875741503,
-0.0124008605179066));
#22805=CARTESIAN_POINT('Ctrl Pts',(-0.0109748351353497,-0.0330414190708893,
-0.0124099596692897));
#22806=CARTESIAN_POINT('Ctrl Pts',(-0.0109776516505458,-0.0330405041262296,
-0.0124276064444926));
#22807=CARTESIAN_POINT('Ctrl Pts',(-0.0109790900548561,-0.0330400579935811,
-0.0124361551964145));
#22808=CARTESIAN_POINT('Ctrl Pts',(-0.0109826421209544,-0.0330390033333457,
-0.0124562305144706));
#22809=CARTESIAN_POINT('Ctrl Pts',(-0.0109848151900985,-0.0330383929267915,
-0.0124677459117464));
#22810=CARTESIAN_POINT('Ctrl Pts',(-0.0109924957788973,-0.0330363440785638,
-0.0125060468579444));
#22811=CARTESIAN_POINT('Ctrl Pts',(-0.0109985839199138,-0.0330348872402636,
-0.0125327095558795));
#22812=CARTESIAN_POINT('Ctrl Pts',(-0.0110309772842716,-0.0330278377748488,
-0.0126590089468896));
#22813=CARTESIAN_POINT('Ctrl Pts',(-0.0110665086202501,-0.0330219547106032,
-0.012755994984683));
#22814=CARTESIAN_POINT('Ctrl Pts',(-0.0111480942304945,-0.0330111915779412,
-0.0129243641307971));
#22815=CARTESIAN_POINT('Ctrl Pts',(-0.0111908820708974,-0.0330063516450282,
-0.0129969074872464));
#22816=CARTESIAN_POINT('Ctrl Pts',(-0.0112476075637781,-0.0330010171067081,
-0.0130772778498566));
#22817=CARTESIAN_POINT('Ctrl Pts',(-0.0112560067434965,-0.0330002510111807,
-0.0130888340442841));
#22818=CARTESIAN_POINT('Ctrl Pts',(-0.0112683549198031,-0.0329991603767217,
-0.0131053366936856));
#22819=CARTESIAN_POINT('Ctrl Pts',(-0.0112721755274159,-0.0329988276816825,
-0.0131103778046844));
#22820=CARTESIAN_POINT('Ctrl Pts',(-0.0112789641621737,-0.0329982450633999,
-0.013119221586375));
#22821=CARTESIAN_POINT('Ctrl Pts',(-0.011281919180256,-0.0329979942562031,
-0.0131230340428408));
#22822=CARTESIAN_POINT('Ctrl Pts',(-0.0112883138634745,-0.032997457549047,
-0.0131312048081595));
#22823=CARTESIAN_POINT('Ctrl Pts',(-0.0112917592084221,-0.0329971720545742,
-0.013135558457285));
#22824=CARTESIAN_POINT('Ctrl Pts',(-0.0113014822670362,-0.0329963762978074,
-0.0131477094739646));
#22825=CARTESIAN_POINT('Ctrl Pts',(-0.0113078125736036,-0.032995869653209,
-0.0131554646153989));
#22826=CARTESIAN_POINT('Ctrl Pts',(-0.0113504464243476,-0.0329925286058322,
-0.0132066691322122));
#22827=CARTESIAN_POINT('Ctrl Pts',(-0.0113890457330661,-0.0329898408982329,
-0.0132481575847098));
#22828=CARTESIAN_POINT('Ctrl Pts',(-0.011514181234861,-0.03298176909845,
-0.013368630062464));
#22829=CARTESIAN_POINT('Ctrl Pts',(-0.0116074853011914,-0.0329765667088619,
-0.013439963034965));
#22830=CARTESIAN_POINT('Ctrl Pts',(-0.0117440273664582,-0.0329689961016864,
-0.013521632071756));
#22831=CARTESIAN_POINT('Ctrl Pts',(-0.0117809579514357,-0.0329669561624363,
-0.0135417205273295));
#22832=CARTESIAN_POINT('Ctrl Pts',(-0.0118313514045219,-0.0329641584066854,
-0.0135665215149725));
#22833=CARTESIAN_POINT('Ctrl Pts',(-0.0118441272053702,-0.0329634480126654,
-0.0135725923194883));
#22834=CARTESIAN_POINT('Ctrl Pts',(-0.0118652944906967,-0.0329622684372074,
-0.0135822961355113));
#22835=CARTESIAN_POINT('Ctrl Pts',(-0.0118736381516352,-0.0329618028283095,
-0.0135860317862855));
#22836=CARTESIAN_POINT('Ctrl Pts',(-0.0118899840936412,-0.032960889206223,
-0.0135931765542023));
#22837=CARTESIAN_POINT('Ctrl Pts',(-0.0118979829868851,-0.0329604414528551,
-0.0135965925880454));
#22838=CARTESIAN_POINT('Ctrl Pts',(-0.011916985876345,-0.0329593759791014,
-0.0136045187317482));
#22839=CARTESIAN_POINT('Ctrl Pts',(-0.011928013867272,-0.0329587562703609,
-0.0136089695679277));
#22840=CARTESIAN_POINT('Ctrl Pts',(-0.0119655619976626,-0.0329566411941367,
-0.0136236213513849));
#22841=CARTESIAN_POINT('Ctrl Pts',(-0.0119923109507173,-0.0329551257665596,
-0.0136332166705206));
#22842=CARTESIAN_POINT('Ctrl Pts',(-0.0120581938271205,-0.0329513713343882,
-0.0136548160656322));
#22843=CARTESIAN_POINT('Ctrl Pts',(-0.0120975685265146,-0.0329491086984023,
-0.013666011709668));
#22844=CARTESIAN_POINT('Ctrl Pts',(-0.0122030850394115,-0.0329430110253012,
-0.0136915266441084));
#22845=CARTESIAN_POINT('Ctrl Pts',(-0.0122698018796857,-0.0329391177373856,
-0.013703083518909));
#22846=CARTESIAN_POINT('Ctrl Pts',(-0.0123438199066056,-0.0329348369247644,
-0.0137109438446322));
#22847=CARTESIAN_POINT('Ctrl Pts',(-0.0123505867931309,-0.0329344459609326,
-0.0137116172453002));
#22848=CARTESIAN_POINT('Ctrl Pts',(-0.0124330278122191,-0.0329296889413775,
-0.0137192712514353));
#22849=CARTESIAN_POINT('Ctrl Pts',(-0.0125091205728446,-0.0329253553718529,
-0.0137206973512007));
#22850=CARTESIAN_POINT('Ctrl Pts',(-0.0125954496246285,-0.0329207106154944,
-0.0137159336742156));
#22851=CARTESIAN_POINT('Ctrl Pts',(-0.0126058792891594,-0.0329201540881409,
-0.0137152518116621));
#22852=CARTESIAN_POINT('Ctrl Pts',(-0.0126219952401571,-0.0329193021375521,
-0.0137140336288337));
#22853=CARTESIAN_POINT('Ctrl Pts',(-0.0126276866447654,-0.0329190028130942,
-0.01371357163749));
#22854=CARTESIAN_POINT('Ctrl Pts',(-0.0126381585326451,-0.0329184550843414,
-0.0137126630568392));
#22855=CARTESIAN_POINT('Ctrl Pts',(-0.0126429395401884,-0.0329182061904306,
-0.0137122257475079));
#22856=CARTESIAN_POINT('Ctrl Pts',(-0.0126538895050607,-0.0329176387833459,
-0.0137111726188893));
#22857=CARTESIAN_POINT('Ctrl Pts',(-0.0126600568555555,-0.0329173211019334,
-0.0137105419317078));
#22858=CARTESIAN_POINT('Ctrl Pts',(-0.0126793686295204,-0.0329163318439331,
-0.013708449385348));
#22859=CARTESIAN_POINT('Ctrl Pts',(-0.0126924984764923,-0.0329156672447565,
-0.0137068556594882));
#22860=CARTESIAN_POINT('Ctrl Pts',(-0.0127608272772352,-0.0329122429023933,
-0.0136976688387602));
#22861=CARTESIAN_POINT('Ctrl Pts',(-0.0128156100796063,-0.0329096135837406,
-0.0136872581774954));
#22862=CARTESIAN_POINT('Ctrl Pts',(-0.0129649152554317,-0.03290249052404,
-0.0136504102436105));
#22863=CARTESIAN_POINT('Ctrl Pts',(-0.0130576593490872,-0.0328981012696692,
-0.0136178938039853));
#22864=CARTESIAN_POINT('Ctrl Pts',(-0.0131958712734373,-0.0328909526596439,
-0.0135540935395386));
#22865=CARTESIAN_POINT('Ctrl Pts',(-0.0132438176649994,-0.0328883517338971,
-0.0135288194993583));
#22866=CARTESIAN_POINT('Ctrl Pts',(-0.0133035606075861,-0.0328848969701308,
-0.0134931901948779));
#22867=CARTESIAN_POINT('Ctrl Pts',(-0.0133166684933199,-0.0328841252425706,
-0.0134851044963859));
#22868=CARTESIAN_POINT('Ctrl Pts',(-0.0133375877116235,-0.0328828702892249,
-0.0134717639288243));
#22869=CARTESIAN_POINT('Ctrl Pts',(-0.0133454759792513,-0.0328823916115646,
-0.0134666313196696));
#22870=CARTESIAN_POINT('Ctrl Pts',(-0.0133604769657345,-0.0328814706014864,
-0.0134566742144954));
#22871=CARTESIAN_POINT('Ctrl Pts',(-0.0133675973107815,-0.0328810287367656,
-0.013451861813306));
#22872=CARTESIAN_POINT('Ctrl Pts',(-0.0133839168246122,-0.0328800049496955,
-0.013440632257663));
#22873=CARTESIAN_POINT('Ctrl Pts',(-0.0133930868912302,-0.0328794214596371,
-0.0134341738316986));
#22874=CARTESIAN_POINT('Ctrl Pts',(-0.0134219964039928,-0.0328775552894878,
-0.0134133378197421));
#22875=CARTESIAN_POINT('Ctrl Pts',(-0.0134414646539318,-0.0328762584115564,
-0.0133985918326946));
#22876=CARTESIAN_POINT('Ctrl Pts',(-0.0135243603918976,-0.0328705572458573,
-0.0133326497747992));
#22877=CARTESIAN_POINT('Ctrl Pts',(-0.0135840185090255,-0.0328659761684123,
-0.0132769406511241));
#22878=CARTESIAN_POINT('Ctrl Pts',(-0.013703765963006,-0.0328558137271099,
-0.0131459127545683));
#22879=CARTESIAN_POINT('Ctrl Pts',(-0.0137617835849164,-0.0328502190270702,
-0.013069145510338));
#22880=CARTESIAN_POINT('Ctrl Pts',(-0.0138250427961349,-0.0328435712401595,
-0.0129668642335203));
#22881=CARTESIAN_POINT('Ctrl Pts',(-0.0138373078725187,-0.0328422512351829,
-0.0129459471180647));
#22882=CARTESIAN_POINT('Ctrl Pts',(-0.0138530011160535,-0.0328405280150102,
-0.0129176769838345));
#22883=CARTESIAN_POINT('Ctrl Pts',(-0.0138568711142915,-0.0328401000875645,
-0.0129105744599875));
#22884=CARTESIAN_POINT('Ctrl Pts',(-0.0138631050811206,-0.0328394062463213,
-0.0128989161292336));
#22885=CARTESIAN_POINT('Ctrl Pts',(-0.0138655024378823,-0.0328391382916245,
-0.0128943784637747));
#22886=CARTESIAN_POINT('Ctrl Pts',(-0.0138701924285461,-0.0328386119678611,
-0.0128853930988605));
#22887=CARTESIAN_POINT('Ctrl Pts',(-0.0138724861399803,-0.0328383535381095,
-0.0128809460697477));
#22888=CARTESIAN_POINT('Ctrl Pts',(-0.0138781587854846,-0.0328377116394678,
-0.0128698154239936));
#22889=CARTESIAN_POINT('Ctrl Pts',(-0.0138815108142272,-0.0328373298260715,
-0.0128631181268945));
#22890=CARTESIAN_POINT('Ctrl Pts',(-0.0138942850700447,-0.0328358639294411,
-0.012837124234716));
#22891=CARTESIAN_POINT('Ctrl Pts',(-0.0139033532252393,-0.0328347999244533,
-0.0128176553858556));
#22892=CARTESIAN_POINT('Ctrl Pts',(-0.013926224460689,-0.0328320357980582,
-0.0127657474880569));
#22893=CARTESIAN_POINT('Ctrl Pts',(-0.0139393278280347,-0.0328303660408524,
-0.0127330130776393));
#22894=CARTESIAN_POINT('Ctrl Pts',(-0.0139917105688196,-0.0328231694238316,
-0.0125879320291054));
#22895=CARTESIAN_POINT('Ctrl Pts',(-0.0140190391198761,-0.0328178951815481,
-0.012471709497576));
#22896=CARTESIAN_POINT('Ctrl Pts',(-0.0140373546116113,-0.0328103457982441,
-0.0123136809524147));
#22897=CARTESIAN_POINT('Ctrl Pts',(-0.0140404158572249,-0.0328084080817642,
-0.0122737018312358));
#22898=CARTESIAN_POINT('Ctrl Pts',(-0.0140423272384866,-0.0328058804702862,
-0.0122227100333379));
#22899=CARTESIAN_POINT('Ctrl Pts',(-0.0140426208761371,-0.0328053347200742,
-0.0122117655427823));
#22900=CARTESIAN_POINT('Ctrl Pts',(-0.0140429326708424,-0.0328043677931774,
-0.0121924976864138));
#22901=CARTESIAN_POINT('Ctrl Pts',(-0.014043,-0.0328039481464066,-0.0121841755036127));
#22902=CARTESIAN_POINT('Ctrl Pts',(-0.014043,-0.0328035263970765,-0.012175853286558));
#22903=CARTESIAN_POINT('Ctrl Pts',(-0.014043,-0.0329194567307744,-0.012175853286558));
#22904=CARTESIAN_POINT('Ctrl Pts',(-0.014043,-0.0329195999341371,-0.0121786026942404));
#22905=CARTESIAN_POINT('Ctrl Pts',(-0.0140429926515305,-0.0329197427213959,
-0.0121813520976706));
#22906=CARTESIAN_POINT('Ctrl Pts',(-0.0140429619707811,-0.0329200399154781,
-0.0121870914667029));
#22907=CARTESIAN_POINT('Ctrl Pts',(-0.0140429372967764,-0.0329201942468374,
-0.0121900813744717));
#22908=CARTESIAN_POINT('Ctrl Pts',(-0.0140428360710219,-0.0329206610219979,
-0.0121991522450127));
#22909=CARTESIAN_POINT('Ctrl Pts',(-0.0140427322590762,-0.0329209719621453,
-0.0122052329173575));
#22910=CARTESIAN_POINT('Ctrl Pts',(-0.0140422594856282,-0.0329220174968526,
-0.0122257998779618));
#22911=CARTESIAN_POINT('Ctrl Pts',(-0.014041722401065,-0.032922743339528,
-0.0122402819253537));
#22912=CARTESIAN_POINT('Ctrl Pts',(-0.0140367797607974,-0.0329275248478707,
-0.0123368139459897));
#22913=CARTESIAN_POINT('Ctrl Pts',(-0.0140260297645205,-0.0329312979608478,
-0.012418414989397));
#22914=CARTESIAN_POINT('Ctrl Pts',(-0.0139871455167143,-0.0329397967123801,
-0.0126000974179127));
#22915=CARTESIAN_POINT('Ctrl Pts',(-0.0139553108782099,-0.0329445061163852,
-0.0126989722561689));
#22916=CARTESIAN_POINT('Ctrl Pts',(-0.0139026943126495,-0.0329508845023387,
-0.0128193344209594));
#22917=CARTESIAN_POINT('Ctrl Pts',(-0.0138908936270081,-0.0329522524208113,
-0.0128444593776491));
#22918=CARTESIAN_POINT('Ctrl Pts',(-0.0138731125759079,-0.0329542358861596,
-0.0128798067357444));
#22919=CARTESIAN_POINT('Ctrl Pts',(-0.013867681949484,-0.0329548323029073,
-0.0128903004013197));
#22920=CARTESIAN_POINT('Ctrl Pts',(-0.0138580377772868,-0.0329558760007039,
-0.0129084229609032));
#22921=CARTESIAN_POINT('Ctrl Pts',(-0.0138538790841758,-0.0329563213172082,
-0.0129160805176271));
#22922=CARTESIAN_POINT('Ctrl Pts',(-0.0138451844818609,-0.0329572429074834,
-0.0129317718132345));
#22923=CARTESIAN_POINT('Ctrl Pts',(-0.0138406409435228,-0.0329577194444046,
-0.0129398009057024));
#22924=CARTESIAN_POINT('Ctrl Pts',(-0.0138288143456409,-0.0329589472875306,
-0.0129602697685481));
#22925=CARTESIAN_POINT('Ctrl Pts',(-0.0138214285801439,-0.0329597023082833,
-0.0129726489133671));
#22926=CARTESIAN_POINT('Ctrl Pts',(-0.013790692239611,-0.032962798411707,
-0.0130225625361672));
#22927=CARTESIAN_POINT('Ctrl Pts',(-0.0137659088770554,-0.032965191816156,
-0.0130591862922433));
#22928=CARTESIAN_POINT('Ctrl Pts',(-0.0136711795036043,-0.0329739867068987,
-0.0131869838270116));
#22929=CARTESIAN_POINT('Ctrl Pts',(-0.0135926801614238,-0.0329806827048526,
-0.0132713401750666));
#22930=CARTESIAN_POINT('Ctrl Pts',(-0.0134630178788468,-0.0329904300486842,
-0.0133827467251288));
#22931=CARTESIAN_POINT('Ctrl Pts',(-0.0134185081556305,-0.0329935791001491,
-0.0134169572659047));
#22932=CARTESIAN_POINT('Ctrl Pts',(-0.013363965201739,-0.0329971253974243,
-0.0134543342323532));
#22933=CARTESIAN_POINT('Ctrl Pts',(-0.0133556446117909,-0.0329976582109083,
-0.0134599178126856));
#22934=CARTESIAN_POINT('Ctrl Pts',(-0.013342616163237,-0.0329984790999736,
-0.0134684777521611));
#22935=CARTESIAN_POINT('Ctrl Pts',(-0.0133379457253415,-0.0329987707303358,
-0.013471510251547));
#22936=CARTESIAN_POINT('Ctrl Pts',(-0.0133291798075773,-0.0329993130076031,
-0.0134771347072217));
#22937=CARTESIAN_POINT('Ctrl Pts',(-0.0133250885276702,-0.0329995640327805,
-0.013479732656352));
#22938=CARTESIAN_POINT('Ctrl Pts',(-0.0133155927122235,-0.0330001419785699,
-0.0134856998750939));
#22939=CARTESIAN_POINT('Ctrl Pts',(-0.0133101794889474,-0.0330004679770742,
-0.0134890550060902));
#22940=CARTESIAN_POINT('Ctrl Pts',(-0.0132924250257821,-0.0330015264303756,
-0.0134999077007458));
#22941=CARTESIAN_POINT('Ctrl Pts',(-0.0132799989623827,-0.0330022503496351,
-0.0135072657546555));
#22942=CARTESIAN_POINT('Ctrl Pts',(-0.0132005855368806,-0.0330067824600841,
-0.0135527966970516));
#22943=CARTESIAN_POINT('Ctrl Pts',(-0.0131309130594329,-0.0330103411939344,
-0.0135860817231761));
#22944=CARTESIAN_POINT('Ctrl Pts',(-0.012994618020904,-0.0330170381419621,
-0.0136390617723327));
#22945=CARTESIAN_POINT('Ctrl Pts',(-0.012928588319169,-0.0330201747633333,
-0.0136597460937967));
#22946=CARTESIAN_POINT('Ctrl Pts',(-0.0128226904031785,-0.0330252666629476,
-0.0136852588003124));
#22947=CARTESIAN_POINT('Ctrl Pts',(-0.0127836398937354,-0.0330271561274909,
-0.0136930817626132));
#22948=CARTESIAN_POINT('Ctrl Pts',(-0.0127168092452417,-0.0330304420367926,
-0.0137037995368402));
#22949=CARTESIAN_POINT('Ctrl Pts',(-0.0126891729729697,-0.0330318156964838,
-0.0137074666382348));
#22950=CARTESIAN_POINT('Ctrl Pts',(-0.0126496834413369,-0.0330338060527694,
-0.0137116214774584));
#22951=CARTESIAN_POINT('Ctrl Pts',(-0.0126378997052687,-0.0330344034310928,
-0.0137127243709459));
#22952=CARTESIAN_POINT('Ctrl Pts',(-0.0126174166645416,-0.0330354482528905,
-0.0137144040057708));
#22953=CARTESIAN_POINT('Ctrl Pts',(-0.012608722916222,-0.033035893719385,
-0.0137150427849832));
#22954=CARTESIAN_POINT('Ctrl Pts',(-0.0125908251323664,-0.0330368150930682,
-0.013716205446885));
#22955=CARTESIAN_POINT('Ctrl Pts',(-0.01258162089507,-0.0330372912578075,
-0.0137167205770884));
#22956=CARTESIAN_POINT('Ctrl Pts',(-0.0125580461718774,-0.0330385170193999,
-0.013717828155152));
#22957=CARTESIAN_POINT('Ctrl Pts',(-0.0125436712294385,-0.0330392703064992,
-0.013718302202476));
#22958=CARTESIAN_POINT('Ctrl Pts',(-0.0124853957293894,-0.033042348631409,
-0.0137194086951833));
#22959=CARTESIAN_POINT('Ctrl Pts',(-0.0124414871536661,-0.0330447252279825,
-0.0137183682182671));
#22960=CARTESIAN_POINT('Ctrl Pts',(-0.0122827748385063,-0.0330535163660108,
-0.0137078209683911));
#22961=CARTESIAN_POINT('Ctrl Pts',(-0.0121690868453822,-0.033060228775654,
-0.0136873436842773));
#22962=CARTESIAN_POINT('Ctrl Pts',(-0.0120049295896913,-0.0330699971878748,
-0.0136383543126339));
#22963=CARTESIAN_POINT('Ctrl Pts',(-0.0119520183292706,-0.0330731508227526,
-0.0136193633028095));
#22964=CARTESIAN_POINT('Ctrl Pts',(-0.0118910220392996,-0.0330767014860323,
-0.0135936315833082));
#22965=CARTESIAN_POINT('Ctrl Pts',(-0.0118818253204101,-0.0330772344536998,
-0.0135896458920154));
#22966=CARTESIAN_POINT('Ctrl Pts',(-0.011867579849828,-0.0330780555274094,
-0.0135833065781637));
#22967=CARTESIAN_POINT('Ctrl Pts',(-0.0118625040576128,-0.0330783471907059,
-0.0135810148216686));
#22968=CARTESIAN_POINT('Ctrl Pts',(-0.0118530345009027,-0.0330788894950169,
-0.0135766773764606));
#22969=CARTESIAN_POINT('Ctrl Pts',(-0.0118486379596951,-0.0330791405147342,
-0.0135746384668961));
#22970=CARTESIAN_POINT('Ctrl Pts',(-0.01183848705678,-0.0330797184050798,
-0.0135698727164946));
#22971=CARTESIAN_POINT('Ctrl Pts',(-0.0118327398934341,-0.0330800443542148,
-0.0135671309360713));
#22972=CARTESIAN_POINT('Ctrl Pts',(-0.0118140207415016,-0.0330811024748431,
-0.0135580579771797));
#22973=CARTESIAN_POINT('Ctrl Pts',(-0.011801120249478,-0.0330818261182355,
-0.0135515801753165));
#22974=CARTESIAN_POINT('Ctrl Pts',(-0.0117198965951304,-0.0330863584258906,
-0.0135093573960194));
#22975=CARTESIAN_POINT('Ctrl Pts',(-0.0116542362045179,-0.0330899175452863,
-0.013468710748643));
#22976=CARTESIAN_POINT('Ctrl Pts',(-0.0115360069820772,-0.0330966148742783,
-0.0133826438735455));
#22977=CARTESIAN_POINT('Ctrl Pts',(-0.0114829253133027,-0.0330997514956493,
-0.0133382580750814));
#22978=CARTESIAN_POINT('Ctrl Pts',(-0.0114042395231014,-0.0331048433952636,
-0.0132629333565266));
#22979=CARTESIAN_POINT('Ctrl Pts',(-0.0113765573810259,-0.033106732859807,
-0.0132343005076058));
#22980=CARTESIAN_POINT('Ctrl Pts',(-0.0113314294628993,-0.033110018769109,
-0.0131838557133378));
#22981=CARTESIAN_POINT('Ctrl Pts',(-0.0113134115642216,-0.0331113924288003,
-0.0131625821028058));
#22982=CARTESIAN_POINT('Ctrl Pts',(-0.0112885788147417,-0.033113382785086,
-0.0131315979076253));
#22983=CARTESIAN_POINT('Ctrl Pts',(-0.011281283895528,-0.0331139801634094,
-0.0131222781992908));
#22984=CARTESIAN_POINT('Ctrl Pts',(-0.0112688033457407,-0.0331150249852071,
-0.0131059499413432));
#22985=CARTESIAN_POINT('Ctrl Pts',(-0.0112635685145531,-0.0331154704517016,
-0.0130989795868927));
#22986=CARTESIAN_POINT('Ctrl Pts',(-0.0112529198203433,-0.0331163918253848,
-0.0130845474089121));
#22987=CARTESIAN_POINT('Ctrl Pts',(-0.011247513213227,-0.0331168679901241,
-0.0130770806865507));
#22988=CARTESIAN_POINT('Ctrl Pts',(-0.0112338435624034,-0.0331180937517165,
-0.0130578417949739));
#22989=CARTESIAN_POINT('Ctrl Pts',(-0.0112256777408025,-0.0331188470388158,
-0.0130460019027213));
#22990=CARTESIAN_POINT('Ctrl Pts',(-0.0111932598222739,-0.0331219253637252,
-0.0129975629020136));
#22991=CARTESIAN_POINT('Ctrl Pts',(-0.0111704111002564,-0.0331243019602983,
-0.0129600531497367));
#22992=CARTESIAN_POINT('Ctrl Pts',(-0.0110935323815902,-0.0331330930983265,
-0.0128208033523248));
#22993=CARTESIAN_POINT('Ctrl Pts',(-0.0110493365457318,-0.03313980550797,
-0.0127140746915099));
#22994=CARTESIAN_POINT('Ctrl Pts',(-0.0110018636076939,-0.0331495739201912,
-0.0125494724944212));
#22995=CARTESIAN_POINT('Ctrl Pts',(-0.010989255406508,-0.0331527275550691,
-0.0124946884347279));
#22996=CARTESIAN_POINT('Ctrl Pts',(-0.0109779508597921,-0.0331562782183488,
-0.0124294590241645));
#22997=CARTESIAN_POINT('Ctrl Pts',(-0.0109763356030537,-0.0331568111860163,
-0.0124195667888718));
#22998=CARTESIAN_POINT('Ctrl Pts',(-0.0109739729479484,-0.033157632259726,
-0.012404154514767));
#22999=CARTESIAN_POINT('Ctrl Pts',(-0.0109731588811264,-0.0331579239230225,
-0.0123986451491363));
#23000=CARTESIAN_POINT('Ctrl Pts',(-0.0109716921962995,-0.0331584662273335,
-0.0123883332739022));
#23001=CARTESIAN_POINT('Ctrl Pts',(-0.0109710323735861,-0.0331587172470508,
-0.0123835320906325));
#23002=CARTESIAN_POINT('Ctrl Pts',(-0.010969557954751,-0.0331592951373964,
-0.0123724154681247));
#23003=CARTESIAN_POINT('Ctrl Pts',(-0.0109687598191304,-0.0331596210865314,
-0.012366098014053));
#23004=CARTESIAN_POINT('Ctrl Pts',(-0.0109662802579694,-0.0331606792071597,
-0.0123454442732641));
#23005=CARTESIAN_POINT('Ctrl Pts',(-0.0109647608413423,-0.0331614028505521,
-0.0123310889263665));
#23006=CARTESIAN_POINT('Ctrl Pts',(-0.0109564039104447,-0.0331659351582133,
-0.0122399285904424));
#23007=CARTESIAN_POINT('Ctrl Pts',(-0.0109551297071341,-0.0331694942776144,
-0.0121627158112966));
#23008=CARTESIAN_POINT('Ctrl Pts',(-0.010963671607677,-0.0331761916066194,
-0.0120167271403392));
#23009=CARTESIAN_POINT('Ctrl Pts',(-0.0109723401835273,-0.0331793282279981,
-0.0119480786262911));
#23010=CARTESIAN_POINT('Ctrl Pts',(-0.0109932086416718,-0.0331844201276134,
-0.0118411685039492));
#23011=CARTESIAN_POINT('Ctrl Pts',(-0.0110023452679362,-0.0331863095921493,
-0.0118024043055921));
#23012=CARTESIAN_POINT('Ctrl Pts',(-0.0110204097744286,-0.0331895955014393,
-0.0117371748656594));
#23013=CARTESIAN_POINT('Ctrl Pts',(-0.011028575540593,-0.0331909691611265,
-0.0117105190701174));
#23014=CARTESIAN_POINT('Ctrl Pts',(-0.0110412303003652,-0.0331929595174073,
-0.0116728820823938));
#23015=CARTESIAN_POINT('Ctrl Pts',(-0.0110451309990397,-0.03319355689573,
-0.0116617081234135));
#23016=CARTESIAN_POINT('Ctrl Pts',(-0.0110521273049904,-0.0331946017175269,
-0.0116423838424964));
#23017=CARTESIAN_POINT('Ctrl Pts',(-0.0110551641887478,-0.0331950471840213,
-0.0116342127571505));
#23018=CARTESIAN_POINT('Ctrl Pts',(-0.0110615547780563,-0.0331959685577046,
-0.0116174543915371));
#23019=CARTESIAN_POINT('Ctrl Pts',(-0.0110649165262468,-0.0331964447224443,
-0.0116088705699796));
#23020=CARTESIAN_POINT('Ctrl Pts',(-0.0110737195480242,-0.0331976704840381,
-0.0115869730561571));
#23021=CARTESIAN_POINT('Ctrl Pts',(-0.0110792703383311,-0.0331984237711386,
-0.0115737045815427));
#23022=CARTESIAN_POINT('Ctrl Pts',(-0.011102514379402,-0.0332015020960607,
-0.0115202539237943));
#23023=CARTESIAN_POINT('Ctrl Pts',(-0.0111217321636346,-0.0332038786926459,
-0.0114807606028172));
#23024=CARTESIAN_POINT('Ctrl Pts',(-0.01119736777905,-0.0332126698306768,
-0.0113408317024874));
#23025=CARTESIAN_POINT('Ctrl Pts',(-0.0112632968571075,-0.0332193822403086,
-0.0112459758351642));
#23026=CARTESIAN_POINT('Ctrl Pts',(-0.0113761538947043,-0.0332291506525148,
-0.011117092740428));
#23027=CARTESIAN_POINT('Ctrl Pts',(-0.0114154404776327,-0.0332323042873894,
-0.0110768829862725));
#23028=CARTESIAN_POINT('Ctrl Pts',(-0.0114642208455187,-0.0332358549506661,
-0.011032126484172));
#23029=CARTESIAN_POINT('Ctrl Pts',(-0.011471672085274,-0.0332363879183335,
-0.0110254224257381));
#23030=CARTESIAN_POINT('Ctrl Pts',(-0.0114833644229151,-0.033237208992043,
-0.0110151069241687));
#23031=CARTESIAN_POINT('Ctrl Pts',(-0.0114875605180411,-0.0332375006553395,
-0.0110114451486249));
#23032=CARTESIAN_POINT('Ctrl Pts',(-0.0114954451454344,-0.0332380429596505,
-0.0110046393726883));
#23033=CARTESIAN_POINT('Ctrl Pts',(-0.0114991286688594,-0.0332382939793677,
-0.0110014900264106));
#23034=CARTESIAN_POINT('Ctrl Pts',(-0.0115076862849315,-0.0332388718697134,
-0.0109942429294712));
#23035=CARTESIAN_POINT('Ctrl Pts',(-0.0115125709667679,-0.0332391978188484,
-0.0109901579411259));
#23036=CARTESIAN_POINT('Ctrl Pts',(-0.0115286106547145,-0.0332402559394769,
-0.0109769120495777));
#23037=CARTESIAN_POINT('Ctrl Pts',(-0.0115398692343731,-0.0332409795828695,
-0.0109678771729534));
#23038=CARTESIAN_POINT('Ctrl Pts',(-0.0116120622211135,-0.0332455118905934,
-0.0109115902469658));
#23039=CARTESIAN_POINT('Ctrl Pts',(-0.0116763456830407,-0.0332490710100485,
-0.0108687992014549));
#23040=CARTESIAN_POINT('Ctrl Pts',(-0.0118038054591141,-0.033255768339187,
-0.0107971077621977));
#23041=CARTESIAN_POINT('Ctrl Pts',(-0.0118662545682228,-0.0332589049606438,
-0.010767310586225));
#23042=CARTESIAN_POINT('Ctrl Pts',(-0.0119674912369483,-0.0332639968602696,
-0.0107271060627891));
#23043=CARTESIAN_POINT('Ctrl Pts',(-0.0120050466006367,-0.0332658863247279,
-0.0107138495347917));
#23044=CARTESIAN_POINT('Ctrl Pts',(-0.0120696953875809,-0.0332691722338961,
-0.0106938060764293));
#23045=CARTESIAN_POINT('Ctrl Pts',(-0.0120965373776007,-0.0332705458935413,
-0.0106862748948614));
#23046=CARTESIAN_POINT('Ctrl Pts',(-0.0121350451156411,-0.0332725362497718,
-0.0106765877993376));
#23047=CARTESIAN_POINT('Ctrl Pts',(-0.0121465552086665,-0.0332731336280875,
-0.0106738327014075));
#23048=CARTESIAN_POINT('Ctrl Pts',(-0.0121665961081347,-0.0332741784498762,
-0.010669278750204));
#23049=CARTESIAN_POINT('Ctrl Pts',(-0.0121751126573689,-0.0332746239163695,
-0.0106674192644108));
#23050=CARTESIAN_POINT('Ctrl Pts',(-0.0121926671517927,-0.0332755452900544,
-0.0106637420132362));
#23051=CARTESIAN_POINT('Ctrl Pts',(-0.0122017065321154,-0.0332760214547967,
-0.0106619328842395));
#23052=CARTESIAN_POINT('Ctrl Pts',(-0.0122248889067874,-0.0332772472164056,
-0.0106575088790393));
#23053=CARTESIAN_POINT('Ctrl Pts',(-0.0122390530250158,-0.0332780005035187,
-0.0106550105889884));
#23054=CARTESIAN_POINT('Ctrl Pts',(-0.0122965889274273,-0.0332810788285701,
-0.0106456897266794));
#23055=CARTESIAN_POINT('Ctrl Pts',(-0.0123402047784401,-0.0332834554252774,
-0.0106405221968228));
#23056=CARTESIAN_POINT('Ctrl Pts',(-0.0124988168744899,-0.0332922465633352,
-0.0106285619925034));
#23057=CARTESIAN_POINT('Ctrl Pts',(-0.0126142570046326,-0.0332989589728471,
-0.0106327874828199));
#23058=CARTESIAN_POINT('Ctrl Pts',(-0.0127836855395962,-0.0333087273849002,
-0.0106581159980292));
#23059=CARTESIAN_POINT('Ctrl Pts',(-0.0128387476170901,-0.033311881019742,
-0.010669448583193));
#23060=CARTESIAN_POINT('Ctrl Pts',(-0.0129027652163431,-0.0333154316829873,
-0.0106863132112805));
#23061=CARTESIAN_POINT('Ctrl Pts',(-0.0129124324335934,-0.0333159646506537,
-0.0106889609052973));
#23062=CARTESIAN_POINT('Ctrl Pts',(-0.0129274300654441,-0.0333167857243618,
-0.0106932260395573));
#23063=CARTESIAN_POINT('Ctrl Pts',(-0.0129327785176059,-0.0333170773876581,
-0.0106947784164003));
#23064=CARTESIAN_POINT('Ctrl Pts',(-0.0129427654904171,-0.0333176196919689,
-0.0106977358323721));
#23065=CARTESIAN_POINT('Ctrl Pts',(-0.012947405803118,-0.0333178707116862,
-0.0106991337682948));
#23066=CARTESIAN_POINT('Ctrl Pts',(-0.0129581277551387,-0.0333184486020322,
-0.0107024190311331));
#23067=CARTESIAN_POINT('Ctrl Pts',(-0.0129642043768496,-0.0333187745511676,
-0.0107043221640999));
#23068=CARTESIAN_POINT('Ctrl Pts',(-0.0129840167495783,-0.0333198326717984,
-0.0107106621263353));
#23069=CARTESIAN_POINT('Ctrl Pts',(-0.0129977024153552,-0.033320556315193,
-0.0107152542026567));
#23070=CARTESIAN_POINT('Ctrl Pts',(-0.0130840725614564,-0.033325088623549,
-0.0107455897523201));
#23071=CARTESIAN_POINT('Ctrl Pts',(-0.0131548127864189,-0.0333286477435496,
-0.0107765616686534));
#23072=CARTESIAN_POINT('Ctrl Pts',(-0.0132840065245436,-0.0333353450740348,
-0.0108450791390976));
#23073=CARTESIAN_POINT('Ctrl Pts',(-0.0133428217329245,-0.0333384816962801,
-0.0108815282347096));
#23074=CARTESIAN_POINT('Ctrl Pts',(-0.013431351664073,-0.0333435735960127,
-0.0109449925399469));
#23075=CARTESIAN_POINT('Ctrl Pts',(-0.0134627981096062,-0.0333454630596884,
-0.0109694314546625));
#23076=CARTESIAN_POINT('Ctrl Pts',(-0.0135145943704972,-0.0333487489676268,
-0.0110130015095112));
#23077=CARTESIAN_POINT('Ctrl Pts',(-0.0135354345954656,-0.0333501226268487,
-0.011031518951365));
#23078=CARTESIAN_POINT('Ctrl Pts',(-0.0135643920696066,-0.0333521129825711,
-0.0110586878597246));
#23079=CARTESIAN_POINT('Ctrl Pts',(-0.0135729294094318,-0.0333527103608161,
-0.0110668846030151));
#23080=CARTESIAN_POINT('Ctrl Pts',(-0.0135875897039654,-0.0333537551825219,
-0.0110812877907902));
#23081=CARTESIAN_POINT('Ctrl Pts',(-0.0135937559755411,-0.0333542006490042,
-0.0110874494779754));
#23082=CARTESIAN_POINT('Ctrl Pts',(-0.0136063351284224,-0.0333551220227048,
-0.0111002341317816));
#23083=CARTESIAN_POINT('Ctrl Pts',(-0.0136127415179121,-0.0333555981874744,
-0.0111068629723535));
#23084=CARTESIAN_POINT('Ctrl Pts',(-0.0136289898413118,-0.0333568239492358,
-0.0111239798190084));
#23085=CARTESIAN_POINT('Ctrl Pts',(-0.0136387450853462,-0.0333575772364759,
-0.0111345485928338));
#23086=CARTESIAN_POINT('Ctrl Pts',(-0.0136776755201077,-0.0333606555628316,
-0.0111779269587674));
#23087=CARTESIAN_POINT('Ctrl Pts',(-0.0137055899193784,-0.0333630321607721,
-0.0112118361621427));
#23088=CARTESIAN_POINT('Ctrl Pts',(-0.0138013537393381,-0.0333718232991008,
-0.0113388406291071));
#23089=CARTESIAN_POINT('Ctrl Pts',(-0.0138601715899953,-0.0333785357074034,
-0.0114382626285861));
#23090=CARTESIAN_POINT('Ctrl Pts',(-0.0139304024462809,-0.0333883041179107,
-0.011594516204129));
#23091=CARTESIAN_POINT('Ctrl Pts',(-0.0139506170570479,-0.0333914577524209,
-0.0116469721736676));
#23092=CARTESIAN_POINT('Ctrl Pts',(-0.0139710154015459,-0.0333950084153505,
-0.0117099529283649));
#23093=CARTESIAN_POINT('Ctrl Pts',(-0.0139740107524153,-0.0333955413830057,
-0.0117195181383488));
#23094=CARTESIAN_POINT('Ctrl Pts',(-0.0139785251593245,-0.0333963624567005,
-0.0117344426300953));
#23095=CARTESIAN_POINT('Ctrl Pts',(-0.0139801087098747,-0.0333966541199944,
-0.0117397819354392));
#23096=CARTESIAN_POINT('Ctrl Pts',(-0.0139830162074801,-0.0333971964243033,
-0.0117497835549122));
#23097=CARTESIAN_POINT('Ctrl Pts',(-0.013984347099905,-0.0333974474440209,
-0.0117544435390592));
#23098=CARTESIAN_POINT('Ctrl Pts',(-0.0139873758422689,-0.033398025334371,
-0.0117652407576162));
#23099=CARTESIAN_POINT('Ctrl Pts',(-0.0139890576808882,-0.03339835128351,
-0.0117713823100489));
#23100=CARTESIAN_POINT('Ctrl Pts',(-0.0139944276440985,-0.0333994094041648,
-0.0117914792936379));
#23101=CARTESIAN_POINT('Ctrl Pts',(-0.0139979580720056,-0.0334001330475793,
-0.0118054764613262));
#23102=CARTESIAN_POINT('Ctrl Pts',(-0.0140190984339713,-0.0334046653624545,
-0.0118945447325097));
#23103=CARTESIAN_POINT('Ctrl Pts',(-0.0140312582910716,-0.0334082244880811,
-0.0119708047959815));
#23104=CARTESIAN_POINT('Ctrl Pts',(-0.0140412213047356,-0.033413716519899,
-0.012090310517274));
#23105=CARTESIAN_POINT('Ctrl Pts',(-0.0140430000004635,-0.0334156645237435,
-0.0121330785747856));
#23106=CARTESIAN_POINT('Ctrl Pts',(-0.014043,-0.033417632014157,-0.012175853303277));
#23107=CARTESIAN_POINT('Origin',(-0.0125,-0.0375520664398416,-0.0121758532865581));
#23108=CARTESIAN_POINT('',(-0.014043,-0.0339165738369763,-0.0121758532867271));
#23109=CARTESIAN_POINT('',(-0.014043,-0.0338009094848242,-0.0121758532862401));
#23110=CARTESIAN_POINT('',(-0.014043,-0.0375520664398416,-0.012175853286558));
#23111=CARTESIAN_POINT('Ctrl Pts',(-0.014043,-0.0338009094848242,-0.0121758532859222));
#23112=CARTESIAN_POINT('Ctrl Pts',(-0.0140429999999882,-0.0337993161421864,
-0.0121472447835339));
#23113=CARTESIAN_POINT('Ctrl Pts',(-0.0140422043596351,-0.0337977478260463,
-0.0121186389603028));
#23114=CARTESIAN_POINT('Ctrl Pts',(-0.0140401034932399,-0.0337957263984264,
-0.012080909112732));
#23115=CARTESIAN_POINT('Ctrl Pts',(-0.0140395117507698,-0.0337952395588485,
-0.0120717536068128));
#23116=CARTESIAN_POINT('Ctrl Pts',(-0.0140384442002407,-0.0337944746419083,
-0.0120572477009742));
#23117=CARTESIAN_POINT('Ctrl Pts',(-0.014038022063108,-0.0337941937084367,
-0.012051893707222));
#23118=CARTESIAN_POINT('Ctrl Pts',(-0.0140371635832908,-0.0337936608885854,
-0.0120416859828794));
#23119=CARTESIAN_POINT('Ctrl Pts',(-0.0140367321926341,-0.0337934087472843,
-0.0120368320093285));
#23120=CARTESIAN_POINT('Ctrl Pts',(-0.0140356448539427,-0.0337928084291541,
-0.0120252214066319));
#23121=CARTESIAN_POINT('Ctrl Pts',(-0.0140349672922442,-0.0337924614498812,
-0.0120184668330488));
#23122=CARTESIAN_POINT('Ctrl Pts',(-0.0140324774597902,-0.0337912730439428,
-0.011995193433061));
#23123=CARTESIAN_POINT('Ctrl Pts',(-0.0140304428741404,-0.0337904432043666,
-0.0119786990361259));
#23124=CARTESIAN_POINT('Ctrl Pts',(-0.0140247383311923,-0.0337884139433801,
-0.0119378899774222));
#23125=CARTESIAN_POINT('Ctrl Pts',(-0.0140207528468879,-0.0337872283690468,
-0.0119136236248547));
#23126=CARTESIAN_POINT('Ctrl Pts',(-0.0140002426252975,-0.0337819784027302,
-0.0118050401417757));
#23127=CARTESIAN_POINT('Ctrl Pts',(-0.0139772724781112,-0.0337781107988135,
-0.0117220935218472));
#23128=CARTESIAN_POINT('Ctrl Pts',(-0.0139165116455943,-0.0337700608211633,
-0.011557501856301));
#23129=CARTESIAN_POINT('Ctrl Pts',(-0.0138782597787381,-0.0337658833867196,
-0.0114763810169881));
#23130=CARTESIAN_POINT('Ctrl Pts',(-0.0138247317664289,-0.033760621247134,
-0.0113845143151584));
#23131=CARTESIAN_POINT('Ctrl Pts',(-0.0138160316133676,-0.0337597811589592,
-0.0113701285287535));
#23132=CARTESIAN_POINT('Ctrl Pts',(-0.0138018848947561,-0.0337584372151351,
-0.0113475773850191));
#23133=CARTESIAN_POINT('Ctrl Pts',(-0.0137965923750887,-0.0337579390498095,
-0.0113393167031883));
#23134=CARTESIAN_POINT('Ctrl Pts',(-0.0137865544843974,-0.0337570024904676,
-0.0113239734654));
#23135=CARTESIAN_POINT('Ctrl Pts',(-0.0137818284774537,-0.0337565648356068,
-0.011316878652754));
#23136=CARTESIAN_POINT('Ctrl Pts',(-0.0137711240412606,-0.0337555806628813,
-0.0113010939356291));
#23137=CARTESIAN_POINT('Ctrl Pts',(-0.013765114847874,-0.0337550329841646,
-0.0112924254940682));
#23138=CARTESIAN_POINT('Ctrl Pts',(-0.0137469589305725,-0.0337533920624747,
-0.0112668002152122));
#23139=CARTESIAN_POINT('Ctrl Pts',(-0.0137345570805766,-0.0337522890333457,
-0.0112500278071728));
#23140=CARTESIAN_POINT('Ctrl Pts',(-0.013674332877356,-0.0337470129602141,
-0.0111719423609822));
#23141=CARTESIAN_POINT('Ctrl Pts',(-0.0136222660851279,-0.0337426732782518,
-0.0111140571079612));
#23142=CARTESIAN_POINT('Ctrl Pts',(-0.0135079316199637,-0.0337336529532164,
-0.0110047901133805));
#23143=CARTESIAN_POINT('Ctrl Pts',(-0.0134455451123945,-0.0337289797791893,
-0.0109538633562121));
#23144=CARTESIAN_POINT('Ctrl Pts',(-0.013341928536635,-0.0337218379014151,
-0.0108819856786954));
#23145=CARTESIAN_POINT('Ctrl Pts',(-0.013303240966222,-0.0337192938699135,
-0.0108576189863246));
#23146=CARTESIAN_POINT('Ctrl Pts',(-0.0132550454566685,-0.0337163205427813,
-0.0108301747966004));
#23147=CARTESIAN_POINT('Ctrl Pts',(-0.0132465190733556,-0.0337158017197733,
-0.010825426123517));
#23148=CARTESIAN_POINT('Ctrl Pts',(-0.0132330693701639,-0.0337149952521195,
-0.0108181017783727));
#23149=CARTESIAN_POINT('Ctrl Pts',(-0.0132281763531113,-0.0337147043097953,
-0.0108154713327942));
#23150=CARTESIAN_POINT('Ctrl Pts',(-0.013219436461792,-0.0337141891326061,
-0.010810833505208));
#23151=CARTESIAN_POINT('Ctrl Pts',(-0.0132155952971133,-0.0337139642644757,
-0.0108088159069703));
#23152=CARTESIAN_POINT('Ctrl Pts',(-0.0132062916312206,-0.0337134232949145,
-0.0108039790516885));
#23153=CARTESIAN_POINT('Ctrl Pts',(-0.0132008207429022,-0.0337131082220881,
-0.0108011762068581));
#23154=CARTESIAN_POINT('Ctrl Pts',(-0.0131837748718316,-0.0337121354963773,
-0.0107925714782024));
#23155=CARTESIAN_POINT('Ctrl Pts',(-0.0131721432418526,-0.0337114844918601,
-0.0107868824013671));
#23156=CARTESIAN_POINT('Ctrl Pts',(-0.0131122926196203,-0.0337081927678809,
-0.0107585371619461));
#23157=CARTESIAN_POINT('Ctrl Pts',(-0.013062991426041,-0.0337056715322415,
-0.0107382410928924));
#23158=CARTESIAN_POINT('Ctrl Pts',(-0.0129225442086121,-0.0336987596843853,
-0.0106887589465888));
#23159=CARTESIAN_POINT('Ctrl Pts',(-0.0128295948403706,-0.0336944792739199,
-0.010665435800378));
#23160=CARTESIAN_POINT('Ctrl Pts',(-0.0126769219728509,-0.0336872558351469,
-0.0106419006425537));
#23161=CARTESIAN_POINT('Ctrl Pts',(-0.0126183004437683,-0.0336844409819132,
-0.010636270161355));
#23162=CARTESIAN_POINT('Ctrl Pts',(-0.0125437949286773,-0.0336807405292667,
-0.0106333948137545));
#23163=CARTESIAN_POINT('Ctrl Pts',(-0.0125280780996695,-0.0336799532024085,
-0.0106330286907548));
#23164=CARTESIAN_POINT('Ctrl Pts',(-0.0125028790765382,-0.0336786790296563,
-0.0106328268508412));
#23165=CARTESIAN_POINT('Ctrl Pts',(-0.0124933990256157,-0.0336781969945015,
-0.0106328382858915));
#23166=CARTESIAN_POINT('Ctrl Pts',(-0.0124753438588177,-0.0336772736084814,
-0.0106330264557832));
#23167=CARTESIAN_POINT('Ctrl Pts',(-0.012466768913629,-0.0336768327744806,
-0.0106331873324422));
#23168=CARTESIAN_POINT('Ctrl Pts',(-0.0124471215681905,-0.0336758173059761,
-0.0106337198287589));
#23169=CARTESIAN_POINT('Ctrl Pts',(-0.0124360510243703,-0.0336752411879286,
-0.0106341392241955));
#23170=CARTESIAN_POINT('Ctrl Pts',(-0.0124013558395995,-0.0336734229251345,
-0.0106358279478391));
#23171=CARTESIAN_POINT('Ctrl Pts',(-0.0123777560685275,-0.0336721675905996,
-0.0106375213809762));
#23172=CARTESIAN_POINT('Ctrl Pts',(-0.0123223978071859,-0.0336691783284451,
-0.0106427755658311));
#23173=CARTESIAN_POINT('Ctrl Pts',(-0.012290693300643,-0.0336674315300226,
-0.0106467815580481));
#23174=CARTESIAN_POINT('Ctrl Pts',(-0.0121666504603399,-0.033660466405645,
-0.0106663849836567));
#23175=CARTESIAN_POINT('Ctrl Pts',(-0.0120756920903544,-0.0336550565078558,
-0.010689388851595));
#23176=CARTESIAN_POINT('Ctrl Pts',(-0.0119187425037636,-0.0336455029100956,
-0.0107446699532416));
#23177=CARTESIAN_POINT('Ctrl Pts',(-0.0118518857586418,-0.0336413623995634,
-0.0107736778824404));
#23178=CARTESIAN_POINT('Ctrl Pts',(-0.0117780852797928,-0.0336368928693253,
-0.0108121096941789));
#23179=CARTESIAN_POINT('Ctrl Pts',(-0.0117688974356628,-0.033636338385576,
-0.0108170131557909));
#23180=CARTESIAN_POINT('Ctrl Pts',(-0.0117547569759684,-0.0336354888936514,
-0.0108247447252493));
#23181=CARTESIAN_POINT('Ctrl Pts',(-0.0117497693724786,-0.0336351900180373,
-0.0108275078126939));
#23182=CARTESIAN_POINT('Ctrl Pts',(-0.0117406097014453,-0.0336346427005868,
-0.0108326487479675));
#23183=CARTESIAN_POINT('Ctrl Pts',(-0.0117364333805626,-0.0336343937747531,
-0.0108350184434727));
#23184=CARTESIAN_POINT('Ctrl Pts',(-0.0117268808787237,-0.0336338257764111,
-0.0108404977555914));
#23185=CARTESIAN_POINT('Ctrl Pts',(-0.0117215123532047,-0.0336335075426844,
-0.0108436203654327));
#23186=CARTESIAN_POINT('Ctrl Pts',(-0.0117047199848925,-0.0336325147617991,
-0.0108535238358687));
#23187=CARTESIAN_POINT('Ctrl Pts',(-0.0116933644961017,-0.0336318472632097,
-0.0108604200253056));
#23188=CARTESIAN_POINT('Ctrl Pts',(-0.01163440278987,-0.0336283941404489,
-0.0108972781421191));
#23189=CARTESIAN_POINT('Ctrl Pts',(-0.0115883683270542,-0.0336257413791545,
-0.010929682483491));
#23190=CARTESIAN_POINT('Ctrl Pts',(-0.0114667999306948,-0.0336185718693533,
-0.0110256063226618));
#23191=CARTESIAN_POINT('Ctrl Pts',(-0.0113954298323821,-0.0336141583269674,
-0.0110939588575385));
#23192=CARTESIAN_POINT('Ctrl Pts',(-0.0112963589614724,-0.0336070240749296,
-0.0112089382003157));
#23193=CARTESIAN_POINT('Ctrl Pts',(-0.0112637572688373,-0.0336044686101761,
-0.0112509858663945));
#23194=CARTESIAN_POINT('Ctrl Pts',(-0.0112246463162661,-0.0336010667294697,
-0.0113072011642105));
#23195=CARTESIAN_POINT('Ctrl Pts',(-0.0112160880000167,-0.0336002992132186,
-0.0113199014869486));
#23196=CARTESIAN_POINT('Ctrl Pts',(-0.0112025881226012,-0.0335990494464454,
-0.0113405930649407));
#23197=CARTESIAN_POINT('Ctrl Pts',(-0.0111975279256079,-0.0335985716741744,
-0.011348505894139));
#23198=CARTESIAN_POINT('Ctrl Pts',(-0.0111879737939721,-0.033597651277201,
-0.0113637509633083));
#23199=CARTESIAN_POINT('Ctrl Pts',(-0.0111834682876219,-0.033597209106703,
-0.0113710755563534));
#23200=CARTESIAN_POINT('Ctrl Pts',(-0.0111732076750668,-0.0335961829393702,
-0.011388072983773));
#23201=CARTESIAN_POINT('Ctrl Pts',(-0.0111674967588407,-0.0335955973507975,
-0.011397771811267));
#23202=CARTESIAN_POINT('Ctrl Pts',(-0.0111496234025559,-0.0335937173847962,
-0.0114289000305843));
#23203=CARTESIAN_POINT('Ctrl Pts',(-0.0111378683530392,-0.0335924085121383,
-0.0114505578961369));
#23204=CARTESIAN_POINT('Ctrl Pts',(-0.0110785156272132,-0.0335853981118196,
-0.0115664474891109));
#23205=CARTESIAN_POINT('Ctrl Pts',(-0.0110401697666802,-0.0335793807025071,
-0.0116650860648329));
#23206=CARTESIAN_POINT('Ctrl Pts',(-0.0109895189172441,-0.0335683883686168,
-0.011849335361499));
#23207=CARTESIAN_POINT('Ctrl Pts',(-0.0109737405501886,-0.0335634594430176,
-0.0119335698749898));
#23208=CARTESIAN_POINT('Ctrl Pts',(-0.0109635742156463,-0.0335580475888531,
-0.0120328573633552));
#23209=CARTESIAN_POINT('Ctrl Pts',(-0.0109623191989988,-0.0335572834824804,
-0.0120470518599872));
#23210=CARTESIAN_POINT('Ctrl Pts',(-0.0109607916799848,-0.0335561951365938,
-0.0120675635152863));
#23211=CARTESIAN_POINT('Ctrl Pts',(-0.0109603611184368,-0.0335558627866068,
-0.0120738677773221));
#23212=CARTESIAN_POINT('Ctrl Pts',(-0.010959670238414,-0.0335552805549607,
-0.0120849880868));
#23213=CARTESIAN_POINT('Ctrl Pts',(-0.0109593937543555,-0.033555029793311,
-0.0120898029700394));
#23214=CARTESIAN_POINT('Ctrl Pts',(-0.0109588473426091,-0.0335544929317273,
-0.0121001673960661));
#23215=CARTESIAN_POINT('Ctrl Pts',(-0.0109585848083938,-0.0335542072400902,
-0.0121057171591305));
#23216=CARTESIAN_POINT('Ctrl Pts',(-0.0109579324790847,-0.0335534103551736,
-0.0121212883021568));
#23217=CARTESIAN_POINT('Ctrl Pts',(-0.0109576103939953,-0.0335529027961535,
-0.0121313124070385));
#23218=CARTESIAN_POINT('Ctrl Pts',(-0.0109561078014767,-0.0335495345987556,
-0.0121984710539084));
#23219=CARTESIAN_POINT('Ctrl Pts',(-0.0109580043126801,-0.0335468234182701,
-0.0122556353169623));
#23220=CARTESIAN_POINT('Ctrl Pts',(-0.0109736621619191,-0.033538615021032,
-0.0124316602842457));
#23221=CARTESIAN_POINT('Ctrl Pts',(-0.0109980610362408,-0.0335333044598007,
-0.012549115392993));
#23222=CARTESIAN_POINT('Ctrl Pts',(-0.0110482585049746,-0.0335257098401372,
-0.0127001253793906));
#23223=CARTESIAN_POINT('Ctrl Pts',(-0.0110621786177751,-0.0335237848857979,
-0.0127371766791065));
#23224=CARTESIAN_POINT('Ctrl Pts',(-0.0110828785354006,-0.0335211215997775,
-0.0127864333521761));
#23225=CARTESIAN_POINT('Ctrl Pts',(-0.0110884224630571,-0.0335204248252831,
-0.0127991430291343));
#23226=CARTESIAN_POINT('Ctrl Pts',(-0.0110978801888293,-0.0335192619159308,
-0.0128200516521546));
#23227=CARTESIAN_POINT('Ctrl Pts',(-0.0111016965060982,-0.0335187991489379,
-0.0128282939608061));
#23228=CARTESIAN_POINT('Ctrl Pts',(-0.0111093233170813,-0.0335178865973378,
-0.0128443916800384));
#23229=CARTESIAN_POINT('Ctrl Pts',(-0.0111131281551799,-0.0335174370223177,
-0.0128522493996618));
#23230=CARTESIAN_POINT('Ctrl Pts',(-0.0111223562120245,-0.0335163597694635,
-0.0128709018638421));
#23231=CARTESIAN_POINT('Ctrl Pts',(-0.0111278398653843,-0.0335157299835402,
-0.0128816659281876));
#23232=CARTESIAN_POINT('Ctrl Pts',(-0.0111471980251655,-0.0335135411948309,
-0.0129185863769873));
#23233=CARTESIAN_POINT('Ctrl Pts',(-0.0111616979969911,-0.0335119601906147,
-0.0129444059604938));
#23234=CARTESIAN_POINT('Ctrl Pts',(-0.0111992267583206,-0.0335080038670154,
-0.0130069462784028));
#23235=CARTESIAN_POINT('Ctrl Pts',(-0.0112230761605314,-0.0335056014448284,
-0.0130431431185843));
#23236=CARTESIAN_POINT('Ctrl Pts',(-0.0112861775452646,-0.0334995236535978,
-0.0131306584133039));
#23237=CARTESIAN_POINT('Ctrl Pts',(-0.011327187965282,-0.0334958054491696,
-0.0131806065012802));
#23238=CARTESIAN_POINT('Ctrl Pts',(-0.0113876125062547,-0.0334907088480056,
-0.013245443063642));
#23239=CARTESIAN_POINT('Ctrl Pts',(-0.0114044308269542,-0.0334893267526076,
-0.0132626635002469));
#23240=CARTESIAN_POINT('Ctrl Pts',(-0.0114632168773144,-0.0334846341095007,
-0.013320103218506));
#23241=CARTESIAN_POINT('Ctrl Pts',(-0.0115070543606992,-0.0334813641346384,
-0.013358345275774));
#23242=CARTESIAN_POINT('Ctrl Pts',(-0.0115610136486099,-0.0334776949471436,
-0.0134002951954203));
#23243=CARTESIAN_POINT('Ctrl Pts',(-0.0115691408846366,-0.033477151274234,
-0.0134064851058104));
#23244=CARTESIAN_POINT('Ctrl Pts',(-0.0115818638775508,-0.0334763148016256,
-0.0134159770986217));
#23245=CARTESIAN_POINT('Ctrl Pts',(-0.0115864171951332,-0.0334760183111638,
-0.0134193352804976));
#23246=CARTESIAN_POINT('Ctrl Pts',(-0.0115948731107472,-0.0334754731476334,
-0.0134255002047708));
#23247=CARTESIAN_POINT('Ctrl Pts',(-0.0115987703768681,-0.0334752240205868,
-0.0134283137741033));
#23248=CARTESIAN_POINT('Ctrl Pts',(-0.0116077829487013,-0.0334746527395366,
-0.0134347564069586));
#23249=CARTESIAN_POINT('Ctrl Pts',(-0.0116129072875935,-0.0334743314629325,
-0.0134383725360855));
#23250=CARTESIAN_POINT('Ctrl Pts',(-0.0116292245495253,-0.0334733191286818,
-0.0134497388606907));
#23251=CARTESIAN_POINT('Ctrl Pts',(-0.0116404983402653,-0.0334726355212428,
-0.0134573724093256));
#23252=CARTESIAN_POINT('Ctrl Pts',(-0.0117013853385578,-0.0334690191951031,
-0.0134974343621052));
#23253=CARTESIAN_POINT('Ctrl Pts',(-0.0117527390760291,-0.0334662335974016,
-0.0135271357213447));
#23254=CARTESIAN_POINT('Ctrl Pts',(-0.0118955823028583,-0.0334588454306064,
-0.0135991112142569));
#23255=CARTESIAN_POINT('Ctrl Pts',(-0.0119897014924633,-0.033454335838558,
-0.0136355037320265));
#23256=CARTESIAN_POINT('Ctrl Pts',(-0.0121334190071866,-0.0334472899210698,
-0.0136754596367959));
#23257=CARTESIAN_POINT('Ctrl Pts',(-0.0121807256702241,-0.0334449496763278,
-0.013686238728406));
#23258=CARTESIAN_POINT('Ctrl Pts',(-0.0122430792972829,-0.0334417997756893,
-0.0136973858494454));
#23259=CARTESIAN_POINT('Ctrl Pts',(-0.012257736323028,-0.0334410548115421,
-0.0136997882847579));
#23260=CARTESIAN_POINT('Ctrl Pts',(-0.0122816167292075,-0.0334398327984506,
-0.0137033493112696));
#23261=CARTESIAN_POINT('Ctrl Pts',(-0.0122908200834134,-0.0334393598608983,
-0.0137046368278112));
#23262=CARTESIAN_POINT('Ctrl Pts',(-0.0123085933590506,-0.0334384425120381,
-0.0137069597509572));
#23263=CARTESIAN_POINT('Ctrl Pts',(-0.0123171614571464,-0.0334379984809096,
-0.0137080065330458));
#23264=CARTESIAN_POINT('Ctrl Pts',(-0.0123371456877173,-0.0334369584764007,
-0.0137102780305097));
#23265=CARTESIAN_POINT('Ctrl Pts',(-0.0123485675025721,-0.0334363607718203,
-0.0137114473120011));
#23266=CARTESIAN_POINT('Ctrl Pts',(-0.0123858296028133,-0.0334343997161618,
-0.0137148421654574));
#23267=CARTESIAN_POINT('Ctrl Pts',(-0.012411712177496,-0.0334330200571125,
-0.0137165436510788));
#23268=CARTESIAN_POINT('Ctrl Pts',(-0.0125237778463481,-0.0334269691166154,
-0.0137210776039364));
#23269=CARTESIAN_POINT('Ctrl Pts',(-0.0126100616949541,-0.0334221009520264,
-0.0137173352890856));
#23270=CARTESIAN_POINT('Ctrl Pts',(-0.0127992737083723,-0.0334111566346289,
-0.0136931581157646));
#23271=CARTESIAN_POINT('Ctrl Pts',(-0.0129013654514121,-0.0334050681875574,
-0.0136694016889682));
#23272=CARTESIAN_POINT('Ctrl Pts',(-0.0130127642015683,-0.0333986984259702,
-0.013631221352361));
#23273=CARTESIAN_POINT('Ctrl Pts',(-0.0130251994520558,-0.0333979916904246,
-0.0136267801943549));
#23274=CARTESIAN_POINT('Ctrl Pts',(-0.0130433836875074,-0.0333969662000074,
-0.0136200214033853));
#23275=CARTESIAN_POINT('Ctrl Pts',(-0.0130491778632807,-0.0333966406420563,
-0.0136178279945866));
#23276=CARTESIAN_POINT('Ctrl Pts',(-0.0130594382125888,-0.033396066486081,
-0.0136138730823058));
#23277=CARTESIAN_POINT('Ctrl Pts',(-0.0130639095641964,-0.0333958170813107,
-0.0136121255629249));
#23278=CARTESIAN_POINT('Ctrl Pts',(-0.0130736842136804,-0.0333952736610276,
-0.0136082526938462));
#23279=CARTESIAN_POINT('Ctrl Pts',(-0.0130789839112385,-0.0333949801621741,
-0.0136061187414957));
#23280=CARTESIAN_POINT('Ctrl Pts',(-0.0130942414297293,-0.0333941381531118,
-0.0135998765151017));
#23281=CARTESIAN_POINT('Ctrl Pts',(-0.0131041684233866,-0.0333935939679268,
-0.0135956932637267));
#23282=CARTESIAN_POINT('Ctrl Pts',(-0.013191282834957,-0.0333888440155744,
-0.0135579040065656));
#23283=CARTESIAN_POINT('Ctrl Pts',(-0.0132656523958536,-0.033384962121768,
-0.0135181333250506));
#23284=CARTESIAN_POINT('Ctrl Pts',(-0.013435825044743,-0.0333756910891636,
-0.0134083612398965));
#23285=CARTESIAN_POINT('Ctrl Pts',(-0.0135275244517434,-0.033370332225433,
-0.0133330203761054));
#23286=CARTESIAN_POINT('Ctrl Pts',(-0.0136239922957768,-0.0333635114639151,
-0.0132331671162951));
#23287=CARTESIAN_POINT('Ctrl Pts',(-0.0136379720976605,-0.0333624902858058,
-0.0132181059769125));
#23288=CARTESIAN_POINT('Ctrl Pts',(-0.0136587149173031,-0.0333609218855837,
-0.0131948437363644));
#23289=CARTESIAN_POINT('Ctrl Pts',(-0.013665701103049,-0.0333603840753491,
-0.0131868442496253));
#23290=CARTESIAN_POINT('Ctrl Pts',(-0.0136781483644111,-0.0333594080830567,
-0.013172291037784));
#23291=CARTESIAN_POINT('Ctrl Pts',(-0.0136836387638517,-0.0333589711435588,
-0.0131657628952886));
#23292=CARTESIAN_POINT('Ctrl Pts',(-0.0136952932600395,-0.0333580295591694,
-0.0131516699898979));
#23293=CARTESIAN_POINT('Ctrl Pts',(-0.0137014402686912,-0.0333575242451902,
-0.0131440916306087));
#23294=CARTESIAN_POINT('Ctrl Pts',(-0.0137181078465028,-0.0333561297419265,
-0.0131231398295445));
#23295=CARTESIAN_POINT('Ctrl Pts',(-0.0137284795161363,-0.0333552346712883,
-0.0131096501420463));
#23296=CARTESIAN_POINT('Ctrl Pts',(-0.0138016805908148,-0.0333487143003003,
-0.013011112033157));
#23297=CARTESIAN_POINT('Ctrl Pts',(-0.0138558340513196,-0.0333427500414317,
-0.0129199884605444));
#23298=CARTESIAN_POINT('Ctrl Pts',(-0.0139416967924835,-0.0333310089665558,
-0.0127345099440163));
#23299=CARTESIAN_POINT('Ctrl Pts',(-0.0139744683273538,-0.0333252803615069,
-0.0126411837191641));
#23300=CARTESIAN_POINT('Ctrl Pts',(-0.0140010448289976,-0.0333192715551104,
-0.0125334345461984));
#23301=CARTESIAN_POINT('Ctrl Pts',(-0.0140038444429358,-0.0333186127660152,
-0.012521471349666));
#23302=CARTESIAN_POINT('Ctrl Pts',(-0.0140078237389314,-0.0333176370673577,
-0.0125035024901238));
#23303=CARTESIAN_POINT('Ctrl Pts',(-0.0140091110093342,-0.0333173145791908,
-0.0124975214265061));
#23304=CARTESIAN_POINT('Ctrl Pts',(-0.0140113681965968,-0.0333167365986814,
-0.0124867219553947));
#23305=CARTESIAN_POINT('Ctrl Pts',(-0.014012350729376,-0.0333164804067694,
-0.0124819062695477));
#23306=CARTESIAN_POINT('Ctrl Pts',(-0.014014320135465,-0.0333159573369494,
-0.0124720125107152));
#23307=CARTESIAN_POINT('Ctrl Pts',(-0.0140153045087452,-0.0333156905993573,
-0.0124669340417576));
#23308=CARTESIAN_POINT('Ctrl Pts',(-0.0140177971545341,-0.0333150008298448,
-0.0124537188587988));
#23309=CARTESIAN_POINT('Ctrl Pts',(-0.0140192655620973,-0.0333145800056606,
-0.01244557469135));
#23310=CARTESIAN_POINT('Ctrl Pts',(-0.0140254881224478,-0.0333127280474943,
-0.0124093984920448));
#23311=CARTESIAN_POINT('Ctrl Pts',(-0.0140295327235197,-0.0333113330052668,
-0.0123812485367736));
#23312=CARTESIAN_POINT('Ctrl Pts',(-0.0140390255558211,-0.0333073550934322,
-0.0122991105353976));
#23313=CARTESIAN_POINT('Ctrl Pts',(-0.014042407755512,-0.0333048456618236,
-0.012244925585549));
#23314=CARTESIAN_POINT('Ctrl Pts',(-0.0140429762849904,-0.0333021306885963,
-0.0121857322010147));
#23315=CARTESIAN_POINT('Ctrl Pts',(-0.0140430000000311,-0.0333019043280856,
-0.0121807923972907));
#23316=CARTESIAN_POINT('Ctrl Pts',(-0.014043,-0.033301678145883,-0.0121758532768531));
#23317=CARTESIAN_POINT('Ctrl Pts',(-0.014043,-0.033417632014157,-0.012175853303277));
#23318=CARTESIAN_POINT('Ctrl Pts',(-0.014042999999715,-0.0334188419092182,
-0.0122021573362673));
#23319=CARTESIAN_POINT('Ctrl Pts',(-0.0140423273793937,-0.0334200590347099,
-0.0122284638982962));
#23320=CARTESIAN_POINT('Ctrl Pts',(-0.0140389460965616,-0.0334231503636634,
-0.0122945082372041));
#23321=CARTESIAN_POINT('Ctrl Pts',(-0.0140353724136637,-0.033425039819269,
-0.0123341737634836));
#23322=CARTESIAN_POINT('Ctrl Pts',(-0.0140266957573011,-0.0334283257145249,
-0.0124012996251137));
#23323=CARTESIAN_POINT('Ctrl Pts',(-0.0140223741544198,-0.0334296993693816,
-0.0124288410353687));
#23324=CARTESIAN_POINT('Ctrl Pts',(-0.0140151584755546,-0.0334316897198655,
-0.0124678872954614));
#23325=CARTESIAN_POINT('Ctrl Pts',(-0.0140128740083621,-0.0334322870973805,
-0.0124794999449829));
#23326=CARTESIAN_POINT('Ctrl Pts',(-0.014008675324236,-0.0334333319182327,
-0.0124996182548541));
#23327=CARTESIAN_POINT('Ctrl Pts',(-0.0140068221732928,-0.0334337773846008,
-0.0125081361819942));
#23328=CARTESIAN_POINT('Ctrl Pts',(-0.0140028609645677,-0.033434698758464,
-0.0125256287913865));
#23329=CARTESIAN_POINT('Ctrl Pts',(-0.0140007444563308,-0.0334351749235147,
-0.0125346011847215));
#23330=CARTESIAN_POINT('Ctrl Pts',(-0.01399512033785,-0.0334364006868484,
-0.012557522029801));
#23331=CARTESIAN_POINT('Ctrl Pts',(-0.0139914979243137,-0.0334371539753981,
-0.0125714411744428));
#23332=CARTESIAN_POINT('Ctrl Pts',(-0.0139760309415478,-0.0334402323152038,
-0.012627637821355));
#23333=CARTESIAN_POINT('Ctrl Pts',(-0.0139625798505904,-0.0334426089258601,
-0.0126694485361724));
#23334=CARTESIAN_POINT('Ctrl Pts',(-0.0139074519912897,-0.033451400066983,
-0.0128186523112334));
#23335=CARTESIAN_POINT('Ctrl Pts',(-0.0138555717064292,-0.0334581124628146,
-0.0129218640318063));
#23336=CARTESIAN_POINT('Ctrl Pts',(-0.0137620362154178,-0.033467880857382,
-0.0130653860550227));
#23337=CARTESIAN_POINT('Ctrl Pts',(-0.0137288184927417,-0.0334710344884734,
-0.0131107384041683));
#23338=CARTESIAN_POINT('Ctrl Pts',(-0.0136868438010502,-0.0334745851481467,
-0.0131619320091844));
#23339=CARTESIAN_POINT('Ctrl Pts',(-0.0136804134221039,-0.033475118115687,
-0.0131696206731239));
#23340=CARTESIAN_POINT('Ctrl Pts',(-0.0136702941516215,-0.0334759391892443,
-0.0131814832448776));
#23341=CARTESIAN_POINT('Ctrl Pts',(-0.0136666569165708,-0.0334762308525137,
-0.0131857006291432));
#23342=CARTESIAN_POINT('Ctrl Pts',(-0.0136598118447903,-0.0334767731568024,
-0.0131935511653801));
#23343=CARTESIAN_POINT('Ctrl Pts',(-0.0136566097213111,-0.0334770241765241,
-0.013197188902726));
#23344=CARTESIAN_POINT('Ctrl Pts',(-0.0136491606889585,-0.0334776020669154,
-0.0132055713334287));
#23345=CARTESIAN_POINT('Ctrl Pts',(-0.0136449014955317,-0.0334779280160911,
-0.0132103048868706));
#23346=CARTESIAN_POINT('Ctrl Pts',(-0.013630892009917,-0.0334789861369936,
-0.0132256821354219));
#23347=CARTESIAN_POINT('Ctrl Pts',(-0.0136210213926637,-0.0334797097806135,
-0.0132362156847351));
#23348=CARTESIAN_POINT('Ctrl Pts',(-0.0135574948811643,-0.0334842421627514,
-0.013302130046507));
#23349=CARTESIAN_POINT('Ctrl Pts',(-0.0134998936434749,-0.0334878013464259,
-0.0133535670668619));
#23350=CARTESIAN_POINT('Ctrl Pts',(-0.0133838259435214,-0.033494498834056,
-0.013442533214749));
#23351=CARTESIAN_POINT('Ctrl Pts',(-0.0133262059647764,-0.033497635548298,
-0.0134808474604466));
#23352=CARTESIAN_POINT('Ctrl Pts',(-0.0132316572462242,-0.0335027274604619,
-0.0135349381301696));
#23353=CARTESIAN_POINT('Ctrl Pts',(-0.0131963507202493,-0.0335046168328217,
-0.0135533616709764));
#23354=CARTESIAN_POINT('Ctrl Pts',(-0.0131351809564327,-0.0335079025972543,
-0.0135823279884092));
#23355=CARTESIAN_POINT('Ctrl Pts',(-0.0131096716356768,-0.0335092762070825,
-0.0135935719861557));
#23356=CARTESIAN_POINT('Ctrl Pts',(-0.0130729178359096,-0.0335112665035286,
-0.0136085968847154));
#23357=CARTESIAN_POINT('Ctrl Pts',(-0.013061912006056,-0.0335118638735136,
-0.013612948952185));
#23358=CARTESIAN_POINT('Ctrl Pts',(-0.0130427147053381,-0.0335129086855603,
-0.0136202859560935));
#23359=CARTESIAN_POINT('Ctrl Pts',(-0.0130345459058136,-0.0335133541507502,
-0.0136233289024706));
#23360=CARTESIAN_POINT('Ctrl Pts',(-0.0130176861602339,-0.0335142755262911,
-0.0136294471167212));
#23361=CARTESIAN_POINT('Ctrl Pts',(-0.0130089925738914,-0.0335147516942412,
-0.0136325140357905));
#23362=CARTESIAN_POINT('Ctrl Pts',(-0.0129866664023287,-0.033515977473795,
-0.0136401659834561));
#23363=CARTESIAN_POINT('Ctrl Pts',(-0.0129729964467952,-0.0335167307758543,
-0.0136446385682866));
#23364=CARTESIAN_POINT('Ctrl Pts',(-0.0129173494210471,-0.0335198092544095,
-0.0136619879616927));
#23365=CARTESIAN_POINT('Ctrl Pts',(-0.012874897064272,-0.0335221859962418,
-0.0136732605412862));
#23366=CARTESIAN_POINT('Ctrl Pts',(-0.0127195607234908,-0.0335309771661923,
-0.0137074877957652));
#23367=CARTESIAN_POINT('Ctrl Pts',(-0.0126046823233424,-0.03353768943338,
-0.0137195980135792));
#23368=CARTESIAN_POINT('Ctrl Pts',(-0.0124333780789518,-0.033547457663513,
-0.0137184372899149));
#23369=CARTESIAN_POINT('Ctrl Pts',(-0.012377268351593,-0.0335506112593318,
-0.0137149900401518));
#23370=CARTESIAN_POINT('Ctrl Pts',(-0.0123115119429668,-0.0335541618854092,
-0.0137073302557702));
#23371=CARTESIAN_POINT('Ctrl Pts',(-0.0123015678167686,-0.0335546948517647,
-0.0137060735758977));
#23372=CARTESIAN_POINT('Ctrl Pts',(-0.012286118348364,-0.0335555159239032,
-0.013703968024865));
#23373=CARTESIAN_POINT('Ctrl Pts',(-0.0122806043327708,-0.0335558075869195,
-0.013703186111275));
#23374=CARTESIAN_POINT('Ctrl Pts',(-0.0122702999158708,-0.0335563498910004,
-0.0137016679408443));
#23375=CARTESIAN_POINT('Ctrl Pts',(-0.0122655087430625,-0.033556600910764,
-0.0137009389689751));
#23376=CARTESIAN_POINT('Ctrl Pts',(-0.0122544304169177,-0.0335571788015811,
-0.0136991999723327));
#23377=CARTESIAN_POINT('Ctrl Pts',(-0.0122481459999849,-0.033557504751136,
-0.0136981735914326));
#23378=CARTESIAN_POINT('Ctrl Pts',(-0.012227637051582,-0.0335585628745932,
-0.0136946935597877));
#23379=CARTESIAN_POINT('Ctrl Pts',(-0.0122134401913984,-0.0335592865203315,
-0.0136920791455995));
#23380=CARTESIAN_POINT('Ctrl Pts',(-0.0121236375502395,-0.0335638196053332,
-0.0136742351652825));
#23381=CARTESIAN_POINT('Ctrl Pts',(-0.012049219097992,-0.0335673793955917,
-0.0136535527859177));
#23382=CARTESIAN_POINT('Ctrl Pts',(-0.0119116147336543,-0.0335740783763959,
-0.0136039400287943));
#23383=CARTESIAN_POINT('Ctrl Pts',(-0.0118482257695319,-0.0335772159632486,
-0.0135761457803177));
#23384=CARTESIAN_POINT('Ctrl Pts',(-0.0117516281924312,-0.033582307991978,
-0.0135258058932876));
#23385=CARTESIAN_POINT('Ctrl Pts',(-0.0117170666046765,-0.0335841964967042,
-0.0135060590744796));
#23386=CARTESIAN_POINT('Ctrl Pts',(-0.0116596674613333,-0.0335874808975805,
-0.0134702514521083));
#23387=CARTESIAN_POINT('Ctrl Pts',(-0.0116364315437997,-0.0335888540380433,
-0.0134548664953536));
#23388=CARTESIAN_POINT('Ctrl Pts',(-0.0116039396891384,-0.0335908437712065,
-0.013432063836645));
#23389=CARTESIAN_POINT('Ctrl Pts',(-0.0115943323557847,-0.0335914410626901,
-0.0134251551456082));
#23390=CARTESIAN_POINT('Ctrl Pts',(-0.0115777875821499,-0.0335924857829406,
-0.0134129665554057));
#23391=CARTESIAN_POINT('Ctrl Pts',(-0.0115708135968848,-0.0335929312358514,
-0.0134077370504474));
#23392=CARTESIAN_POINT('Ctrl Pts',(-0.011556555650037,-0.0335938526288993,
-0.0133968556421665));
#23393=CARTESIAN_POINT('Ctrl Pts',(-0.0115492772959708,-0.0335943288270915,
-0.0133911969947188));
#23394=CARTESIAN_POINT('Ctrl Pts',(-0.011530772971779,-0.0335955547758169,
-0.013376542632161));
#23395=CARTESIAN_POINT('Ctrl Pts',(-0.0115196214679203,-0.033596308218779,
-0.0133674546677911));
#23396=CARTESIAN_POINT('Ctrl Pts',(-0.0114749355659099,-0.0335993881443212,
-0.0133299858017371));
#23397=CARTESIAN_POINT('Ctrl Pts',(-0.0114424956041238,-0.0336017662541618,
-0.0133003366754625));
#23398=CARTESIAN_POINT('Ctrl Pts',(-0.0113297703865931,-0.033610557725176,
-0.0131881123875606));
#23399=CARTESIAN_POINT('Ctrl Pts',(-0.0112575279296278,-0.0336172686512803,
-0.0130980051100665));
#23400=CARTESIAN_POINT('Ctrl Pts',(-0.0111659648444407,-0.0336270351665792,
-0.0129532549765209));
#23401=CARTESIAN_POINT('Ctrl Pts',(-0.0111385523345016,-0.0336301883940965,
-0.0129041832623619));
#23402=CARTESIAN_POINT('Ctrl Pts',(-0.0111094718289135,-0.0336337386693752,
-0.012844718636034));
#23403=CARTESIAN_POINT('Ctrl Pts',(-0.0111051564731134,-0.0336342716233584,
-0.0128356721982252));
#23404=CARTESIAN_POINT('Ctrl Pts',(-0.0110985808396488,-0.0336350926806802,
-0.0128215345940113));
#23405=CARTESIAN_POINT('Ctrl Pts',(-0.011096259536667,-0.0336353843410538,
-0.0128164723054101));
#23406=CARTESIAN_POINT('Ctrl Pts',(-0.0110919694629843,-0.0336359266429641,
-0.0128069812409461));
#23407=CARTESIAN_POINT('Ctrl Pts',(-0.0110899941459429,-0.0336361776631654,
-0.0128025557517783));
#23408=CARTESIAN_POINT('Ctrl Pts',(-0.011085471687265,-0.0336367555584293,
-0.0127922940368988));
#23409=CARTESIAN_POINT('Ctrl Pts',(-0.0110829397880767,-0.0336370815119439,
-0.0127864512760361));
#23410=CARTESIAN_POINT('Ctrl Pts',(-0.0110747867227164,-0.0336381396620814,
-0.0127673129036136));
#23411=CARTESIAN_POINT('Ctrl Pts',(-0.011069315795437,-0.0336388633299439,
-0.0127539537098811));
#23412=CARTESIAN_POINT('Ctrl Pts',(-0.0110357453120358,-0.0336434051251161,
-0.0126685826950959));
#23413=CARTESIAN_POINT('Ctrl Pts',(-0.0110129004208285,-0.0336469724342582,
-0.0125946147937823));
#23414=CARTESIAN_POINT('Ctrl Pts',(-0.0109802591867677,-0.0336536893025543,
-0.0124516204862864));
#23415=CARTESIAN_POINT('Ctrl Pts',(-0.0109694007204777,-0.0336568370952115,
-0.0123830374474221));
#23416=CARTESIAN_POINT('Ctrl Pts',(-0.0109578583589872,-0.033662867374927,
-0.0122545964123853));
#23417=CARTESIAN_POINT('Ctrl Pts',(-0.0109559680881269,-0.0336657191615092,
-0.0121949800949101));
#23418=CARTESIAN_POINT('Ctrl Pts',(-0.0109579320381111,-0.0336694409500641,
-0.0121200821823339));
#23419=CARTESIAN_POINT('Ctrl Pts',(-0.0109585622387561,-0.0336702092552543,
-0.0121047644549504));
#23420=CARTESIAN_POINT('Ctrl Pts',(-0.0109599480973457,-0.0336714613173229,
-0.0120800518813177));
#23421=CARTESIAN_POINT('Ctrl Pts',(-0.0109605617835608,-0.0336719405977302,
-0.0120706499372031));
#23422=CARTESIAN_POINT('Ctrl Pts',(-0.0109619032267775,-0.0336728646172739,
-0.0120526381640575));
#23423=CARTESIAN_POINT('Ctrl Pts',(-0.0109626172731864,-0.0336733089064685,
-0.0120440276538187));
#23424=CARTESIAN_POINT('Ctrl Pts',(-0.0109644173049838,-0.0336743312285039,
-0.0120243315010868));
#23425=CARTESIAN_POINT('Ctrl Pts',(-0.0109655510803624,-0.0336749107517826,
-0.0120132507990589));
#23426=CARTESIAN_POINT('Ctrl Pts',(-0.0109689077681384,-0.033676472640218,
-0.0119836172109057));
#23427=CARTESIAN_POINT('Ctrl Pts',(-0.0109713478369917,-0.0336774617790287,
-0.0119650912064516));
#23428=CARTESIAN_POINT('Ctrl Pts',(-0.0109802070646319,-0.0336806516392054,
-0.0119061217256684));
#23429=CARTESIAN_POINT('Ctrl Pts',(-0.0109878995051436,-0.0336828908783642,
-0.0118658897870954));
#23430=CARTESIAN_POINT('Ctrl Pts',(-0.0110217486329495,-0.0336912025163248,
-0.0117204829739705));
#23431=CARTESIAN_POINT('Ctrl Pts',(-0.0110573619899019,-0.0336975190679095,
-0.011617837821735));
#23432=CARTESIAN_POINT('Ctrl Pts',(-0.0111191447161997,-0.033705797005906,
-0.0114863212448241));
#23433=CARTESIAN_POINT('Ctrl Pts',(-0.0111360622430286,-0.033707880701205,
-0.0114534338591265));
#23434=CARTESIAN_POINT('Ctrl Pts',(-0.0111650056310049,-0.0337111391680469,
-0.0114018170668279));
#23435=CARTESIAN_POINT('Ctrl Pts',(-0.0111762829698282,-0.0337123441092489,
-0.0113826853612786));
#23436=CARTESIAN_POINT('Ctrl Pts',(-0.0111919706851298,-0.0337139297716866,
-0.01135733871569));
#23437=CARTESIAN_POINT('Ctrl Pts',(-0.011196019296504,-0.0337143313642452,
-0.0113509041239544));
#23438=CARTESIAN_POINT('Ctrl Pts',(-0.0112028318730518,-0.033714994229264,
-0.0113402521433342));
#23439=CARTESIAN_POINT('Ctrl Pts',(-0.0112055692184076,-0.0337152572033376,
-0.0113360179612292));
#23440=CARTESIAN_POINT('Ctrl Pts',(-0.0112108000905011,-0.0337157532663478,
-0.0113280130731278));
#23441=CARTESIAN_POINT('Ctrl Pts',(-0.0112132895094078,-0.0337159866332001,
-0.0113242397893671));
#23442=CARTESIAN_POINT('Ctrl Pts',(-0.0112199471104154,-0.0337166037288225,
-0.0113142445091727));
#23443=CARTESIAN_POINT('Ctrl Pts',(-0.0112241441189503,-0.0337169855559622,
-0.0113080417513844));
#23444=CARTESIAN_POINT('Ctrl Pts',(-0.011239550772152,-0.0337183622793037,
-0.0112856256413522));
#23445=CARTESIAN_POINT('Ctrl Pts',(-0.0112510260667238,-0.0337193406966561,
-0.0112695963154988));
#23446=CARTESIAN_POINT('Ctrl Pts',(-0.0113224235834729,-0.033725179398347,
-0.0111737974155291));
#23447=CARTESIAN_POINT('Ctrl Pts',(-0.011389664513514,-0.0337296656966443,
-0.0110997673076007));
#23448=CARTESIAN_POINT('Ctrl Pts',(-0.0115345618938466,-0.0337386231585147,
-0.0109683946848047));
#23449=CARTESIAN_POINT('Ctrl Pts',(-0.0116113687685034,-0.0337430724518835,
-0.0109108003156418));
#23450=CARTESIAN_POINT('Ctrl Pts',(-0.0117074261725664,-0.0337486513555158,
-0.0108518586884018));
#23451=CARTESIAN_POINT('Ctrl Pts',(-0.0117219836650929,-0.0337494966413229,
-0.0108432522502181));
#23452=CARTESIAN_POINT('Ctrl Pts',(-0.0117451627903961,-0.0337508435852963,
-0.0108300579543876));
#23453=CARTESIAN_POINT('Ctrl Pts',(-0.0117536917629376,-0.0337513394191275,
-0.0108253095817266));
#23454=CARTESIAN_POINT('Ctrl Pts',(-0.0117697934074394,-0.0337522761326918,
-0.0108165443434453));
#23455=CARTESIAN_POINT('Ctrl Pts',(-0.0117773556368542,-0.0337527163268646,
-0.0108125090192861));
#23456=CARTESIAN_POINT('Ctrl Pts',(-0.0117944535217119,-0.0337537123320167,
-0.0108035675436729));
#23457=CARTESIAN_POINT('Ctrl Pts',(-0.0118040074254927,-0.0337542693933093,
-0.0107986974052046));
#23458=CARTESIAN_POINT('Ctrl Pts',(-0.0118329753618903,-0.0337559602952649,
-0.0107843093200875));
#23459=CARTESIAN_POINT('Ctrl Pts',(-0.0118525388697481,-0.033757104784583,
-0.0107750997396421));
#23460=CARTESIAN_POINT('Ctrl Pts',(-0.0119675842690624,-0.0337638519033324,
-0.0107238668266645));
#23461=CARTESIAN_POINT('Ctrl Pts',(-0.0120669245023405,-0.0337697712544364,
-0.0106912082172402));
#23462=CARTESIAN_POINT('Ctrl Pts',(-0.0122353051240417,-0.033779684491913,
-0.0106542013779307));
#23463=CARTESIAN_POINT('Ctrl Pts',(-0.0123027242863996,-0.0337836159000032,
-0.0106440011856401));
#23464=CARTESIAN_POINT('Ctrl Pts',(-0.0123923464125038,-0.0337886405261163,
-0.0106364585944451));
#23465=CARTESIAN_POINT('Ctrl Pts',(-0.0124141314467661,-0.0337898459711493,
-0.0106350898446689));
#23466=CARTESIAN_POINT('Ctrl Pts',(-0.0124511545656918,-0.0337918596321266,
-0.0106335514239226));
#23467=CARTESIAN_POINT('Ctrl Pts',(-0.0124663791902328,-0.0337926776652764,
-0.0106331444393136));
#23468=CARTESIAN_POINT('Ctrl Pts',(-0.0124881822396982,-0.0337938324114437,
-0.0106328845348419));
#23469=CARTESIAN_POINT('Ctrl Pts',(-0.0124947571425421,-0.0337941784545337,
-0.0106328481848931));
#23470=CARTESIAN_POINT('Ctrl Pts',(-0.0125061905878966,-0.0337947761740979,
-0.0106328580562863));
#23471=CARTESIAN_POINT('Ctrl Pts',(-0.0125110489899436,-0.0337950288887853,
-0.0106328851967611));
#23472=CARTESIAN_POINT('Ctrl Pts',(-0.0125214216370628,-0.0337955656459904,
-0.0106329921379444));
#23473=CARTESIAN_POINT('Ctrl Pts',(-0.0125269356490412,-0.0337958493240467,
-0.0106330785515137));
#23474=CARTESIAN_POINT('Ctrl Pts',(-0.0125419646913128,-0.0337966182824319,
-0.0106333946809437));
#23475=CARTESIAN_POINT('Ctrl Pts',(-0.0125514783926477,-0.0337971004190363,
-0.0106336828779773));
#23476=CARTESIAN_POINT('Ctrl Pts',(-0.0126017531627813,-0.033799626570421,
-0.0106356716065254));
#23477=CARTESIAN_POINT('Ctrl Pts',(-0.0126424404025149,-0.0338015957707894,
-0.010638900283556));
#23478=CARTESIAN_POINT('Ctrl Pts',(-0.0127661891140722,-0.0338074794338633,
-0.010653677495936));
#23479=CARTESIAN_POINT('Ctrl Pts',(-0.0128484785538294,-0.033811251827044,
-0.0106703833519706));
#23480=CARTESIAN_POINT('Ctrl Pts',(-0.0130051857784739,-0.033818746274944,
-0.0107157417095733));
#23481=CARTESIAN_POINT('Ctrl Pts',(-0.0130795463175328,-0.0338224497980643,
-0.010743630209548));
#23482=CARTESIAN_POINT('Ctrl Pts',(-0.0131705446041,-0.0338273786683246,
-0.0107860102765897));
#23483=CARTESIAN_POINT('Ctrl Pts',(-0.0131894749911651,-0.033828426377807,
-0.0107953034536584));
#23484=CARTESIAN_POINT('Ctrl Pts',(-0.0132176433641564,-0.0338300219940254,
-0.0108098555642873));
#23485=CARTESIAN_POINT('Ctrl Pts',(-0.0132270275509547,-0.0338305598023805,
-0.0108148269428763));
#23486=CARTESIAN_POINT('Ctrl Pts',(-0.0132438849536706,-0.033831537538864,
-0.0108239814327754));
#23487=CARTESIAN_POINT('Ctrl Pts',(-0.0132513761267323,-0.0338319762423345,
-0.010828130672073));
#23488=CARTESIAN_POINT('Ctrl Pts',(-0.0132673953666124,-0.0338329236224645,
-0.0108371785426421));
#23489=CARTESIAN_POINT('Ctrl Pts',(-0.0132759118848646,-0.033833432996384,
-0.0108420967647028));
#23490=CARTESIAN_POINT('Ctrl Pts',(-0.0132988510462349,-0.0338348207641835,
-0.0108556380148122));
#23491=CARTESIAN_POINT('Ctrl Pts',(-0.0133131805051868,-0.0338357047748763,
-0.0108644156046177));
#23492=CARTESIAN_POINT('Ctrl Pts',(-0.0134117859614017,-0.0338419097792291,
-0.0109270544155038));
#23493=CARTESIAN_POINT('Ctrl Pts',(-0.0134907816943701,-0.0338475313241312,
-0.0109887566480671));
#23494=CARTESIAN_POINT('Ctrl Pts',(-0.0136194032055111,-0.0338577131435112,
-0.0111110570263196));
#23495=CARTESIAN_POINT('Ctrl Pts',(-0.0136714618823321,-0.0338622066619729,
-0.0111686133915369));
#23496=CARTESIAN_POINT('Ctrl Pts',(-0.0137333073952456,-0.0338678574080462,
-0.0112483037142908));
#23497=CARTESIAN_POINT('Ctrl Pts',(-0.0137472171817328,-0.0338691516903793,
-0.0112670932872624));
#23498=CARTESIAN_POINT('Ctrl Pts',(-0.0137699340005241,-0.033871296376397,
-0.0112992841885698));
#23499=CARTESIAN_POINT('Ctrl Pts',(-0.0137789686231406,-0.0338721582173478,
-0.0113125196026057));
#23500=CARTESIAN_POINT('Ctrl Pts',(-0.0137914911886668,-0.0338733629044542,
-0.011331492868959));
#23501=CARTESIAN_POINT('Ctrl Pts',(-0.0137951501211502,-0.0338737161772758,
-0.0113371160379705));
#23502=CARTESIAN_POINT('Ctrl Pts',(-0.0138014056211775,-0.0338743221276717,
-0.0113468682465799));
#23503=CARTESIAN_POINT('Ctrl Pts',(-0.0138040194736659,-0.0338745759284721,
-0.0113509860232788));
#23504=CARTESIAN_POINT('Ctrl Pts',(-0.013809510697429,-0.0338751103286701,
-0.0113597280549905));
#23505=CARTESIAN_POINT('Ctrl Pts',(-0.0138123831523895,-0.0338753906142976,
-0.0113643552130005));
#23506=CARTESIAN_POINT('Ctrl Pts',(-0.0138201750183855,-0.0338761532393882,
-0.0113770564977198));
#23507=CARTESIAN_POINT('Ctrl Pts',(-0.013825044888757,-0.0338766324508055,
-0.0113851609062188));
#23508=CARTESIAN_POINT('Ctrl Pts',(-0.0138492075520212,-0.0338790259337489,
-0.011426222491462));
#23509=CARTESIAN_POINT('Ctrl Pts',(-0.013867347903725,-0.0338808749196336,
-0.011459845278926));
#23510=CARTESIAN_POINT('Ctrl Pts',(-0.0139220774965238,-0.033886742484643,
-0.0115709689639838));
#23511=CARTESIAN_POINT('Ctrl Pts',(-0.0139534663360998,-0.0338905970346306,
-0.0116508518520702));
#23512=CARTESIAN_POINT('Ctrl Pts',(-0.0140032783571748,-0.0338985654211833,
-0.0118170778931771));
#23513=CARTESIAN_POINT('Ctrl Pts',(-0.0140212604602887,-0.0339026720376336,
-0.0119032179818425));
#23514=CARTESIAN_POINT('Ctrl Pts',(-0.014033824569558,-0.0339078493565943,
-0.0120070029145103));
#23515=CARTESIAN_POINT('Ctrl Pts',(-0.0140355632349712,-0.0339086849332264,
-0.0120236239127629));
#23516=CARTESIAN_POINT('Ctrl Pts',(-0.0140378855705759,-0.0339100199072247,
-0.0120499508257753));
#23517=CARTESIAN_POINT('Ctrl Pts',(-0.0140386480739004,-0.0339105136584508,
-0.0120596398757809));
#23518=CARTESIAN_POINT('Ctrl Pts',(-0.014039911085653,-0.0339114486147741,
-0.0120778919923943));
#23519=CARTESIAN_POINT('Ctrl Pts',(-0.0140404318250625,-0.0339118891627012,
-0.0120864533131702));
#23520=CARTESIAN_POINT('Ctrl Pts',(-0.0140414463073588,-0.0339128889318733,
-0.0121057914610266));
#23521=CARTESIAN_POINT('Ctrl Pts',(-0.0140418984581002,-0.0339134494426792,
-0.0121165699432197));
#23522=CARTESIAN_POINT('Ctrl Pts',(-0.014042745840595,-0.0339148590888116,
-0.0121435149562545));
#23523=CARTESIAN_POINT('Ctrl Pts',(-0.0140430000000035,-0.0339157125708919,
-0.0121596840009703));
#23524=CARTESIAN_POINT('Ctrl Pts',(-0.014043,-0.0339165738369763,-0.0121758532868962));
#23525=CARTESIAN_POINT('Origin',(-0.0125,-0.0375520664398416,-0.0121758532865581));
#23526=CARTESIAN_POINT('',(-0.014043,-0.0344186209509151,-0.012175853286558));
#23527=CARTESIAN_POINT('',(-0.014043,-0.0343031952477557,-0.0121758532813813));
#23528=CARTESIAN_POINT('',(-0.014043,-0.0375520664398416,-0.012175853286558));
#23529=CARTESIAN_POINT('Ctrl Pts',(-0.014043,-0.0343031952477557,-0.0121758532762046));
#23530=CARTESIAN_POINT('Ctrl Pts',(-0.0140429999999155,-0.0343025001782861,
-0.0121632591726524));
#23531=CARTESIAN_POINT('Ctrl Pts',(-0.0140428458087414,-0.0343018010815279,
-0.0121506642448564));
#23532=CARTESIAN_POINT('Ctrl Pts',(-0.014040120579621,-0.0342955917809417,
-0.0120394004326745));
#23533=CARTESIAN_POINT('Ctrl Pts',(-0.0140282417712872,-0.0342898578569338,
-0.0119411935070349));
#23534=CARTESIAN_POINT('Ctrl Pts',(-0.0139949955681177,-0.0342809983564059,
-0.011789843232452));
#23535=CARTESIAN_POINT('Ctrl Pts',(-0.0139799239403911,-0.0342778221547362,
-0.0117355787661732));
#23536=CARTESIAN_POINT('Ctrl Pts',(-0.0139576695576264,-0.034274058406594,
-0.0116696665560275));
#23537=CARTESIAN_POINT('Ctrl Pts',(-0.013953256529049,-0.03427334709226,
-0.011657132716861));
#23538=CARTESIAN_POINT('Ctrl Pts',(-0.0139465438191688,-0.0342723162749851,
-0.0116388257687814));
#23539=CARTESIAN_POINT('Ctrl Pts',(-0.0139443704074148,-0.0342719898716033,
-0.0116330073559015));
#23540=CARTESIAN_POINT('Ctrl Pts',(-0.0139404544759888,-0.0342714148059591,
-0.0116227140995119));
#23541=CARTESIAN_POINT('Ctrl Pts',(-0.0139387261284921,-0.0342711653269669,
-0.0116182340736097));
#23542=CARTESIAN_POINT('Ctrl Pts',(-0.0139348999118669,-0.0342706224223885,
-0.0116084524157116));
#23543=CARTESIAN_POINT('Ctrl Pts',(-0.0139327935552788,-0.0342703295055538,
-0.0116031542946884));
#23544=CARTESIAN_POINT('Ctrl Pts',(-0.013926757549759,-0.0342695063942333,
-0.0115882136773387));
#23545=CARTESIAN_POINT('Ctrl Pts',(-0.0139227595288143,-0.0342689801383092,
-0.0115785989433625));
#23546=CARTESIAN_POINT('Ctrl Pts',(-0.0138901791117773,-0.0342648331201147,
-0.0115024312836866));
#23547=CARTESIAN_POINT('Ctrl Pts',(-0.0138570370162666,-0.034261452496981,
-0.0114379184286584));
#23548=CARTESIAN_POINT('Ctrl Pts',(-0.0137708047440976,-0.034253803946893,
-0.0112956707371701));
#23549=CARTESIAN_POINT('Ctrl Pts',(-0.0137149017722829,-0.0342495768176398,
-0.011219987504965));
#23550=CARTESIAN_POINT('Ctrl Pts',(-0.013631191248228,-0.0342436222914258,
-0.0111259585078482));
#23551=CARTESIAN_POINT('Ctrl Pts',(-0.0136091792952162,-0.0342420871570714,
-0.0111027298897534));
#23552=CARTESIAN_POINT('Ctrl Pts',(-0.0135696450220958,-0.0342393658079462,
-0.0110635271549066));
#23553=CARTESIAN_POINT('Ctrl Pts',(-0.0135524469812946,-0.0342381929600111,
-0.0110472412306433));
#23554=CARTESIAN_POINT('Ctrl Pts',(-0.0135266609059339,-0.0342364463305617,
-0.0110239248097739));
#23555=CARTESIAN_POINT('Ctrl Pts',(-0.0135183606171101,-0.0342358858573487,
-0.0110165804642149));
#23556=CARTESIAN_POINT('Ctrl Pts',(-0.0135034977590349,-0.0342348849638155,
-0.0110037121635231));
#23557=CARTESIAN_POINT('Ctrl Pts',(-0.0134969668436084,-0.0342344460680893,
-0.0109981522746276));
#23558=CARTESIAN_POINT('Ctrl Pts',(-0.013483122355339,-0.0342335174184684,
-0.0109865638938266));
#23559=CARTESIAN_POINT('Ctrl Pts',(-0.0134757989300945,-0.0342330271846811,
-0.0109805477742034));
#23560=CARTESIAN_POINT('Ctrl Pts',(-0.0134561905046735,-0.0342317170125173,
-0.0109647399525555));
#23561=CARTESIAN_POINT('Ctrl Pts',(-0.0134438108191034,-0.0342308923214378,
-0.0109550679237343));
#23562=CARTESIAN_POINT('Ctrl Pts',(-0.0133845203030087,-0.0342269531238785,
-0.0109101862460423));
#23563=CARTESIAN_POINT('Ctrl Pts',(-0.0133357789788223,-0.0342237427947477,
-0.0108774844912127));
#23564=CARTESIAN_POINT('Ctrl Pts',(-0.0132028632044925,-0.0342150854732618,
-0.0107988988580127));
#23565=CARTESIAN_POINT('Ctrl Pts',(-0.0131160715130319,-0.0342095165175969,
-0.0107579414345621));
#23566=CARTESIAN_POINT('Ctrl Pts',(-0.0129759041915379,-0.034201005896186,
-0.0107071089824328));
#23567=CARTESIAN_POINT('Ctrl Pts',(-0.0129248420221395,-0.0341980026431484,
-0.0106915336481659));
#23568=CARTESIAN_POINT('Ctrl Pts',(-0.0128605010395783,-0.0341944181106357,
-0.0106755013799547));
#23569=CARTESIAN_POINT('Ctrl Pts',(-0.0128478906298712,-0.0341937249746895,
-0.0106725273157621));
#23570=CARTESIAN_POINT('Ctrl Pts',(-0.0128292422996723,-0.0341927153295564,
-0.0106683764836284));
#23571=CARTESIAN_POINT('Ctrl Pts',(-0.0128232327044016,-0.0341923923028462,
-0.0106670764890774));
#23572=CARTESIAN_POINT('Ctrl Pts',(-0.0128129690918423,-0.0341918447957871,
-0.0106649204044006));
#23573=CARTESIAN_POINT('Ctrl Pts',(-0.0128087190292513,-0.0341916193048559,
-0.0106640462918413));
#23574=CARTESIAN_POINT('Ctrl Pts',(-0.0127990202809435,-0.0341911075549493,
-0.0106620941512873));
#23575=CARTESIAN_POINT('Ctrl Pts',(-0.0127935694186492,-0.0341908219498469,
-0.0106610276047234));
#23576=CARTESIAN_POINT('Ctrl Pts',(-0.01277852983684,-0.0341900391665776,
-0.0106581691029102));
#23577=CARTESIAN_POINT('Ctrl Pts',(-0.0127689295492263,-0.0341895453411792,
-0.0106564385774857));
#23578=CARTESIAN_POINT('Ctrl Pts',(-0.012714358969439,-0.0341867682217497,
-0.0106471352430246));
#23579=CARTESIAN_POINT('Ctrl Pts',(-0.0126690833101511,-0.0341845788641603,
-0.0106414673787615));
#23580=CARTESIAN_POINT('Ctrl Pts',(-0.0125434049372057,-0.0341786597351835,
-0.0106313659900271));
#23581=CARTESIAN_POINT('Ctrl Pts',(-0.0124628061911458,-0.0341750358121085,
-0.0106312036349826));
#23582=CARTESIAN_POINT('Ctrl Pts',(-0.0123050045562738,-0.0341677598296407,
-0.0106432490600485));
#23583=CARTESIAN_POINT('Ctrl Pts',(-0.0122280131332436,-0.0341641222036786,
-0.0106550243931813));
#23584=CARTESIAN_POINT('Ctrl Pts',(-0.0121319177140237,-0.0341592772142508,
-0.0106772540591647));
#23585=CARTESIAN_POINT('Ctrl Pts',(-0.012111690785222,-0.0341582403689585,
-0.0106823673927283));
#23586=CARTESIAN_POINT('Ctrl Pts',(-0.012081402302508,-0.0341566593984008,
-0.0106906811641245));
#23587=CARTESIAN_POINT('Ctrl Pts',(-0.0120712593558486,-0.0341561251314964,
-0.0106935774288066));
#23588=CARTESIAN_POINT('Ctrl Pts',(-0.0120529743466897,-0.0341551529170905,
-0.0106990019950824));
#23589=CARTESIAN_POINT('Ctrl Pts',(-0.0120448219774238,-0.0341547161680707,
-0.010701494227259));
#23590=CARTESIAN_POINT('Ctrl Pts',(-0.0120273333812615,-0.0341537720022813,
-0.0107069994799274));
#23591=CARTESIAN_POINT('Ctrl Pts',(-0.012018004432477,-0.0341532638825246,
-0.010710034230663));
#23592=CARTESIAN_POINT('Ctrl Pts',(-0.0119927710666613,-0.0341518770894466,
-0.0107185096929943));
#23593=CARTESIAN_POINT('Ctrl Pts',(-0.011976925905318,-0.0341509927790022,
-0.0107241215614215));
#23594=CARTESIAN_POINT('Ctrl Pts',(-0.011873853308883,-0.034145150004962,
-0.0107625332350306));
#23595=CARTESIAN_POINT('Ctrl Pts',(-0.0117896707683111,-0.034139933704283,
-0.0108029144086997));
#23596=CARTESIAN_POINT('Ctrl Pts',(-0.0116195660128787,-0.0341285959118747,
-0.0109043629369295));
#23597=CARTESIAN_POINT('Ctrl Pts',(-0.0115351884367015,-0.0341224712879432,
-0.0109671383273606));
#23598=CARTESIAN_POINT('Ctrl Pts',(-0.0114444985879512,-0.0341157494274545,
-0.0110502011985624));
#23599=CARTESIAN_POINT('Ctrl Pts',(-0.0114313814725755,-0.0341147739626844,
-0.0110626460495307));
#23600=CARTESIAN_POINT('Ctrl Pts',(-0.0114134820691962,-0.0341134421749624,
-0.0110802361096432));
#23601=CARTESIAN_POINT('Ctrl Pts',(-0.0114085120577957,-0.0341130723119575,
-0.0110851873028349));
#23602=CARTESIAN_POINT('Ctrl Pts',(-0.0114001199648845,-0.0341124479396526,
-0.0110936624379642));
#23603=CARTESIAN_POINT('Ctrl Pts',(-0.0113966806506289,-0.0341121921031992,
-0.0110971691158545));
#23604=CARTESIAN_POINT('Ctrl Pts',(-0.0113895795570858,-0.034111664086293,
-0.0111044787913426));
#23605=CARTESIAN_POINT('Ctrl Pts',(-0.0113859204782858,-0.0341113921050778,
-0.0111082842302582));
#23606=CARTESIAN_POINT('Ctrl Pts',(-0.0113762430693028,-0.0341106727974637,
-0.0111184526689691));
#23607=CARTESIAN_POINT('Ctrl Pts',(-0.0113702591797555,-0.0341102280436273,
-0.0111248483430431));
#23608=CARTESIAN_POINT('Ctrl Pts',(-0.0113438122980292,-0.0341082606183883,
-0.0111536020519938));
#23609=CARTESIAN_POINT('Ctrl Pts',(-0.0113239551060861,-0.0341067786152503,
-0.0111765103943231));
#23610=CARTESIAN_POINT('Ctrl Pts',(-0.0112469980073477,-0.0341009473641577,
-0.0112707657352405));
#23611=CARTESIAN_POINT('Ctrl Pts',(-0.0111956085801621,-0.0340968387689115,
-0.0113465386881616));
#23612=CARTESIAN_POINT('Ctrl Pts',(-0.0111069104476058,-0.0340884633623077,
-0.0115061707450445));
#23613=CARTESIAN_POINT('Ctrl Pts',(-0.0110697609084799,-0.0340842097093618,
-0.0115896903431503));
#23614=CARTESIAN_POINT('Ctrl Pts',(-0.011034779142933,-0.0340788625490606,
-0.0116918514858917));
#23615=CARTESIAN_POINT('Ctrl Pts',(-0.0110296085039665,-0.0340780245885084,
-0.0117077948247062));
#23616=CARTESIAN_POINT('Ctrl Pts',(-0.0110218560302274,-0.0340766879942518,
-0.0117330965129598));
#23617=CARTESIAN_POINT('Ctrl Pts',(-0.0110191009637645,-0.034076195065444,
-0.011742400642326));
#23618=CARTESIAN_POINT('Ctrl Pts',(-0.0110140874660354,-0.0340752630514139,
-0.0117599376549591));
#23619=CARTESIAN_POINT('Ctrl Pts',(-0.0110118092392667,-0.0340748246351806,
-0.0117681645241889));
#23620=CARTESIAN_POINT('Ctrl Pts',(-0.0110068294485792,-0.0340738316198713,
-0.0117867450807002));
#23621=CARTESIAN_POINT('Ctrl Pts',(-0.0110041671026767,-0.034073275767296,
-0.0117971087460061));
#23622=CARTESIAN_POINT('Ctrl Pts',(-0.0109964463349754,-0.0340715850131807,
-0.0118285152010133));
#23623=CARTESIAN_POINT('Ctrl Pts',(-0.0109917227785662,-0.0340704394205825,
-0.0118496369038934));
#23624=CARTESIAN_POINT('Ctrl Pts',(-0.0109671718474253,-0.0340637851152729,
-0.0119713885849393));
#23625=CARTESIAN_POINT('Ctrl Pts',(-0.0109569757564983,-0.0340579714105121,
-0.012073683851691));
#23626=CARTESIAN_POINT('Ctrl Pts',(-0.0109570221828998,-0.034046703314225,
-0.0122696877500179));
#23627=CARTESIAN_POINT('Ctrl Pts',(-0.0109655372081662,-0.0340412926146118,
-0.0123629673414816));
#23628=CARTESIAN_POINT('Ctrl Pts',(-0.0109847321391462,-0.0340355405047427,
-0.0124673536575062));
#23629=CARTESIAN_POINT('Ctrl Pts',(-0.0109871739779461,-0.0340348613835662,
-0.0124797720309346));
#23630=CARTESIAN_POINT('Ctrl Pts',(-0.0109910408991057,-0.0340338608848952,
-0.0124982349931949));
#23631=CARTESIAN_POINT('Ctrl Pts',(-0.0109923500721701,-0.0340335335474189,
-0.0125043030249268));
#23632=CARTESIAN_POINT('Ctrl Pts',(-0.010994669976286,-0.034032972777018,
-0.0125147495982409));
#23633=CARTESIAN_POINT('Ctrl Pts',(-0.0109956632707457,-0.0340327383782787,
-0.0125191318853797));
#23634=CARTESIAN_POINT('Ctrl Pts',(-0.0109978086250615,-0.0340322440592089,
-0.012528408751749));
#23635=CARTESIAN_POINT('Ctrl Pts',(-0.0109989654948077,-0.0340319844292006,
-0.0125333021616155));
#23636=CARTESIAN_POINT('Ctrl Pts',(-0.011001932652963,-0.0340313353815449,
-0.0125455843965908));
#23637=CARTESIAN_POINT('Ctrl Pts',(-0.0110037737244983,-0.0340309476997052,
-0.0125529657460045));
#23638=CARTESIAN_POINT('Ctrl Pts',(-0.0110112515671131,-0.0340294295694962,
-0.0125820293341924));
#23639=CARTESIAN_POINT('Ctrl Pts',(-0.0110173059019867,-0.0340283210758478,
-0.0126036022626613));
#23640=CARTESIAN_POINT('Ctrl Pts',(-0.0110347453129404,-0.0340254072208504,
-0.0126609141907877));
#23641=CARTESIAN_POINT('Ctrl Pts',(-0.0110469673856446,-0.0340236364636228,
-0.0126963836774273));
#23642=CARTESIAN_POINT('Ctrl Pts',(-0.0111011427833561,-0.0340166364647975,
-0.0128367691975007));
#23643=CARTESIAN_POINT('Ctrl Pts',(-0.0111532656534442,-0.0340116126488013,
-0.0129373773537217));
#23644=CARTESIAN_POINT('Ctrl Pts',(-0.0112416655960233,-0.0340040648823587,
-0.0130700578661278));
#23645=CARTESIAN_POINT('Ctrl Pts',(-0.0112691559250478,-0.0340018188346173,
-0.0131075343881972));
#23646=CARTESIAN_POINT('Ctrl Pts',(-0.0113074673874814,-0.0339987799213331,
-0.0131551024233376));
#23647=CARTESIAN_POINT('Ctrl Pts',(-0.0113168025875147,-0.0339980460281833,
-0.0131663616248628));
#23648=CARTESIAN_POINT('Ctrl Pts',(-0.0113322971197394,-0.0339968376225824,
-0.0131845179682216));
#23649=CARTESIAN_POINT('Ctrl Pts',(-0.0113383609892643,-0.0339963670458924,
-0.0131914955761731));
#23650=CARTESIAN_POINT('Ctrl Pts',(-0.0113502199331881,-0.0339954510291983,
-0.0132048963517449));
#23651=CARTESIAN_POINT('Ctrl Pts',(-0.0113560070553403,-0.0339950059318243,
-0.0132113261111845));
#23652=CARTESIAN_POINT('Ctrl Pts',(-0.01136968279182,-0.0339939583872156,
-0.0132262658976273));
#23653=CARTESIAN_POINT('Ctrl Pts',(-0.0113776138723128,-0.0339933541328016,
-0.0132347361955889));
#23654=CARTESIAN_POINT('Ctrl Pts',(-0.0114040767878785,-0.0339913481755186,
-0.0132623669024121));
#23655=CARTESIAN_POINT('Ctrl Pts',(-0.0114230088841539,-0.0339899291129235,
-0.0132811358483241));
#23656=CARTESIAN_POINT('Ctrl Pts',(-0.0114697181287215,-0.0339864645574422,
-0.0133251026197715));
#23657=CARTESIAN_POINT('Ctrl Pts',(-0.0114979453942418,-0.0339843999464167,
-0.0133497958032575));
#23658=CARTESIAN_POINT('Ctrl Pts',(-0.011637651110176,-0.0339743343944601,
-0.0134632976154327));
#23659=CARTESIAN_POINT('Ctrl Pts',(-0.0117601616082825,-0.0339658753144117,
-0.0135373937570606));
#23660=CARTESIAN_POINT('Ctrl Pts',(-0.0119093496999108,-0.0339569652999109,
-0.0136014675862712));
#23661=CARTESIAN_POINT('Ctrl Pts',(-0.0119277598477927,-0.0339558895009686,
-0.0136089566285915));
#23662=CARTESIAN_POINT('Ctrl Pts',(-0.0119533035028888,-0.0339544343401563,
-0.013618776733013));
#23663=CARTESIAN_POINT('Ctrl Pts',(-0.011960316297486,-0.0339540386794832,
-0.013621414298075));
#23664=CARTESIAN_POINT('Ctrl Pts',(-0.011971578654342,-0.0339534097221458,
-0.0136255567734038));
#23665=CARTESIAN_POINT('Ctrl Pts',(-0.0119758159973781,-0.0339531745402035,
-0.0136270942902337));
#23666=CARTESIAN_POINT('Ctrl Pts',(-0.0119847782164407,-0.0339526802831967,
-0.0136303018508139));
#23667=CARTESIAN_POINT('Ctrl Pts',(-0.0119895046014784,-0.0339524214839101,
-0.0136319674858335));
#23668=CARTESIAN_POINT('Ctrl Pts',(-0.0120013490607268,-0.0339517773686502,
-0.0136360768577345));
#23669=CARTESIAN_POINT('Ctrl Pts',(-0.0120084771505703,-0.0339513937330016,
-0.0136384916321495));
#23670=CARTESIAN_POINT('Ctrl Pts',(-0.0120362812142936,-0.033949911808473,
-0.0136476845653664));
#23671=CARTESIAN_POINT('Ctrl Pts',(-0.0120570828194464,-0.0339488341641262,
-0.0136540775205268));
#23672=CARTESIAN_POINT('Ctrl Pts',(-0.0121125738806857,-0.0339460245121221,
-0.0136698549496255));
#23673=CARTESIAN_POINT('Ctrl Pts',(-0.0121474686241941,-0.0339443241260699,
-0.0136784716199955));
#23674=CARTESIAN_POINT('Ctrl Pts',(-0.0122472492148597,-0.0339395714174577,
-0.0136994429950605));
#23675=CARTESIAN_POINT('Ctrl Pts',(-0.012312670921864,-0.0339365821794981,
-0.0137088623568889));
#23676=CARTESIAN_POINT('Ctrl Pts',(-0.0124695198751476,-0.0339293672839225,
-0.0137212519344233));
#23677=CARTESIAN_POINT('Ctrl Pts',(-0.0125609950934298,-0.0339251121722748,
-0.013720347791863));
#23678=CARTESIAN_POINT('Ctrl Pts',(-0.012668527312152,-0.0339197637057954,
-0.0137097139447504));
#23679=CARTESIAN_POINT('Ctrl Pts',(-0.0126851797925043,-0.0339189260030248,
-0.0137077927078329));
#23680=CARTESIAN_POINT('Ctrl Pts',(-0.0127115127304582,-0.0339175850251615,
-0.0137043189870211));
#23681=CARTESIAN_POINT('Ctrl Pts',(-0.0127212156050764,-0.0339170873970374,
-0.0137029448630254));
#23682=CARTESIAN_POINT('Ctrl Pts',(-0.0127393343318218,-0.0339161513139628,
-0.0137002025791944));
#23683=CARTESIAN_POINT('Ctrl Pts',(-0.0127477532388353,-0.0339157135910384,
-0.0136988569034629));
#23684=CARTESIAN_POINT('Ctrl Pts',(-0.0127665763240518,-0.0339147285598326,
-0.0136956880238568));
#23685=CARTESIAN_POINT('Ctrl Pts',(-0.0127769737358373,-0.0339141800816312,
-0.0136938276300223));
#23686=CARTESIAN_POINT('Ctrl Pts',(-0.0128079189208646,-0.0339125343235155,
-0.0136879621363756));
#23687=CARTESIAN_POINT('Ctrl Pts',(-0.0128284045828412,-0.0339114271713619,
-0.0136836455823627));
#23688=CARTESIAN_POINT('Ctrl Pts',(-0.0129251292450522,-0.0339061138457267,
-0.0136611999642417));
#23689=CARTESIAN_POINT('Ctrl Pts',(-0.0129999935089968,-0.033901738289074,
-0.0136376992090498));
#23690=CARTESIAN_POINT('Ctrl Pts',(-0.0131486557125619,-0.0338926037356183,
-0.0135782721193122));
#23691=CARTESIAN_POINT('Ctrl Pts',(-0.0132220365602471,-0.0338878509325728,
-0.0135419411007113));
#23692=CARTESIAN_POINT('Ctrl Pts',(-0.013329778709678,-0.0338807514782663,
-0.0134774809683645));
#23693=CARTESIAN_POINT('Ctrl Pts',(-0.01336639292423,-0.0338783171863884,
-0.0134534022032823));
#23694=CARTESIAN_POINT('Ctrl Pts',(-0.0134097757816292,-0.0338754515491987,
-0.0134221479554379));
#23695=CARTESIAN_POINT('Ctrl Pts',(-0.0134175630498147,-0.0338749379522715,
-0.0134164259097671));
#23696=CARTESIAN_POINT('Ctrl Pts',(-0.0134297243011914,-0.0338741378081026,
-0.0134073127223922));
#23697=CARTESIAN_POINT('Ctrl Pts',(-0.0134341345492815,-0.0338738480435428,
-0.0134039706523065));
#23698=CARTESIAN_POINT('Ctrl Pts',(-0.0134423585012808,-0.0338733086268853,
-0.0133976686402707));
#23699=CARTESIAN_POINT('Ctrl Pts',(-0.0134461762972185,-0.0338730586071664,
-0.0133947145249577));
#23700=CARTESIAN_POINT('Ctrl Pts',(-0.0134550759381883,-0.0338724766146771,
-0.0133877611906282));
#23701=CARTESIAN_POINT('Ctrl Pts',(-0.0134601465741876,-0.033872145642017,
-0.0133837478906604));
#23702=CARTESIAN_POINT('Ctrl Pts',(-0.0134766598247441,-0.0338710692824627,
-0.0133705083152189));
#23703=CARTESIAN_POINT('Ctrl Pts',(-0.0134879961645058,-0.0338703327408832,
-0.0133611501520987));
#23704=CARTESIAN_POINT('Ctrl Pts',(-0.0135150749094679,-0.0338685744948397,
-0.0133381381409284));
#23705=CARTESIAN_POINT('Ctrl Pts',(-0.0135306780669897,-0.0338675622911256,
-0.0133243244194481));
#23706=CARTESIAN_POINT('Ctrl Pts',(-0.0135921505298278,-0.0338635563248979,
-0.0132676397082127));
#23707=CARTESIAN_POINT('Ctrl Pts',(-0.0136356661331904,-0.0338606769791345,
-0.0132223014160844));
#23708=CARTESIAN_POINT('Ctrl Pts',(-0.013748768832314,-0.0338526845189636,
-0.0130890698215807));
#23709=CARTESIAN_POINT('Ctrl Pts',(-0.0138117230367726,-0.0338475881631072,
-0.0129960779024097));
#23710=CARTESIAN_POINT('Ctrl Pts',(-0.0138738817199854,-0.0338410609070436,
-0.0128785193145112));
#23711=CARTESIAN_POINT('Ctrl Pts',(-0.0138833227899311,-0.0338400172924914,
-0.012859745480525));
#23712=CARTESIAN_POINT('Ctrl Pts',(-0.0138969955099977,-0.0338384212191129,
-0.0128311146042731));
#23713=CARTESIAN_POINT('Ctrl Pts',(-0.0139015127879805,-0.0338378786935256,
-0.012821396272776));
#23714=CARTESIAN_POINT('Ctrl Pts',(-0.0139094463617619,-0.0338368976195423,
-0.0128038523704722));
#23715=CARTESIAN_POINT('Ctrl Pts',(-0.0139128996525081,-0.0338364603723145,
-0.0127960439541196));
#23716=CARTESIAN_POINT('Ctrl Pts',(-0.0139201344036976,-0.0338355219611277,
-0.0127793110037617));
#23717=CARTESIAN_POINT('Ctrl Pts',(-0.01392389692116,-0.033835020171144,
-0.0127703787218071));
#23718=CARTESIAN_POINT('Ctrl Pts',(-0.0139339156993355,-0.0338336454730962,
-0.0127459532225766));
#23719=CARTESIAN_POINT('Ctrl Pts',(-0.0139400047342329,-0.0338327669578527,
-0.0127303931909371));
#23720=CARTESIAN_POINT('Ctrl Pts',(-0.0139770304278779,-0.0338271390945943,
-0.0126310523803796));
#23721=CARTESIAN_POINT('Ctrl Pts',(-0.0140008924353247,-0.0338221541627022,
-0.012544828933463));
#23722=CARTESIAN_POINT('Ctrl Pts',(-0.0140332301460074,-0.0338120131433148,
-0.012370346730091));
#23723=CARTESIAN_POINT('Ctrl Pts',(-0.0140418372477321,-0.0338068806733685,
-0.0122824390536171));
#23724=CARTESIAN_POINT('Ctrl Pts',(-0.014042963335665,-0.0338015947159046,
-0.0121881359786935));
#23725=CARTESIAN_POINT('Ctrl Pts',(-0.0140430000000025,-0.0338012515219821,
-0.0121819945706754));
#23726=CARTESIAN_POINT('Ctrl Pts',(-0.014043,-0.0338009094848242,-0.0121758532859222));
#23727=CARTESIAN_POINT('Ctrl Pts',(-0.014043,-0.0339165738369763,-0.0121758532868962));
#23728=CARTESIAN_POINT('Ctrl Pts',(-0.0140429999999987,-0.0339168819553875,
-0.0121816378577507));
#23729=CARTESIAN_POINT('Ctrl Pts',(-0.0140429674712373,-0.033917191068193,
-0.0121874224595749));
#23730=CARTESIAN_POINT('Ctrl Pts',(-0.0140418661808551,-0.0339224402550407,
-0.0122853381697386));
#23731=CARTESIAN_POINT('Ctrl Pts',(-0.0140325801638651,-0.0339276333236809,
-0.0123771794184772));
#23732=CARTESIAN_POINT('Ctrl Pts',(-0.0140005714140538,-0.0339373450165894,
-0.0125433955946321));
#23733=CARTESIAN_POINT('Ctrl Pts',(-0.0139803192175374,-0.0339418181117581,
-0.0126179590145431));
#23734=CARTESIAN_POINT('Ctrl Pts',(-0.0139467928300904,-0.0339474463079475,
-0.0127126804242815));
#23735=CARTESIAN_POINT('Ctrl Pts',(-0.0139385137036548,-0.0339487375513169,
-0.0127344866971223));
#23736=CARTESIAN_POINT('Ctrl Pts',(-0.0139237275806061,-0.033950877777093,
-0.0127709202301066));
#23737=CARTESIAN_POINT('Ctrl Pts',(-0.0139174816935648,-0.0339517381395521,
-0.0127856488087573));
#23738=CARTESIAN_POINT('Ctrl Pts',(-0.0139082946000599,-0.0339529411465164,
-0.01280640880767));
#23739=CARTESIAN_POINT('Ctrl Pts',(-0.0139055415684377,-0.033953294179785,
-0.0128125218411621));
#23740=CARTESIAN_POINT('Ctrl Pts',(-0.0139007173125061,-0.0339538998557613,
-0.0128230501587434));
#23741=CARTESIAN_POINT('Ctrl Pts',(-0.0138986648578924,-0.0339541536188767,
-0.0128274738806194));
#23742=CARTESIAN_POINT('Ctrl Pts',(-0.0138942749599308,-0.0339546880892563,
-0.0128368192612915));
#23743=CARTESIAN_POINT('Ctrl Pts',(-0.0138919323914168,-0.0339549684811363,
-0.0128417383390659));
#23744=CARTESIAN_POINT('Ctrl Pts',(-0.0138854492956723,-0.0339557317070355,
-0.0128551682535083));
#23745=CARTESIAN_POINT('Ctrl Pts',(-0.0138812563780146,-0.0339562114047318,
-0.0128636536950639));
#23746=CARTESIAN_POINT('Ctrl Pts',(-0.0138596882441195,-0.0339586126064289,
-0.0129063095507802));
#23747=CARTESIAN_POINT('Ctrl Pts',(-0.013841120852835,-0.0339604683146547,
-0.0129398649008883));
#23748=CARTESIAN_POINT('Ctrl Pts',(-0.0137771292331624,-0.0339663367787027,
-0.0130459755702796));
#23749=CARTESIAN_POINT('Ctrl Pts',(-0.0137269155223952,-0.0339701867653888,
-0.0131154551184635));
#23750=CARTESIAN_POINT('Ctrl Pts',(-0.0136140448127748,-0.0339781479683432,
-0.0132470487015677));
#23751=CARTESIAN_POINT('Ctrl Pts',(-0.0135513143481563,-0.0339822520805361,
-0.0133086778101584));
#23752=CARTESIAN_POINT('Ctrl Pts',(-0.0134708167675302,-0.0339874264744039,
-0.0133752877386101));
#23753=CARTESIAN_POINT('Ctrl Pts',(-0.0134577714770716,-0.0339882619674114,
-0.0133857301278624));
#23754=CARTESIAN_POINT('Ctrl Pts',(-0.0134368746619523,-0.0339895968383089,
-0.0134019076566646));
#23755=CARTESIAN_POINT('Ctrl Pts',(-0.0134291339232105,-0.0339900905715831,
-0.01340778412786));
#23756=CARTESIAN_POINT('Ctrl Pts',(-0.0134144580375437,-0.0339910255129273,
-0.0134187084934615));
#23757=CARTESIAN_POINT('Ctrl Pts',(-0.0134075352859757,-0.0339914660640731,
-0.0134237724620258));
#23758=CARTESIAN_POINT('Ctrl Pts',(-0.0133918105008916,-0.0339924658665136,
-0.0134350750385165));
#23759=CARTESIAN_POINT('Ctrl Pts',(-0.0133829845956837,-0.033993026407715,
-0.0134412795332876));
#23760=CARTESIAN_POINT('Ctrl Pts',(-0.0133565991031334,-0.0339947006558988,
-0.0134594177420068));
#23761=CARTESIAN_POINT('Ctrl Pts',(-0.0133388579822405,-0.0339958244594125,
-0.0134710818222768));
#23762=CARTESIAN_POINT('Ctrl Pts',(-0.0132295442832735,-0.0340027394800111,
-0.0135397631460481));
#23763=CARTESIAN_POINT('Ctrl Pts',(-0.0131324528691232,-0.034008872529904,
-0.0135874063062154));
#23764=CARTESIAN_POINT('Ctrl Pts',(-0.012969652526776,-0.0340188463127523,
-0.0136471022663717));
#23765=CARTESIAN_POINT('Ctrl Pts',(-0.0129067222950847,-0.0340226252486277,
-0.0136657273388944));
#23766=CARTESIAN_POINT('Ctrl Pts',(-0.0128219608150001,-0.0340274779539682,
-0.0136850407778995));
#23767=CARTESIAN_POINT('Ctrl Pts',(-0.0128010282009019,-0.0340286573498574,
-0.0136893551027976));
#23768=CARTESIAN_POINT('Ctrl Pts',(-0.0127652697494482,-0.0340306323340263,
-0.0136959538398902));
#23769=CARTESIAN_POINT('Ctrl Pts',(-0.0127504881781399,-0.0340314372853405,
-0.0136984594200026));
#23770=CARTESIAN_POINT('Ctrl Pts',(-0.0127292147095755,-0.0340325770535712,
-0.0137017472240129));
#23771=CARTESIAN_POINT('Ctrl Pts',(-0.012722751113083,-0.034032920883753,
-0.0137027041751847));
#23772=CARTESIAN_POINT('Ctrl Pts',(-0.0127114763373589,-0.0340335161068744,
-0.0137043003125492));
#23773=CARTESIAN_POINT('Ctrl Pts',(-0.0127066679255429,-0.0340337685120117,
-0.0137049579014638));
#23774=CARTESIAN_POINT('Ctrl Pts',(-0.0126963667331323,-0.034034306096683,
-0.0137063171921365));
#23775=CARTESIAN_POINT('Ctrl Pts',(-0.0126908732145924,-0.03403459089536,
-0.0137070120235859));
#23776=CARTESIAN_POINT('Ctrl Pts',(-0.0126758286714037,-0.0340353659628247,
-0.0137088326616785));
#23777=CARTESIAN_POINT('Ctrl Pts',(-0.01266627052738,-0.034035853004221,
-0.0137098987900806));
#23778=CARTESIAN_POINT('Ctrl Pts',(-0.0126144778912107,-0.0340384660171013,
-0.0137151860436606));
#23779=CARTESIAN_POINT('Ctrl Pts',(-0.0125720897816036,-0.0340405108877644,
-0.0137177528066572));
#23780=CARTESIAN_POINT('Ctrl Pts',(-0.0124470069403706,-0.0340464052221194,
-0.0137201565645436));
#23781=CARTESIAN_POINT('Ctrl Pts',(-0.0123643700750698,-0.0340501257252152,
-0.0137151019765015));
#23782=CARTESIAN_POINT('Ctrl Pts',(-0.0122045639817979,-0.0340575430202072,
-0.013692352199915));
#23783=CARTESIAN_POINT('Ctrl Pts',(-0.01212756464644,-0.0340612226693292,
-0.0136753004213883));
#23784=CARTESIAN_POINT('Ctrl Pts',(-0.0120320943646422,-0.0340661217417427,
-0.0136463481344442));
#23785=CARTESIAN_POINT('Ctrl Pts',(-0.012012107731748,-0.0340671661508977,
-0.013639838212183));
#23786=CARTESIAN_POINT('Ctrl Pts',(-0.0119822453669242,-0.0340687577323076,
-0.013629432190861));
#23787=CARTESIAN_POINT('Ctrl Pts',(-0.0119722662719568,-0.0340692948845896,
-0.0136258390092792));
#23788=CARTESIAN_POINT('Ctrl Pts',(-0.0119542992869944,-0.0340702719232579,
-0.0136191595774042));
#23789=CARTESIAN_POINT('Ctrl Pts',(-0.0119462984888226,-0.0340707105931873,
-0.0136161091492304));
#23790=CARTESIAN_POINT('Ctrl Pts',(-0.0119291546369109,-0.0340716584595555,
-0.0136094088253486));
#23791=CARTESIAN_POINT('Ctrl Pts',(-0.0119200203267481,-0.0340721683596231,
-0.013605737716826));
#23792=CARTESIAN_POINT('Ctrl Pts',(-0.0118953508102537,-0.0340735589724287,
-0.0135955476849608));
#23793=CARTESIAN_POINT('Ctrl Pts',(-0.0118798865356904,-0.0340744453405359,
-0.0135888614565525));
#23794=CARTESIAN_POINT('Ctrl Pts',(-0.0117830585293732,-0.0340800898728459,
-0.0135451006373227));
#23795=CARTESIAN_POINT('Ctrl Pts',(-0.0117049480160294,-0.0340850837187335,
-0.0135012708639027));
#23796=CARTESIAN_POINT('Ctrl Pts',(-0.0115600854845306,-0.0340951046315003,
-0.0134025523475392));
#23797=CARTESIAN_POINT('Ctrl Pts',(-0.0114932556694099,-0.0341001028324449,
-0.013348327577726));
#23798=CARTESIAN_POINT('Ctrl Pts',(-0.0114135372186772,-0.0341063064698478,
-0.0132717789779167));
#23799=CARTESIAN_POINT('Ctrl Pts',(-0.0113961976756812,-0.0341076716363909,
-0.0132543128512691));
#23800=CARTESIAN_POINT('Ctrl Pts',(-0.0113678443336097,-0.0341099199323959,
-0.0132243519613536));
#23801=CARTESIAN_POINT('Ctrl Pts',(-0.0113566018868824,-0.034110815869021,
-0.0132120804445538));
#23802=CARTESIAN_POINT('Ctrl Pts',(-0.0113410418169122,-0.0341120592011703,
-0.0131945344416672));
#23803=CARTESIAN_POINT('Ctrl Pts',(-0.0113365575880127,-0.0341124179146666,
-0.0131894099565694));
#23804=CARTESIAN_POINT('Ctrl Pts',(-0.0113289097754156,-0.034113030125752,
-0.0131805525573911));
#23805=CARTESIAN_POINT('Ctrl Pts',(-0.0113257297810704,-0.0341132848106381,
-0.0131768340028047));
#23806=CARTESIAN_POINT('Ctrl Pts',(-0.0113190777067926,-0.0341138177497968,
-0.0131689800115793));
#23807=CARTESIAN_POINT('Ctrl Pts',(-0.0113156095912245,-0.0341140957258592,
-0.0131648414138303));
#23808=CARTESIAN_POINT('Ctrl Pts',(-0.0113062650182166,-0.0341148453117391,
-0.0131535706236289));
#23809=CARTESIAN_POINT('Ctrl Pts',(-0.0113004307062702,-0.0341153139708604,
-0.0131464036023412));
#23810=CARTESIAN_POINT('Ctrl Pts',(-0.0112726333011313,-0.0341175524042072,
-0.0131116229387454));
#23811=CARTESIAN_POINT('Ctrl Pts',(-0.0112515559114053,-0.0341192666688254,
-0.0130833121254884));
#23812=CARTESIAN_POINT('Ctrl Pts',(-0.0111815198250803,-0.034125117201908,
-0.0129821757173299));
#23813=CARTESIAN_POINT('Ctrl Pts',(-0.011137812967947,-0.0341290632318393,
-0.0129059176817033));
#23814=CARTESIAN_POINT('Ctrl Pts',(-0.0110665693752285,-0.0341368196305555,
-0.0127526783502748));
#23815=CARTESIAN_POINT('Ctrl Pts',(-0.011038191181993,-0.0341406071633157,
-0.0126764167811611));
#23816=CARTESIAN_POINT('Ctrl Pts',(-0.0110101121022922,-0.0341456409612672,
-0.0125777709467302));
#23817=CARTESIAN_POINT('Ctrl Pts',(-0.0110046999714092,-0.0341467001635747,
-0.0125571425758574));
#23818=CARTESIAN_POINT('Ctrl Pts',(-0.0109972248765825,-0.0341483098244435,
-0.0125260385130953));
#23819=CARTESIAN_POINT('Ctrl Pts',(-0.0109948401621653,-0.0341488499092875,
-0.0125156423676058));
#23820=CARTESIAN_POINT('Ctrl Pts',(-0.0109907515084667,-0.0341498260794714,
-0.0124969296714958));
#23821=CARTESIAN_POINT('Ctrl Pts',(-0.0109890080441714,-0.0341502608711658,
-0.0124886221465086));
#23822=CARTESIAN_POINT('Ctrl Pts',(-0.0109854049022679,-0.0341512010374324,
-0.0124707197057026));
#23823=CARTESIAN_POINT('Ctrl Pts',(-0.0109835676686091,-0.0341517071119637,
-0.0124611206937532));
#23824=CARTESIAN_POINT('Ctrl Pts',(-0.010978868711545,-0.034153077070768,
-0.0124352407394915));
#23825=CARTESIAN_POINT('Ctrl Pts',(-0.0109761772794249,-0.0341539463330875,
-0.0124189305067325));
#23826=CARTESIAN_POINT('Ctrl Pts',(-0.0109625220912687,-0.0341588796863046,
-0.0123270084003832));
#23827=CARTESIAN_POINT('Ctrl Pts',(-0.0109569254141913,-0.0341631120817109,
-0.012250716307284));
#23828=CARTESIAN_POINT('Ctrl Pts',(-0.0109570599964251,-0.0341708617876835,
-0.0121142608933694));
#23829=CARTESIAN_POINT('Ctrl Pts',(-0.0109606271248052,-0.0341743301422374,
-0.0120542462511054));
#23830=CARTESIAN_POINT('Ctrl Pts',(-0.0109762855719327,-0.0341819839972782,
-0.0119218736270641));
#23831=CARTESIAN_POINT('Ctrl Pts',(-0.0109900545224996,-0.0341861514704352,
-0.0118498503352225));
#23832=CARTESIAN_POINT('Ctrl Pts',(-0.0110115743999154,-0.0341906470959918,
-0.0117689782013035));
#23833=CARTESIAN_POINT('Ctrl Pts',(-0.0110143628699955,-0.0341912032825339,
-0.0117589115261202));
#23834=CARTESIAN_POINT('Ctrl Pts',(-0.0110188371096052,-0.0341920555827564,
-0.0117433741014541));
#23835=CARTESIAN_POINT('Ctrl Pts',(-0.0110204514078073,-0.034192355583777,
-0.011737883288903));
#23836=CARTESIAN_POINT('Ctrl Pts',(-0.0110234824791191,-0.0341929051354327,
-0.0117277815556296));
#23837=CARTESIAN_POINT('Ctrl Pts',(-0.0110248903332141,-0.0341931551716302,
-0.0117231682556579));
#23838=CARTESIAN_POINT('Ctrl Pts',(-0.0110281707749667,-0.0341937260555698,
-0.0117125966219053));
#23839=CARTESIAN_POINT('Ctrl Pts',(-0.011030057923812,-0.034194046052353,
-0.0117066429922562));
#23840=CARTESIAN_POINT('Ctrl Pts',(-0.0110361036969079,-0.0341950457294547,
-0.0116879641251366));
#23841=CARTESIAN_POINT('Ctrl Pts',(-0.0110403919102006,-0.0341957182474183,
-0.0116752811468108));
#23842=CARTESIAN_POINT('Ctrl Pts',(-0.0110637921214595,-0.0341992111765697,
-0.0116089306680731));
#23843=CARTESIAN_POINT('Ctrl Pts',(-0.0110857018862287,-0.034201895485191,
-0.0115562919490737));
#23844=CARTESIAN_POINT('Ctrl Pts',(-0.0111536770251621,-0.0342091294323706,
-0.0114155001548916));
#23845=CARTESIAN_POINT('Ctrl Pts',(-0.0112054208378183,-0.0342135776605898,
-0.0113304022107571));
#23846=CARTESIAN_POINT('Ctrl Pts',(-0.0112959237898262,-0.0342206841362531,
-0.0112095652720746));
#23847=CARTESIAN_POINT('Ctrl Pts',(-0.0113289095904308,-0.0342231669787839,
-0.0111698420270301));
#23848=CARTESIAN_POINT('Ctrl Pts',(-0.0113741618885419,-0.0342264896218121,
-0.0111205944995771));
#23849=CARTESIAN_POINT('Ctrl Pts',(-0.011384668643336,-0.0342272556095621,
-0.0111094956990838));
#23850=CARTESIAN_POINT('Ctrl Pts',(-0.0114019093675456,-0.0342285048183376,
-0.0110918170591769));
#23851=CARTESIAN_POINT('Ctrl Pts',(-0.0114085418524266,-0.0342289836011937,
-0.0110851394440199));
#23852=CARTESIAN_POINT('Ctrl Pts',(-0.0114213816155277,-0.034229907293543,
-0.0110724467050304));
#23853=CARTESIAN_POINT('Ctrl Pts',(-0.011427579173089,-0.034230351760627,
-0.0110664222299238));
#23854=CARTESIAN_POINT('Ctrl Pts',(-0.0114420327825883,-0.0342313853077307,
-0.0110526065523283));
#23855=CARTESIAN_POINT('Ctrl Pts',(-0.0114503247823202,-0.0342319760226555,
-0.0110448538227376));
#23856=CARTESIAN_POINT('Ctrl Pts',(-0.01147716705339,-0.0342338815517711,
-0.011020306704095));
#23857=CARTESIAN_POINT('Ctrl Pts',(-0.0114960399330842,-0.0342352113660145,
-0.0110038723882454));
#23858=CARTESIAN_POINT('Ctrl Pts',(-0.0115867473111157,-0.0342415588360713,
-0.0109286845707943));
#23859=CARTESIAN_POINT('Ctrl Pts',(-0.0116633789458999,-0.0342468118296892,
-0.0108760373479941));
#23860=CARTESIAN_POINT('Ctrl Pts',(-0.0118302512465144,-0.0342578068989465,
-0.0107822921191419));
#23861=CARTESIAN_POINT('Ctrl Pts',(-0.0119206760742138,-0.0342635322458617,
-0.0107423393303115));
#23862=CARTESIAN_POINT('Ctrl Pts',(-0.0120259792068886,-0.0342695394874135,
-0.010707417147708));
#23863=CARTESIAN_POINT('Ctrl Pts',(-0.012037704699816,-0.0342701993351495,
-0.0107036836360494));
#23864=CARTESIAN_POINT('Ctrl Pts',(-0.0120553421645006,-0.0342711770218776,
-0.0106982992081205));
#23865=CARTESIAN_POINT('Ctrl Pts',(-0.0120612211157337,-0.0342715004505767,
-0.0106965427246439));
#23866=CARTESIAN_POINT('Ctrl Pts',(-0.0120718459873247,-0.0342720803496296,
-0.0106934371903639));
#23867=CARTESIAN_POINT('Ctrl Pts',(-0.0120765881985979,-0.0342723375211186,
-0.010692075746158));
#23868=CARTESIAN_POINT('Ctrl Pts',(-0.0120863423381146,-0.0342728629797478,
-0.0106893259966914));
#23869=CARTESIAN_POINT('Ctrl Pts',(-0.0120913548806263,-0.0342731311213061,
-0.0106879402471858));
#23870=CARTESIAN_POINT('Ctrl Pts',(-0.0121044195150341,-0.0342738253265849,
-0.0106843994462253));
#23871=CARTESIAN_POINT('Ctrl Pts',(-0.0121124823328493,-0.0342742491457788,
-0.0106822842250389));
#23872=CARTESIAN_POINT('Ctrl Pts',(-0.0121484985631459,-0.0342761234157088,
-0.010673146921336));
#23873=CARTESIAN_POINT('Ctrl Pts',(-0.0121766298190491,-0.0342775367744566,
-0.0106668431475499));
#23874=CARTESIAN_POINT('Ctrl Pts',(-0.0122593065354476,-0.0342815862738689,
-0.0106507350859149));
#23875=CARTESIAN_POINT('Ctrl Pts',(-0.0123142248016605,-0.03428414596265,
-0.0106430756999138));
#23876=CARTESIAN_POINT('Ctrl Pts',(-0.0124925214292395,-0.0342923481943397,
-0.0106279347851452));
#23877=CARTESIAN_POINT('Ctrl Pts',(-0.0126164021547135,-0.0342979222621967,
-0.0106323002044008));
#23878=CARTESIAN_POINT('Ctrl Pts',(-0.0127564829825984,-0.034304894310201,
-0.0106542097215534));
#23879=CARTESIAN_POINT('Ctrl Pts',(-0.0127744778656844,-0.0343058018431939,
-0.010657352537306));
#23880=CARTESIAN_POINT('Ctrl Pts',(-0.0128032320490911,-0.0343072729945317,
-0.0106629022783815));
#23881=CARTESIAN_POINT('Ctrl Pts',(-0.012814028966042,-0.0343078301740489,
-0.0106651063755651));
#23882=CARTESIAN_POINT('Ctrl Pts',(-0.0128332315208545,-0.0343088300182377,
-0.010669241153507));
#23883=CARTESIAN_POINT('Ctrl Pts',(-0.0128416463865858,-0.0343092712258645,
-0.0106711270295678));
#23884=CARTESIAN_POINT('Ctrl Pts',(-0.0128592788420057,-0.0343102023283021,
-0.0106752342123483));
#23885=CARTESIAN_POINT('Ctrl Pts',(-0.0128684926289635,-0.0343106926803488,
-0.0106774701348917));
#23886=CARTESIAN_POINT('Ctrl Pts',(-0.0128928155464958,-0.0343119974403325,
-0.0106836105223035));
#23887=CARTESIAN_POINT('Ctrl Pts',(-0.0129078867897223,-0.0343128164998596,
-0.0106876594606027));
#23888=CARTESIAN_POINT('Ctrl Pts',(-0.0129841371338026,-0.0343170155297221,
-0.0107093896420596));
#23889=CARTESIAN_POINT('Ctrl Pts',(-0.0130442347208517,-0.0343205102854798,
-0.0107306157847064));
#23890=CARTESIAN_POINT('Ctrl Pts',(-0.0131637612941513,-0.0343278159899963,
-0.0107813464492047));
#23891=CARTESIAN_POINT('Ctrl Pts',(-0.013222949450712,-0.0343316265907891,
-0.0108110926124364));
#23892=CARTESIAN_POINT('Ctrl Pts',(-0.0132999518711651,-0.0343367588370512,
-0.0108562099697055));
#23893=CARTESIAN_POINT('Ctrl Pts',(-0.0133195975824376,-0.034338084110897,
-0.0108683207611632));
#23894=CARTESIAN_POINT('Ctrl Pts',(-0.0133886065513542,-0.034342781360564,
-0.010913028651199));
#23895=CARTESIAN_POINT('Ctrl Pts',(-0.013436362987608,-0.0343461120321917,
-0.0109480205363585));
#23896=CARTESIAN_POINT('Ctrl Pts',(-0.0134899171378269,-0.0343498398806495,
-0.0109922070016261));
#23897=CARTESIAN_POINT('Ctrl Pts',(-0.0134977733931625,-0.034350386505033,
-0.0109988219638662));
#23898=CARTESIAN_POINT('Ctrl Pts',(-0.0135098744994844,-0.0343512272905925,
-0.0110092193233459));
#23899=CARTESIAN_POINT('Ctrl Pts',(-0.0135141653446655,-0.034351525182294,
-0.011012947458667));
#23900=CARTESIAN_POINT('Ctrl Pts',(-0.0135220624227746,-0.034352072831153,
-0.0110198858508781));
#23901=CARTESIAN_POINT('Ctrl Pts',(-0.0135256742153983,-0.034352323047202,
-0.0110230893415534));
#23902=CARTESIAN_POINT('Ctrl Pts',(-0.013533964311583,-0.0343528968425861,
-0.0110305120764382));
#23903=CARTESIAN_POINT('Ctrl Pts',(-0.0135386318644841,-0.0343532195365757,
-0.0110347430648929));
#23904=CARTESIAN_POINT('Ctrl Pts',(-0.013553352486738,-0.0343542365682551,
-0.0110482519930885));
#23905=CARTESIAN_POINT('Ctrl Pts',(-0.0135633083998079,-0.034354923384867,
-0.0110576353250008));
#23906=CARTESIAN_POINT('Ctrl Pts',(-0.013616011049628,-0.0343585619753758,
-0.0111086473952346));
#23907=CARTESIAN_POINT('Ctrl Pts',(-0.0136564443444972,-0.034361364809422,
-0.0111526002560622));
#23908=CARTESIAN_POINT('Ctrl Pts',(-0.0137587137663943,-0.0343688224020463,
-0.0112776006168463));
#23909=CARTESIAN_POINT('Ctrl Pts',(-0.0138152329854705,-0.0343733834884902,
-0.0113626002734257));
#23910=CARTESIAN_POINT('Ctrl Pts',(-0.0138850475166336,-0.0343804288090042,
-0.0114941560716249));
#23911=CARTESIAN_POINT('Ctrl Pts',(-0.0139052095747807,-0.0343827046221997,
-0.0115367498061741));
#23912=CARTESIAN_POINT('Ctrl Pts',(-0.0139290773392635,-0.0343857801539392,
-0.0115937846297097));
#23913=CARTESIAN_POINT('Ctrl Pts',(-0.0139345685567039,-0.0343865191528315,
-0.0116074528995361));
#23914=CARTESIAN_POINT('Ctrl Pts',(-0.0139432035754576,-0.0343877351642379,
-0.0116298690416399));
#23915=CARTESIAN_POINT('Ctrl Pts',(-0.0139464655601267,-0.0343882081750974,
-0.0116385705543616));
#23916=CARTESIAN_POINT('Ctrl Pts',(-0.0139526236571518,-0.0343891283853403,
-0.011655460227402));
#23917=CARTESIAN_POINT('Ctrl Pts',(-0.0139555296322574,-0.0343895752324933,
-0.0116636444318603));
#23918=CARTESIAN_POINT('Ctrl Pts',(-0.0139621662630897,-0.0343906260883323,
-0.0116828480551826));
#23919=CARTESIAN_POINT('Ctrl Pts',(-0.013965841657881,-0.0343912319070737,
-0.0116938858985679));
#23920=CARTESIAN_POINT('Ctrl Pts',(-0.0139775273935811,-0.0343932396398711,
-0.0117303507889806));
#23921=CARTESIAN_POINT('Ctrl Pts',(-0.013985003317691,-0.0343946588963027,
-0.011755942937559));
#23922=CARTESIAN_POINT('Ctrl Pts',(-0.0140013808732151,-0.0343981218848936,
-0.0118179319184796));
#23923=CARTESIAN_POINT('Ctrl Pts',(-0.0140096268551409,-0.0344001846568486,
-0.0118544832622702));
#23924=CARTESIAN_POINT('Ctrl Pts',(-0.0140341595026928,-0.0344076234534603,
-0.0119852290946746));
#23925=CARTESIAN_POINT('Ctrl Pts',(-0.014043,-0.0344131679976405,-0.0120804906866184));
#23926=CARTESIAN_POINT('Ctrl Pts',(-0.014043,-0.0344186209509151,-0.012175853286558));
#23927=CARTESIAN_POINT('Origin',(-0.0125,-0.0375520664398416,-0.0121758532865581));
#23928=CARTESIAN_POINT('',(-0.014043,-0.0349189332996453,-0.0121758532870635));
#23929=CARTESIAN_POINT('',(-0.014043,-0.0348029487958341,-0.0121758532497851));
#23930=CARTESIAN_POINT('',(-0.014043,-0.0375520664398416,-0.012175853286558));
#23931=CARTESIAN_POINT('Ctrl Pts',(-0.014043,-0.0348029487975611,-0.0121758532497038));
#23932=CARTESIAN_POINT('Ctrl Pts',(-0.0140429999991421,-0.0348012580629849,
-0.0121399335435184));
#23933=CARTESIAN_POINT('Ctrl Pts',(-0.014041745734116,-0.0347995408373542,
-0.0121040125839542));
#23934=CARTESIAN_POINT('Ctrl Pts',(-0.01403751176791,-0.0347965809558476,
-0.012043499716227));
#23935=CARTESIAN_POINT('Ctrl Pts',(-0.0140351945091131,-0.0347953584651334,
-0.0120188894748785));
#23936=CARTESIAN_POINT('Ctrl Pts',(-0.014030961674456,-0.0347935516956769,
-0.011983155759407));
#23937=CARTESIAN_POINT('Ctrl Pts',(-0.0140295135721886,-0.0347929821110866,
-0.0119719802638061));
#23938=CARTESIAN_POINT('Ctrl Pts',(-0.0140267445567563,-0.034791970918662,
-0.0119523045466312));
#23939=CARTESIAN_POINT('Ctrl Pts',(-0.0140254747189967,-0.0347915309495704,
-0.0119437975638588));
#23940=CARTESIAN_POINT('Ctrl Pts',(-0.0140226705680918,-0.0347906060983903,
-0.0119260304715128));
#23941=CARTESIAN_POINT('Ctrl Pts',(-0.0140211227541889,-0.0347901208019042,
-0.0119167728756742));
#23942=CARTESIAN_POINT('Ctrl Pts',(-0.0140168326182398,-0.0347888380831219,
-0.0118924782121651));
#23943=CARTESIAN_POINT('Ctrl Pts',(-0.0140139512013873,-0.0347880362541413,
-0.0118774670241026));
#23944=CARTESIAN_POINT('Ctrl Pts',(-0.0140001148026942,-0.0347844303922262,
-0.0118107538762324));
#23945=CARTESIAN_POINT('Ctrl Pts',(-0.0139867318031865,-0.0347815496634318,
-0.0117595965603673));
#23946=CARTESIAN_POINT('Ctrl Pts',(-0.0139408670432501,-0.034773090139021,
-0.0116150351352174));
#23947=CARTESIAN_POINT('Ctrl Pts',(-0.0139020029980949,-0.0347673494112467,
-0.0115239332417468));
#23948=CARTESIAN_POINT('Ctrl Pts',(-0.0138277053165867,-0.0347584755960986,
-0.0113876734085803));
#23949=CARTESIAN_POINT('Ctrl Pts',(-0.013798013594988,-0.0347552923452348,
-0.0113396770781155));
#23950=CARTESIAN_POINT('Ctrl Pts',(-0.0137581520650528,-0.0347515213179414,
-0.0112825004569037));
#23951=CARTESIAN_POINT('Ctrl Pts',(-0.0137504046323687,-0.0347508092782744,
-0.0112716883814002));
#23952=CARTESIAN_POINT('Ctrl Pts',(-0.0137388340669561,-0.0347497776175363,
-0.0112559740766092));
#23953=CARTESIAN_POINT('Ctrl Pts',(-0.0137351197652447,-0.0347494510805446,
-0.0112509928784568));
#23954=CARTESIAN_POINT('Ctrl Pts',(-0.0137284816915407,-0.0347488758708944,
-0.0112422019635401));
#23955=CARTESIAN_POINT('Ctrl Pts',(-0.0137255701010103,-0.0347486263799291,
-0.011238383293038));
#23956=CARTESIAN_POINT('Ctrl Pts',(-0.0137191637439839,-0.034748083555758,
-0.0112300619513505));
#23957=CARTESIAN_POINT('Ctrl Pts',(-0.0137156618268175,-0.0347477907300632,
-0.0112255650096444));
#23958=CARTESIAN_POINT('Ctrl Pts',(-0.0137056972964128,-0.0347469681255311,
-0.011212914413566));
#23959=CARTESIAN_POINT('Ctrl Pts',(-0.013699176909141,-0.034746442277628,
-0.0112048064311313));
#23960=CARTESIAN_POINT('Ctrl Pts',(-0.013648176290168,-0.0347424187219958,
-0.0111426853287046));
#23961=CARTESIAN_POINT('Ctrl Pts',(-0.0136001458317616,-0.0347391448638842,
-0.0110916826586344));
#23962=CARTESIAN_POINT('Ctrl Pts',(-0.0134785476955321,-0.0347315126789831,
-0.0109789943837103));
#23963=CARTESIAN_POINT('Ctrl Pts',(-0.01340237143499,-0.0347272062335571,
-0.0109205635125968));
#23964=CARTESIAN_POINT('Ctrl Pts',(-0.0132939182019669,-0.0347211501204998,
-0.010852378079092));
#23965=CARTESIAN_POINT('Ctrl Pts',(-0.0132660355449561,-0.0347196007418359,
-0.0108360465380061));
#23966=CARTESIAN_POINT('Ctrl Pts',(-0.013216707639586,-0.0347168564646891,
-0.0108091973977016));
#23967=CARTESIAN_POINT('Ctrl Pts',(-0.0131954925442745,-0.0347156752600287,
-0.0107982799842638));
#23968=CARTESIAN_POINT('Ctrl Pts',(-0.0131640355302172,-0.0347139184946066,
-0.0107830039234968));
#23969=CARTESIAN_POINT('Ctrl Pts',(-0.0131539855139859,-0.0347133564706586,
-0.0107782569669066));
#23970=CARTESIAN_POINT('Ctrl Pts',(-0.013136087158528,-0.0347123538342471,
-0.0107700383061924));
#23971=CARTESIAN_POINT('Ctrl Pts',(-0.0131282594335889,-0.0347119147657585,
-0.0107665226963752));
#23972=CARTESIAN_POINT('Ctrl Pts',(-0.0131117400723384,-0.0347109868114844,
-0.0107592684497054));
#23973=CARTESIAN_POINT('Ctrl Pts',(-0.0131030425782815,-0.0347104974573156,
-0.0107555441091177));
#23974=CARTESIAN_POINT('Ctrl Pts',(-0.013079883891889,-0.0347091921786198,
-0.0107458784308514));
#23975=CARTESIAN_POINT('Ctrl Pts',(-0.0130653659692476,-0.0347083715638186,
-0.0107400765934362));
#23976=CARTESIAN_POINT('Ctrl Pts',(-0.0129971769284857,-0.0347045052814919,
-0.0107140205999448));
#23977=CARTESIAN_POINT('Ctrl Pts',(-0.012942496253295,-0.0347013682441913,
-0.0106965508671733));
#23978=CARTESIAN_POINT('Ctrl Pts',(-0.0127936343780978,-0.0346927557600194,
-0.0106579847228088));
#23979=CARTESIAN_POINT('Ctrl Pts',(-0.0126982363183118,-0.0346871497843407,
-0.0106426063059972));
#23980=CARTESIAN_POINT('Ctrl Pts',(-0.0125481484477505,-0.0346785606464023,
-0.010632659369271));
#23981=CARTESIAN_POINT('Ctrl Pts',(-0.0124941049071916,-0.0346755183130572,
-0.0106319193779547));
#23982=CARTESIAN_POINT('Ctrl Pts',(-0.0124271083915702,-0.0346718931775235,
-0.0106345208644435));
#23983=CARTESIAN_POINT('Ctrl Pts',(-0.0124140931256991,-0.0346711958684321,
-0.0106351914635125));
#23984=CARTESIAN_POINT('Ctrl Pts',(-0.0123949373131373,-0.0346701813572464,
-0.0106364219588273));
#23985=CARTESIAN_POINT('Ctrl Pts',(-0.0123887894361534,-0.03466985755058,
-0.0106368538732956));
#23986=CARTESIAN_POINT('Ctrl Pts',(-0.0123783161241449,-0.0346693091732236,
-0.0106376527548753));
#23987=CARTESIAN_POINT('Ctrl Pts',(-0.0123739894365506,-0.0346690835831548,
-0.0106380011542992));
#23988=CARTESIAN_POINT('Ctrl Pts',(-0.0123641395461644,-0.0346685722226116,
-0.0106388361502355));
#23989=CARTESIAN_POINT('Ctrl Pts',(-0.0123586174510793,-0.0346682870993795,
-0.0106393342606434));
#23990=CARTESIAN_POINT('Ctrl Pts',(-0.0123434305523197,-0.0346675069527838,
-0.01064078673296));
#23991=CARTESIAN_POINT('Ctrl Pts',(-0.0123337717363325,-0.0346670152453671,
-0.0106418026063482));
#23992=CARTESIAN_POINT('Ctrl Pts',(-0.0122796699143721,-0.0346642829411992,
-0.0106480097948837));
#23993=CARTESIAN_POINT('Ctrl Pts',(-0.0122354561737832,-0.0346621327194156,
-0.0106550415726527));
#23994=CARTESIAN_POINT('Ctrl Pts',(-0.0121121622172345,-0.0346562196910767,
-0.0106801912180253));
#23995=CARTESIAN_POINT('Ctrl Pts',(-0.0120341153318108,-0.034652568891892,
-0.0107026338102876));
#23996=CARTESIAN_POINT('Ctrl Pts',(-0.0118851068061876,-0.0346452533972879,
-0.0107585149605496));
#23997=CARTESIAN_POINT('Ctrl Pts',(-0.0118142125622679,-0.0346416038930214,
-0.0107914271992862));
#23998=CARTESIAN_POINT('Ctrl Pts',(-0.0117278848647284,-0.034636744087275,
-0.0108397680112178));
#23999=CARTESIAN_POINT('Ctrl Pts',(-0.0117098625537106,-0.0346357055856312,
-0.0108503464368677));
#24000=CARTESIAN_POINT('Ctrl Pts',(-0.011683068762984,-0.0346341225896791,
-0.010866814035145));
#24001=CARTESIAN_POINT('Ctrl Pts',(-0.0116741334895471,-0.0346335879927251,
-0.0108724328219833));
#24002=CARTESIAN_POINT('Ctrl Pts',(-0.0116580867218919,-0.0346326154279782,
-0.0108827547938788));
#24003=CARTESIAN_POINT('Ctrl Pts',(-0.0116509551818055,-0.0346321786627748,
-0.0108874261165389));
#24004=CARTESIAN_POINT('Ctrl Pts',(-0.0116357054653001,-0.0346312347449588,
-0.0108975966232083));
#24005=CARTESIAN_POINT('Ctrl Pts',(-0.0116276002921786,-0.0346307268925758,
-0.0109031145529893));
#24006=CARTESIAN_POINT('Ctrl Pts',(-0.0116057627621163,-0.0346293415456556,
-0.010918287957471));
#24007=CARTESIAN_POINT('Ctrl Pts',(-0.0115921347630105,-0.0346284584335719,
-0.0109280906986019));
#24008=CARTESIAN_POINT('Ctrl Pts',(-0.0115071365015549,-0.0346228303094849,
-0.0109913604379074));
#24009=CARTESIAN_POINT('Ctrl Pts',(-0.0114403638143025,-0.0346178508380652,
-0.0110507006533252));
#24010=CARTESIAN_POINT('Ctrl Pts',(-0.0113198272228724,-0.0346078258708291,
-0.0111781163137375));
#24011=CARTESIAN_POINT('Ctrl Pts',(-0.0112659160124668,-0.0346028078556228,
-0.0112456254768164));
#24012=CARTESIAN_POINT('Ctrl Pts',(-0.0112042216707944,-0.0345965842034982,
-0.0113377517207346));
#24013=CARTESIAN_POINT('Ctrl Pts',(-0.0111910073972785,-0.0345952176661557,
-0.0113585441729841));
#24014=CARTESIAN_POINT('Ctrl Pts',(-0.0111697097040237,-0.0345929681388785,
-0.0113938982932357));
#24015=CARTESIAN_POINT('Ctrl Pts',(-0.0111613541210226,-0.034592072289641,
-0.0114082901699963));
#24016=CARTESIAN_POINT('Ctrl Pts',(-0.0111499180136471,-0.0345908299782384,
-0.0114287430142325));
#24017=CARTESIAN_POINT('Ctrl Pts',(-0.0111466424789714,-0.0345904721865331,
-0.0114346930120205));
#24018=CARTESIAN_POINT('Ctrl Pts',(-0.0111410841852982,-0.0345898618858341,
-0.0114449493529299));
#24019=CARTESIAN_POINT('Ctrl Pts',(-0.0111387823650064,-0.0345896081919407,
-0.0114492452049711));
#24020=CARTESIAN_POINT('Ctrl Pts',(-0.0111339875844909,-0.0345890778025186,
-0.0114582963856109));
#24021=CARTESIAN_POINT('Ctrl Pts',(-0.0111314990500196,-0.0345888013776382,
-0.0114630538918928));
#24022=CARTESIAN_POINT('Ctrl Pts',(-0.0111248289077022,-0.0345880570649138,
-0.0114759693659859));
#24023=CARTESIAN_POINT('Ctrl Pts',(-0.0111206950246796,-0.034587592075028,
-0.0114841518855002));
#24024=CARTESIAN_POINT('Ctrl Pts',(-0.0111012792213883,-0.0345853878878853,
-0.011523449401265));
#24025=CARTESIAN_POINT('Ctrl Pts',(-0.0110869748538561,-0.0345837022660812,
-0.0115550385811138));
#24026=CARTESIAN_POINT('Ctrl Pts',(-0.01104008192827,-0.0345778522521503,
-0.0116686336922188));
#24027=CARTESIAN_POINT('Ctrl Pts',(-0.0110134721977819,-0.0345738843268449,
-0.0117529238063195));
#24028=CARTESIAN_POINT('Ctrl Pts',(-0.0109747091602888,-0.0345657346855752,
-0.0119262162696693));
#24029=CARTESIAN_POINT('Ctrl Pts',(-0.0109628173557519,-0.0345615629243733,
-0.0120149246320466));
#24030=CARTESIAN_POINT('Ctrl Pts',(-0.0109578902189873,-0.0345563116029354,
-0.0121208475924382));
#24031=CARTESIAN_POINT('Ctrl Pts',(-0.0109573850016952,-0.0345554761140637,
-0.0121375499888535));
#24032=CARTESIAN_POINT('Ctrl Pts',(-0.0109570154826123,-0.0345541425670264,
-0.0121639484849535));
#24033=CARTESIAN_POINT('Ctrl Pts',(-0.0109569711456687,-0.0345536501686099,
-0.01217364098189));
#24034=CARTESIAN_POINT('Ctrl Pts',(-0.0109570595178176,-0.0345527186021928,
-0.0121918709027938));
#24035=CARTESIAN_POINT('Ctrl Pts',(-0.0109571717679699,-0.0345522800959843,
-0.0122004080850345));
#24036=CARTESIAN_POINT('Ctrl Pts',(-0.0109575846833157,-0.0345512861226654,
-0.0122196577761233));
#24037=CARTESIAN_POINT('Ctrl Pts',(-0.0109579261096864,-0.0345507293921081,
-0.0122303688938816));
#24038=CARTESIAN_POINT('Ctrl Pts',(-0.0109592672037795,-0.0345490706659133,
-0.0122620676283123));
#24039=CARTESIAN_POINT('Ctrl Pts',(-0.0109605839821037,-0.0345479588055577,
-0.0122830387664267));
#24040=CARTESIAN_POINT('Ctrl Pts',(-0.0109716291063822,-0.0345408367033072,
-0.0124155976015113));
#24041=CARTESIAN_POINT('Ctrl Pts',(-0.010993054851541,-0.034534454179706,
-0.0125258591424952));
#24042=CARTESIAN_POINT('Ctrl Pts',(-0.0110448051221494,-0.0345244015989573,
-0.0126927638524296));
#24043=CARTESIAN_POINT('Ctrl Pts',(-0.0110670350297019,-0.0345207895977096,
-0.0127515274245164));
#24044=CARTESIAN_POINT('Ctrl Pts',(-0.0111013291370773,-0.0345161274986028,
-0.0128277757172094));
#24045=CARTESIAN_POINT('Ctrl Pts',(-0.0111102591466179,-0.0345149787699522,
-0.0128466017260878));
#24046=CARTESIAN_POINT('Ctrl Pts',(-0.0111261345057325,-0.0345130501332825,
-0.0128783905533677));
#24047=CARTESIAN_POINT('Ctrl Pts',(-0.0111328887549882,-0.034512261366232,
-0.0128914452669116));
#24048=CARTESIAN_POINT('Ctrl Pts',(-0.0111428818634372,-0.0345111410406802,
-0.0129101020017497));
#24049=CARTESIAN_POINT('Ctrl Pts',(-0.0111459708455386,-0.0345108008422562,
-0.012915782921158));
#24050=CARTESIAN_POINT('Ctrl Pts',(-0.0111514280551518,-0.0345102105969556,
-0.0129256706053631));
#24051=CARTESIAN_POINT('Ctrl Pts',(-0.0111537804470121,-0.0345099595712933,
-0.0129298859246751));
#24052=CARTESIAN_POINT('Ctrl Pts',(-0.0111588718750154,-0.0345094235687743,
-0.0129389096228454));
#24053=CARTESIAN_POINT('Ctrl Pts',(-0.0111616170232771,-0.0345091389843756,
-0.0129437143608758));
#24054=CARTESIAN_POINT('Ctrl Pts',(-0.0111692270630409,-0.0345083617834544,
-0.0129568691490597));
#24055=CARTESIAN_POINT('Ctrl Pts',(-0.0111741447184453,-0.0345078724419543,
-0.0129651885566677));
#24056=CARTESIAN_POINT('Ctrl Pts',(-0.0112017872861205,-0.0345051889368049,
-0.013010965363179));
#24057=CARTESIAN_POINT('Ctrl Pts',(-0.0112260230999787,-0.0345030813511353,
-0.013047490756475));
#24058=CARTESIAN_POINT('Ctrl Pts',(-0.0112998359588708,-0.0344971748629624,
-0.0131490629118939));
#24059=CARTESIAN_POINT('Ctrl Pts',(-0.0113530696020962,-0.0344934948411737,
-0.0132112674077798));
#24060=CARTESIAN_POINT('Ctrl Pts',(-0.0114664916952165,-0.0344861362843386,
-0.0133242648397486));
#24061=CARTESIAN_POINT('Ctrl Pts',(-0.0115261285457597,-0.0344824737558901,
-0.0133752536876955));
#24062=CARTESIAN_POINT('Ctrl Pts',(-0.0116062743455237,-0.0344775977020852,
-0.013433844410628));
#24063=CARTESIAN_POINT('Ctrl Pts',(-0.0116234227475888,-0.0344765573886726,
-0.0134458530824239));
#24064=CARTESIAN_POINT('Ctrl Pts',(-0.0116495830095334,-0.0344749721775005,
-0.0134633902784696));
#24065=CARTESIAN_POINT('Ctrl Pts',(-0.0116584163806167,-0.0344744372198324,
-0.0134691813839847));
#24066=CARTESIAN_POINT('Ctrl Pts',(-0.0116744860615738,-0.0344734642718251,
-0.0134794822313509));
#24067=CARTESIAN_POINT('Ctrl Pts',(-0.0116817016621884,-0.0344730274885644,
-0.0134840235792547));
#24068=CARTESIAN_POINT('Ctrl Pts',(-0.0116972911702999,-0.0344720838399689,
-0.0134936558395733));
#24069=CARTESIAN_POINT('Ctrl Pts',(-0.0117056766547608,-0.0344715762783654,
-0.0134987272228245));
#24070=CARTESIAN_POINT('Ctrl Pts',(-0.011728535198581,-0.0344701925037559,
-0.0135122559372665));
#24071=CARTESIAN_POINT('Ctrl Pts',(-0.0117430984048055,-0.0344693106944539,
-0.0135205576889706));
#24072=CARTESIAN_POINT('Ctrl Pts',(-0.0118355791730597,-0.034463708092659,
-0.013571297998802));
#24073=CARTESIAN_POINT('Ctrl Pts',(-0.0119168898298866,-0.0344587553480055,
-0.0136071812099891));
#24074=CARTESIAN_POINT('Ctrl Pts',(-0.0120828077546296,-0.0344487351974828,
-0.0136639080563882));
#24075=CARTESIAN_POINT('Ctrl Pts',(-0.0121670083159569,-0.0344436930623477,
-0.0136849832016467));
#24076=CARTESIAN_POINT('Ctrl Pts',(-0.0122769000602528,-0.0344374432036704,
-0.0137028388305269));
#24077=CARTESIAN_POINT('Ctrl Pts',(-0.0123013598632317,-0.0344360734899141,
-0.0137062129303402));
#24078=CARTESIAN_POINT('Ctrl Pts',(-0.0123424517868188,-0.0344338193407467,
-0.013710879460063));
#24079=CARTESIAN_POINT('Ctrl Pts',(-0.0123590425179456,-0.0344329219829101,
-0.0137124917688753));
#24080=CARTESIAN_POINT('Ctrl Pts',(-0.0123824308491513,-0.0344316779667341,
-0.0137143826762979));
#24081=CARTESIAN_POINT('Ctrl Pts',(-0.0123892086150432,-0.0344313199386283,
-0.0137148855996492));
#24082=CARTESIAN_POINT('Ctrl Pts',(-0.012400852788297,-0.0344307093644327,
-0.013715672298297));
#24083=CARTESIAN_POINT('Ctrl Pts',(-0.0124057175844363,-0.0344304556306669,
-0.0137159778227638));
#24084=CARTESIAN_POINT('Ctrl Pts',(-0.0124159419035796,-0.0344299252977918,
-0.0137165713143825));
#24085=CARTESIAN_POINT('Ctrl Pts',(-0.0124213015638884,-0.0344296489678495,
-0.0137168543776347));
#24086=CARTESIAN_POINT('Ctrl Pts',(-0.0124358106491749,-0.034428905190079,
-0.0137175447609512));
#24087=CARTESIAN_POINT('Ctrl Pts',(-0.0124449625339696,-0.0344284406330838,
-0.0137178986036904));
#24088=CARTESIAN_POINT('Ctrl Pts',(-0.0124886603330122,-0.0344262421684204,
-0.0137191985795725));
#24089=CARTESIAN_POINT('Ctrl Pts',(-0.0125232305406614,-0.0344245614994274,
-0.0137190655004037));
#24090=CARTESIAN_POINT('Ctrl Pts',(-0.0126460070657806,-0.0344187120481743,
-0.013714465577828));
#24091=CARTESIAN_POINT('Ctrl Pts',(-0.0127338029101666,-0.0344147407483755,
-0.0137035914232518));
#24092=CARTESIAN_POINT('Ctrl Pts',(-0.0129076304177375,-0.0344065857117213,
-0.0136667175489091));
#24093=CARTESIAN_POINT('Ctrl Pts',(-0.012993286343299,-0.0344024120093137,
-0.0136406075715908));
#24094=CARTESIAN_POINT('Ctrl Pts',(-0.0130916959270272,-0.034397158417778,
-0.0136009933410134));
#24095=CARTESIAN_POINT('Ctrl Pts',(-0.0131070949117104,-0.034396322868048,
-0.0135945019342409));
#24096=CARTESIAN_POINT('Ctrl Pts',(-0.0131312543787784,-0.0343949892459798,
-0.0135838521713802));
#24097=CARTESIAN_POINT('Ctrl Pts',(-0.0131400865170009,-0.0343944968345006,
-0.0135798590541857));
#24098=CARTESIAN_POINT('Ctrl Pts',(-0.0131566265255959,-0.0343935652570884,
-0.0135721926080917));
#24099=CARTESIAN_POINT('Ctrl Pts',(-0.0131643426920788,-0.034393126753125,
-0.0135685379883299));
#24100=CARTESIAN_POINT('Ctrl Pts',(-0.0131816743247193,-0.0343921328035431,
-0.0135601523686827));
#24101=CARTESIAN_POINT('Ctrl Pts',(-0.0131912715675292,-0.0343915760947242,
-0.0135553848903495));
#24102=CARTESIAN_POINT('Ctrl Pts',(-0.0132201729881524,-0.0343898800699295,
-0.0135406506478272));
#24103=CARTESIAN_POINT('Ctrl Pts',(-0.0132393164956937,-0.0343887299648524,
-0.0135303760897539));
#24104=CARTESIAN_POINT('Ctrl Pts',(-0.0133439590897324,-0.034382291844298,
-0.0134713338477309));
#24105=CARTESIAN_POINT('Ctrl Pts',(-0.0134248458984153,-0.0343767256154551,
-0.0134148819204856));
#24106=CARTESIAN_POINT('Ctrl Pts',(-0.0135550778538552,-0.0343669025282936,
-0.0133040941262781));
#24107=CARTESIAN_POINT('Ctrl Pts',(-0.0136069739435985,-0.0343627037007513,
-0.0132532232252696));
#24108=CARTESIAN_POINT('Ctrl Pts',(-0.013677372847466,-0.0343567640962357,
-0.0131737365056892));
#24109=CARTESIAN_POINT('Ctrl Pts',(-0.0136988222322934,-0.0343549168131173,
-0.0131478632159134));
#24110=CARTESIAN_POINT('Ctrl Pts',(-0.0137247641618978,-0.0343526552957386,
-0.0131144043359448));
#24111=CARTESIAN_POINT('Ctrl Pts',(-0.0137300586754671,-0.0343521922225408,
-0.013107454588873));
#24112=CARTESIAN_POINT('Ctrl Pts',(-0.0137384545114311,-0.0343514559544015,
-0.0130962375767377));
#24113=CARTESIAN_POINT('Ctrl Pts',(-0.0137415934031003,-0.034351180244284,
-0.0130919988216753));
#24114=CARTESIAN_POINT('Ctrl Pts',(-0.0137475817111962,-0.0343506535243498,
-0.0130838249142345));
#24115=CARTESIAN_POINT('Ctrl Pts',(-0.0137504343479523,-0.03435040230315,
-0.0130798923037048));
#24116=CARTESIAN_POINT('Ctrl Pts',(-0.0137573439934643,-0.0343497928862808,
-0.0130702714750008));
#24117=CARTESIAN_POINT('Ctrl Pts',(-0.0137613810865214,-0.0343494360404971,
-0.013064568973313));
#24118=CARTESIAN_POINT('Ctrl Pts',(-0.0137728329372339,-0.0343484209271794,
-0.0130481576846542));
#24119=CARTESIAN_POINT('Ctrl Pts',(-0.0137801511740157,-0.0343477687156927,
-0.0130373819519556));
#24120=CARTESIAN_POINT('Ctrl Pts',(-0.0138318843500512,-0.034343122660757,
-0.0129590925156564));
#24121=CARTESIAN_POINT('Ctrl Pts',(-0.0138710754892787,-0.0343394053229053,
-0.0128882676210948));
#24122=CARTESIAN_POINT('Ctrl Pts',(-0.0139500787897683,-0.0343306739126644,
-0.012714572418188));
#24123=CARTESIAN_POINT('Ctrl Pts',(-0.0139847782156196,-0.0343256821182595,
-0.0126098792706016));
#24124=CARTESIAN_POINT('Ctrl Pts',(-0.0140132724251587,-0.0343191116588909,
-0.0124782832610245));
#24125=CARTESIAN_POINT('Ctrl Pts',(-0.0140179130323191,-0.0343178916782183,
-0.0124540569241657));
#24126=CARTESIAN_POINT('Ctrl Pts',(-0.0140238234510058,-0.0343160879454099,
-0.0124186245096236));
#24127=CARTESIAN_POINT('Ctrl Pts',(-0.0140255543805702,-0.0343155188157125,
-0.0124074987048593));
#24128=CARTESIAN_POINT('Ctrl Pts',(-0.0140283923323993,-0.0343145081406761,
-0.0123878434683056));
#24129=CARTESIAN_POINT('Ctrl Pts',(-0.0140295501047151,-0.0343140682283638,
-0.0123793217904838));
#24130=CARTESIAN_POINT('Ctrl Pts',(-0.0140318229146649,-0.0343131432033015,
-0.0123614758534347));
#24131=CARTESIAN_POINT('Ctrl Pts',(-0.0140329241873776,-0.0343126576730004,
-0.0123521502228244));
#24132=CARTESIAN_POINT('Ctrl Pts',(-0.0140355963351681,-0.0343113736545842,
-0.0123276002306477));
#24133=CARTESIAN_POINT('Ctrl Pts',(-0.0140370259083655,-0.0343105707436344,
-0.012312361798405));
#24134=CARTESIAN_POINT('Ctrl Pts',(-0.0140414088711038,-0.0343076187357149,
-0.0122567584652518));
#24135=CARTESIAN_POINT('Ctrl Pts',(-0.0140430000002715,-0.0343054280631435,
-0.0122163101074072));
#24136=CARTESIAN_POINT('Ctrl Pts',(-0.014043,-0.0343031952477557,-0.0121758532762046));
#24137=CARTESIAN_POINT('Ctrl Pts',(-0.014043,-0.0344186209509151,-0.012175853286558));
#24138=CARTESIAN_POINT('Ctrl Pts',(-0.014043,-0.0344212507268401,-0.0122218434604753));
#24139=CARTESIAN_POINT('Ctrl Pts',(-0.0140409438983355,-0.0344238559182217,
-0.0122678573148423));
#24140=CARTESIAN_POINT('Ctrl Pts',(-0.0140349925434263,-0.0344275142554532,
-0.0123341798515428));
#24141=CARTESIAN_POINT('Ctrl Pts',(-0.014032753055036,-0.0344286252473827,
-0.0123545641161567));
#24142=CARTESIAN_POINT('Ctrl Pts',(-0.014029127197785,-0.0344301204238227,
-0.0123824369283828));
#24143=CARTESIAN_POINT('Ctrl Pts',(-0.0140280908529206,-0.0344305220049617,
-0.0123899680641488));
#24144=CARTESIAN_POINT('Ctrl Pts',(-0.0140263465288212,-0.0344311586276199,
-0.0124019857676221));
#24145=CARTESIAN_POINT('Ctrl Pts',(-0.0140256743384956,-0.0344313956230572,
-0.0124064773073147));
#24146=CARTESIAN_POINT('Ctrl Pts',(-0.0140242176896289,-0.0344318920770031,
-0.012415925392678));
#24147=CARTESIAN_POINT('Ctrl Pts',(-0.0140234288656404,-0.0344321512710044,
-0.0124208811903783));
#24148=CARTESIAN_POINT('Ctrl Pts',(-0.014021402918539,-0.0344327938360067,
-0.0124332211438851));
#24149=CARTESIAN_POINT('Ctrl Pts',(-0.0140201361843025,-0.0344331755607431,
-0.0124406004113445));
#24150=CARTESIAN_POINT('Ctrl Pts',(-0.0140150577362094,-0.0344346331018128,
-0.0124689456686067));
#24151=CARTESIAN_POINT('Ctrl Pts',(-0.0140108654191812,-0.0344356891821672,
-0.0124898419133742));
#24152=CARTESIAN_POINT('Ctrl Pts',(-0.0139986874897082,-0.0344384250248136,
-0.0125446308192381));
#24153=CARTESIAN_POINT('Ctrl Pts',(-0.0139899851396795,-0.0344400752532725,
-0.0125783524600527));
#24154=CARTESIAN_POINT('Ctrl Pts',(-0.0139614688427985,-0.0344447874594057,
-0.012675183064974));
#24155=CARTESIAN_POINT('Ctrl Pts',(-0.0139387301644725,-0.0344477820149067,
-0.0127373489605207));
#24156=CARTESIAN_POINT('Ctrl Pts',(-0.0138746491574022,-0.034455067885897,
-0.0128828236496189));
#24157=CARTESIAN_POINT('Ctrl Pts',(-0.0138296375007157,-0.0344593888479459,
-0.0129642244645762));
#24158=CARTESIAN_POINT('Ctrl Pts',(-0.0137681720549098,-0.0344648141028137,
-0.013054983881949));
#24159=CARTESIAN_POINT('Ctrl Pts',(-0.0137585300794762,-0.0344656532479546,
-0.0130687323241851));
#24160=CARTESIAN_POINT('Ctrl Pts',(-0.0137428898990631,-0.0344669973190432,
-0.0130902768021956));
#24161=CARTESIAN_POINT('Ctrl Pts',(-0.0137370380960509,-0.0344674965869797,
-0.0130981777469375));
#24162=CARTESIAN_POINT('Ctrl Pts',(-0.0137259487763708,-0.0344684362777711,
-0.0131128548529574));
#24163=CARTESIAN_POINT('Ctrl Pts',(-0.0137207295603245,-0.0344688759688194,
-0.0131196444045108));
#24164=CARTESIAN_POINT('Ctrl Pts',(-0.0137089099485386,-0.0344698661564612,
-0.0131347581766962));
#24165=CARTESIAN_POINT('Ctrl Pts',(-0.0137022796029769,-0.0344704178421874,
-0.0131430583323764));
#24166=CARTESIAN_POINT('Ctrl Pts',(-0.0136822220287321,-0.0344720759439644,
-0.0131676423327415));
#24167=CARTESIAN_POINT('Ctrl Pts',(-0.0136685462341116,-0.0344731924098364,
-0.013183719387019));
#24168=CARTESIAN_POINT('Ctrl Pts',(-0.013601830900007,-0.0344785752545321,
-0.0132589651751012));
#24169=CARTESIAN_POINT('Ctrl Pts',(-0.0135446091033189,-0.0344830159552006,
-0.0133142520737316));
#24170=CARTESIAN_POINT('Ctrl Pts',(-0.0134185518572565,-0.0344923550363818,
-0.0134185082873221));
#24171=CARTESIAN_POINT('Ctrl Pts',(-0.0133494350079558,-0.0344972493751752,
-0.0134667402443044));
#24172=CARTESIAN_POINT('Ctrl Pts',(-0.0132418511657536,-0.0345042684666625,
-0.0135294172345303));
#24173=CARTESIAN_POINT('Ctrl Pts',(-0.0132061847201313,-0.0345065049803165,
-0.0135483627201609));
#24174=CARTESIAN_POINT('Ctrl Pts',(-0.0131611701940534,-0.0345091814720202,
-0.0135700537865768));
#24175=CARTESIAN_POINT('Ctrl Pts',(-0.0131524877115586,-0.0345096911585609,
-0.013574138255789));
#24176=CARTESIAN_POINT('Ctrl Pts',(-0.0131387902837861,-0.0345104843077879,
-0.0135804265195531));
#24177=CARTESIAN_POINT('Ctrl Pts',(-0.0131338008787443,-0.0345107709621863,
-0.0135826849898683));
#24178=CARTESIAN_POINT('Ctrl Pts',(-0.013124353670445,-0.0345113093241089,
-0.0135869008390902));
#24179=CARTESIAN_POINT('Ctrl Pts',(-0.0131198985359548,-0.0345115613494253,
-0.0135888637276754));
#24180=CARTESIAN_POINT('Ctrl Pts',(-0.0131093386806568,-0.0345121544506331,
-0.0135934567415438));
#24181=CARTESIAN_POINT('Ctrl Pts',(-0.0131032260643617,-0.0345124944268501,
-0.0135960685877475));
#24182=CARTESIAN_POINT('Ctrl Pts',(-0.0130826620287619,-0.0345136275953856,
-0.0136046986297439));
#24183=CARTESIAN_POINT('Ctrl Pts',(-0.0130681355260242,-0.0345144106331394,
-0.0136105365666277));
#24184=CARTESIAN_POINT('Ctrl Pts',(-0.0130323805919522,-0.0345163013261759,
-0.0136242775637009));
#24185=CARTESIAN_POINT('Ctrl Pts',(-0.0130110618042765,-0.0345173974993715,
-0.0136319363528153));
#24186=CARTESIAN_POINT('Ctrl Pts',(-0.0129203948004886,-0.0345219585292715,
-0.0136622717458253));
#24187=CARTESIAN_POINT('Ctrl Pts',(-0.0128496497782722,-0.0345252747761337,
-0.0136804854118785));
#24188=CARTESIAN_POINT('Ctrl Pts',(-0.012681684620417,-0.0345330813399018,
-0.0137112369833737));
#24189=CARTESIAN_POINT('Ctrl Pts',(-0.0125840398651382,-0.0345375805294642,
-0.0137196627070563));
#24190=CARTESIAN_POINT('Ctrl Pts',(-0.0124644990598134,-0.0345434431340746,
-0.0137185983581558));
#24191=CARTESIAN_POINT('Ctrl Pts',(-0.012442743171024,-0.0345445235251208,
-0.0137179441623546));
#24192=CARTESIAN_POINT('Ctrl Pts',(-0.0124102721184903,-0.0345461590552488,
-0.0137162796858622));
#24193=CARTESIAN_POINT('Ctrl Pts',(-0.0123995414261918,-0.0345467033036156,
-0.0137156171164198));
#24194=CARTESIAN_POINT('Ctrl Pts',(-0.0123802671483107,-0.0345476879542266,
-0.0137142246835322));
#24195=CARTESIAN_POINT('Ctrl Pts',(-0.0123717210068596,-0.0345481270513804,
-0.0137135356356726));
#24196=CARTESIAN_POINT('Ctrl Pts',(-0.0123534764071276,-0.0345490699698217,
-0.0137119114773233));
#24197=CARTESIAN_POINT('Ctrl Pts',(-0.0123437802057966,-0.0345495744283035,
-0.013710955660578));
#24198=CARTESIAN_POINT('Ctrl Pts',(-0.012317367260995,-0.0345509579434118,
-0.0137080991329777));
#24199=CARTESIAN_POINT('Ctrl Pts',(-0.0123006718484562,-0.0345518426943833,
-0.0137060167774706));
#24200=CARTESIAN_POINT('Ctrl Pts',(-0.0121929255386265,-0.0345576205837428,
-0.0136907847209407));
#24201=CARTESIAN_POINT('Ctrl Pts',(-0.0121031840000439,-0.03456276464901,
-0.0136697892702447));
#24202=CARTESIAN_POINT('Ctrl Pts',(-0.0119278500652107,-0.0345733294245694,
-0.0136118493040906));
#24203=CARTESIAN_POINT('Ctrl Pts',(-0.0118426414073102,-0.0345787284675585,
-0.0135748959628348));
#24204=CARTESIAN_POINT('Ctrl Pts',(-0.011736278603535,-0.0345854665044419,
-0.0135168933738501));
#24205=CARTESIAN_POINT('Ctrl Pts',(-0.0117116738317919,-0.0345870239106572,
-0.0135025789304071));
#24206=CARTESIAN_POINT('Ctrl Pts',(-0.0116801682658603,-0.0345890025386721,
-0.0134830636198682));
#24207=CARTESIAN_POINT('Ctrl Pts',(-0.011672896614481,-0.0345894581002025,
-0.0134784748448617));
#24208=CARTESIAN_POINT('Ctrl Pts',(-0.0116612403164175,-0.0345901860513018,
-0.0134709821767271));
#24209=CARTESIAN_POINT('Ctrl Pts',(-0.0116568315909705,-0.0345904608443533,
-0.0134681162956237));
#24210=CARTESIAN_POINT('Ctrl Pts',(-0.0116482954647415,-0.0345909917094007,
-0.0134625051255732));
#24211=CARTESIAN_POINT('Ctrl Pts',(-0.011644166533352,-0.0345912479316971,
-0.013459762414175));
#24212=CARTESIAN_POINT('Ctrl Pts',(-0.011634093270176,-0.0345918718315033,
-0.0134530008972992));
#24213=CARTESIAN_POINT('Ctrl Pts',(-0.0116281635339138,-0.0345922380702319,
-0.0134489603773653));
#24214=CARTESIAN_POINT('Ctrl Pts',(-0.0116065999958337,-0.0345935669625945,
-0.0134340456745451));
#24215=CARTESIAN_POINT('Ctrl Pts',(-0.0115911391205138,-0.0345945140808452,
-0.0134229232989986));
#24216=CARTESIAN_POINT('Ctrl Pts',(-0.0115521392417426,-0.0345968992515924,
-0.0133937565659356));
#24217=CARTESIAN_POINT('Ctrl Pts',(-0.0115289068157599,-0.0345983163853198,
-0.0133753142510458));
#24218=CARTESIAN_POINT('Ctrl Pts',(-0.0114514862346744,-0.0346030787644519,
-0.0133101315167793));
#24219=CARTESIAN_POINT('Ctrl Pts',(-0.0114000225827501,-0.0346063175145695,
-0.0132602972377898));
#24220=CARTESIAN_POINT('Ctrl Pts',(-0.0112883237706678,-0.0346139721258716,
-0.0131359705705696));
#24221=CARTESIAN_POINT('Ctrl Pts',(-0.0112311951148977,-0.0346184113773414,
-0.0130590951188015));
#24222=CARTESIAN_POINT('Ctrl Pts',(-0.0111728350093234,-0.0346239717535003,
-0.0129631038363583));
#24223=CARTESIAN_POINT('Ctrl Pts',(-0.0111643558936737,-0.034624809994748,
-0.0129486308316105));
#24224=CARTESIAN_POINT('Ctrl Pts',(-0.0111512856205181,-0.0346261529418966,
-0.0129254632569788));
#24225=CARTESIAN_POINT('Ctrl Pts',(-0.0111465386009794,-0.0346266520062032,
-0.0129168578889023));
#24226=CARTESIAN_POINT('Ctrl Pts',(-0.0111378093737311,-0.0346275915178356,
-0.012900669844358));
#24227=CARTESIAN_POINT('Ctrl Pts',(-0.0111338074505789,-0.0346280312360786,
-0.0128930981950225));
#24228=CARTESIAN_POINT('Ctrl Pts',(-0.0111249804694063,-0.0346290217558974,
-0.0128760555893368));
#24229=CARTESIAN_POINT('Ctrl Pts',(-0.0111201898570151,-0.0346295737501186,
-0.0128665673634514));
#24230=CARTESIAN_POINT('Ctrl Pts',(-0.0111061675002692,-0.0346312337242514,
-0.0128380667285328));
#24231=CARTESIAN_POINT('Ctrl Pts',(-0.0110972282144649,-0.0346323517877049,
-0.0128189138885718));
#24232=CARTESIAN_POINT('Ctrl Pts',(-0.0110564691595448,-0.0346377492536229,
-0.0127266884485972));
#24233=CARTESIAN_POINT('Ctrl Pts',(-0.0110299528350907,-0.0346422040800077,
-0.0126514153285098));
#24234=CARTESIAN_POINT('Ctrl Pts',(-0.0109875065077053,-0.0346515861904159,
-0.0124926748650385));
#24235=CARTESIAN_POINT('Ctrl Pts',(-0.01097240774431,-0.0346565098378627,
-0.0124092508181465));
#24236=CARTESIAN_POINT('Ctrl Pts',(-0.0109603913409666,-0.0346635128933569,
-0.0122855251281353));
#24237=CARTESIAN_POINT('Ctrl Pts',(-0.010958080395888,-0.0346657093357846,
-0.0122459042652407));
#24238=CARTESIAN_POINT('Ctrl Pts',(-0.0109571111242769,-0.034668345670086,
-0.0121966884258337));
#24239=CARTESIAN_POINT('Ctrl Pts',(-0.0109570117242127,-0.0346688528747534,
-0.0121871393696784));
#24240=CARTESIAN_POINT('Ctrl Pts',(-0.010956994824899,-0.0346696430421348,
-0.0121721230666707));
#24241=CARTESIAN_POINT('Ctrl Pts',(-0.0109570177247147,-0.0346699291585376,
-0.0121666562813285));
#24242=CARTESIAN_POINT('Ctrl Pts',(-0.0109571159709193,-0.0346704671196264,
-0.0121563186645673));
#24243=CARTESIAN_POINT('Ctrl Pts',(-0.010957185328934,-0.0346707192749122,
-0.0121514479661761));
#24244=CARTESIAN_POINT('Ctrl Pts',(-0.0109574042410045,-0.0346713134964511,
-0.0121399120923173));
#24245=CARTESIAN_POINT('Ctrl Pts',(-0.0109575739297537,-0.0346716544506249,
-0.0121332473469337));
#24246=CARTESIAN_POINT('Ctrl Pts',(-0.0109582904115228,-0.0346727944660679,
-0.0121108203325944));
#24247=CARTESIAN_POINT('Ctrl Pts',(-0.0109590356851479,-0.0346735832046999,
-0.0120950649399482));
#24248=CARTESIAN_POINT('Ctrl Pts',(-0.0109614536953316,-0.0346754904615439,
-0.0120564896014039));
#24249=CARTESIAN_POINT('Ctrl Pts',(-0.0109633926884691,-0.03467659723158,
-0.0120336897343118));
#24250=CARTESIAN_POINT('Ctrl Pts',(-0.0109737857491623,-0.0346812339026118,
-0.0119370044324663));
#24251=CARTESIAN_POINT('Ctrl Pts',(-0.0109870682727495,-0.0346846102113984,
-0.0118637354869106));
#24252=CARTESIAN_POINT('Ctrl Pts',(-0.0110294743414793,-0.0346923988376801,
-0.0116987662729677));
#24253=CARTESIAN_POINT('Ctrl Pts',(-0.0110619818392575,-0.0346968199988048,
-0.011608262439399));
#24254=CARTESIAN_POINT('Ctrl Pts',(-0.0111119193099963,-0.0347025934885319,
-0.0115016460443384));
#24255=CARTESIAN_POINT('Ctrl Pts',(-0.0111215742441188,-0.034703674693506,
-0.0114821200642037));
#24256=CARTESIAN_POINT('Ctrl Pts',(-0.0111366086924991,-0.0347053112167356,
-0.0114532684840331));
#24257=CARTESIAN_POINT('Ctrl Pts',(-0.0111416779145405,-0.0347058556241761,
-0.0114437837825054));
#24258=CARTESIAN_POINT('Ctrl Pts',(-0.0111509661488267,-0.0347068404469925,
-0.0114268338048159));
#24259=CARTESIAN_POINT('Ctrl Pts',(-0.0111551490551011,-0.0347072795552926,
-0.0114193491902687));
#24260=CARTESIAN_POINT('Ctrl Pts',(-0.0111642169170902,-0.0347082223703798,
-0.0114034366618691));
#24261=CARTESIAN_POINT('Ctrl Pts',(-0.0111691197225938,-0.0347087267129308,
-0.0113950193938277));
#24262=CARTESIAN_POINT('Ctrl Pts',(-0.011182701766812,-0.034710109577188,
-0.0113722009507238));
#24263=CARTESIAN_POINT('Ctrl Pts',(-0.0111915370541682,-0.0347109937842608,
-0.0113578946071711));
#24264=CARTESIAN_POINT('Ctrl Pts',(-0.0112499986394791,-0.0347167496779284,
-0.0112666037139836));
#24265=CARTESIAN_POINT('Ctrl Pts',(-0.0113061556332917,-0.0347218699466105,
-0.011194033775052));
#24266=CARTESIAN_POINT('Ctrl Pts',(-0.0114309511580672,-0.0347323707039697,
-0.0110594091082525));
#24267=CARTESIAN_POINT('Ctrl Pts',(-0.0114994045822469,-0.0347377292348476,
-0.01099766722472));
#24268=CARTESIAN_POINT('Ctrl Pts',(-0.0115964408072155,-0.034744488767067,
-0.010924736496737));
#24269=CARTESIAN_POINT('Ctrl Pts',(-0.011620431400459,-0.0347460985075692,
-0.0109077556060341));
#24270=CARTESIAN_POINT('Ctrl Pts',(-0.0116521282506485,-0.034748132193312,
-0.010886652745782));
#24271=CARTESIAN_POINT('Ctrl Pts',(-0.0116594035212191,-0.0347485928061274,
-0.0108818972964116));
#24272=CARTESIAN_POINT('Ctrl Pts',(-0.0116711615260432,-0.0347493268534591,
-0.0108743527491169));
#24273=CARTESIAN_POINT('Ctrl Pts',(-0.01167561897002,-0.034749602761412,
-0.0108715248064854));
#24274=CARTESIAN_POINT('Ctrl Pts',(-0.0116842805814157,-0.0347501341877967,
-0.0108660917472102));
#24275=CARTESIAN_POINT('Ctrl Pts',(-0.0116884828674735,-0.0347503898732507,
-0.0108634839011457));
#24276=CARTESIAN_POINT('Ctrl Pts',(-0.011698761429683,-0.0347510102205853,
-0.0108571734990464));
#24277=CARTESIAN_POINT('Ctrl Pts',(-0.0117048510011,-0.0347513734828541,
-0.0108534926315561));
#24278=CARTESIAN_POINT('Ctrl Pts',(-0.0117269779680434,-0.0347526788612845,
-0.0108403260104871));
#24279=CARTESIAN_POINT('Ctrl Pts',(-0.0117431619490734,-0.034753606152339,
-0.0108310884782717));
#24280=CARTESIAN_POINT('Ctrl Pts',(-0.0117847432090315,-0.0347559295268815,
-0.0108083431553214));
#24281=CARTESIAN_POINT('Ctrl Pts',(-0.0118103586684988,-0.0347573060424203,
-0.0107952479045287));
#24282=CARTESIAN_POINT('Ctrl Pts',(-0.0119493823579586,-0.034764563769676,
-0.0107290111082644));
#24283=CARTESIAN_POINT('Ctrl Pts',(-0.0120685763625761,-0.0347700819971045,
-0.0106891089616857));
#24284=CARTESIAN_POINT('Ctrl Pts',(-0.0122378970252888,-0.0347782528460791,
-0.0106545334591239));
#24285=CARTESIAN_POINT('Ctrl Pts',(-0.0122849180065759,-0.0347805502851189,
-0.0106471769961609));
#24286=CARTESIAN_POINT('Ctrl Pts',(-0.0123468933462481,-0.0347836511966907,
-0.0106403970701265));
#24287=CARTESIAN_POINT('Ctrl Pts',(-0.0123616074013197,-0.0347843926393942,
-0.0106390010134324));
#24288=CARTESIAN_POINT('Ctrl Pts',(-0.012385612520354,-0.0347856116538727,
-0.0106370709562861));
#24289=CARTESIAN_POINT('Ctrl Pts',(-0.0123948925285678,-0.0347860851851846,
-0.0106364092408305));
#24290=CARTESIAN_POINT('Ctrl Pts',(-0.0124128416008519,-0.0347870056835294,
-0.0106352924259929));
#24291=CARTESIAN_POINT('Ctrl Pts',(-0.0124215096514107,-0.0347874522899658,
-0.0106348264818894));
#24292=CARTESIAN_POINT('Ctrl Pts',(-0.0124417753208816,-0.0347885014552659,
-0.0106339085438657));
#24293=CARTESIAN_POINT('Ctrl Pts',(-0.0124533749188357,-0.034789105807075,
-0.010633514220517));
#24294=CARTESIAN_POINT('Ctrl Pts',(-0.0124914671727522,-0.0347911034375968,
-0.0106326493962043));
#24295=CARTESIAN_POINT('Ctrl Pts',(-0.0125179665803499,-0.0347925138192516,
-0.0106327304330261));
#24296=CARTESIAN_POINT('Ctrl Pts',(-0.0126295277406936,-0.0347985404059354,
-0.0106359455470927));
#24297=CARTESIAN_POINT('Ctrl Pts',(-0.0127142470947548,-0.0348033462275276,
-0.0106454323101142));
#24298=CARTESIAN_POINT('Ctrl Pts',(-0.0129006082005719,-0.0348142427166544,
-0.0106820820321214));
#24299=CARTESIAN_POINT('Ctrl Pts',(-0.0130011488008545,-0.0348203490665612,
-0.010712742995192));
#24300=CARTESIAN_POINT('Ctrl Pts',(-0.0131098159395933,-0.0348267247793116,
-0.0107584107980874));
#24301=CARTESIAN_POINT('Ctrl Pts',(-0.0131217610027258,-0.0348274221141635,
-0.0107636096936498));
#24302=CARTESIAN_POINT('Ctrl Pts',(-0.0131392927328714,-0.0348284388279881,
-0.0107715056629536));
#24303=CARTESIAN_POINT('Ctrl Pts',(-0.0131449309932392,-0.0348287647621707,
-0.0107740860224269));
#24304=CARTESIAN_POINT('Ctrl Pts',(-0.0131549318099693,-0.034829340815958,
-0.0107787360271017));
#24305=CARTESIAN_POINT('Ctrl Pts',(-0.01315930040594,-0.0348295917318798,
-0.0107807922523895));
#24306=CARTESIAN_POINT('Ctrl Pts',(-0.0131687873096692,-0.034830135021877,
-0.0107853120977104));
#24307=CARTESIAN_POINT('Ctrl Pts',(-0.0131739017150181,-0.0348304269145063,
-0.0107877834958212));
#24308=CARTESIAN_POINT('Ctrl Pts',(-0.0131884712285375,-0.0348312559053572,
-0.01079492332561));
#24309=CARTESIAN_POINT('Ctrl Pts',(-0.0131978924551705,-0.0348317889037202,
-0.0107996605957608));
#24310=CARTESIAN_POINT('Ctrl Pts',(-0.0132771326879101,-0.0348362519471852,
-0.0108405279466831));
#24311=CARTESIAN_POINT('Ctrl Pts',(-0.0133441528350246,-0.0348398985544469,
-0.0108818526568864));
#24312=CARTESIAN_POINT('Ctrl Pts',(-0.0135092295622997,-0.0348492609955216,
-0.0110019464219508));
#24313=CARTESIAN_POINT('Ctrl Pts',(-0.0136013257636308,-0.0348549164922762,
-0.0110878821278987));
#24314=CARTESIAN_POINT('Ctrl Pts',(-0.013693601149457,-0.0348619787007947,
-0.0111978496251147));
#24315=CARTESIAN_POINT('Ctrl Pts',(-0.0137049608330007,-0.0348628758751834,
-0.0112118801423067));
#24316=CARTESIAN_POINT('Ctrl Pts',(-0.0137228893480208,-0.0348643394227479,
-0.0112348361059553));
#24317=CARTESIAN_POINT('Ctrl Pts',(-0.0137296129122642,-0.0348648996281477,
-0.0112436388426649));
#24318=CARTESIAN_POINT('Ctrl Pts',(-0.0137413918132987,-0.0348659018439433,
-0.0112594093680791));
#24319=CARTESIAN_POINT('Ctrl Pts',(-0.0137464847513141,-0.0348663423497975,
-0.0112663485583684));
#24320=CARTESIAN_POINT('Ctrl Pts',(-0.0137571041425502,-0.0348672763137529,
-0.0112810743519968));
#24321=CARTESIAN_POINT('Ctrl Pts',(-0.0137626168971439,-0.0348677702764735,
-0.011288870348456));
#24322=CARTESIAN_POINT('Ctrl Pts',(-0.0137771251407206,-0.0348690951303613,
-0.0113097968826123));
#24323=CARTESIAN_POINT('Ctrl Pts',(-0.0137859902563478,-0.0348699309309308,
-0.0113230160484024));
#24324=CARTESIAN_POINT('Ctrl Pts',(-0.0138321383068054,-0.0348744261404011,
-0.0113941854307183));
#24325=CARTESIAN_POINT('Ctrl Pts',(-0.0138657082887652,-0.0348782212023065,
-0.0114544407312063));
#24326=CARTESIAN_POINT('Ctrl Pts',(-0.0139354997108496,-0.0348874499541373,
-0.0116021655012082));
#24327=CARTESIAN_POINT('Ctrl Pts',(-0.0139679273055855,-0.0348929562700478,
-0.0116911211347877));
#24328=CARTESIAN_POINT('Ctrl Pts',(-0.0140044249149756,-0.0349010831195163,
-0.0118295522751019));
#24329=CARTESIAN_POINT('Ctrl Pts',(-0.0140146018867452,-0.0349038007813811,
-0.0118771885495423));
#24330=CARTESIAN_POINT('Ctrl Pts',(-0.0140241282398028,-0.0349069469760492,
-0.0119350600933263));
#24331=CARTESIAN_POINT('Ctrl Pts',(-0.0140256512231199,-0.0349074768703016,
-0.0119449060873067));
#24332=CARTESIAN_POINT('Ctrl Pts',(-0.0140278833574914,-0.034908297470321,
-0.0119603237581672));
#24333=CARTESIAN_POINT('Ctrl Pts',(-0.014028657610351,-0.0349085916387056,
-0.011965885565256));
#24334=CARTESIAN_POINT('Ctrl Pts',(-0.014029978069052,-0.0349091107582605,
-0.0119757656751512));
#24335=CARTESIAN_POINT('Ctrl Pts',(-0.0140305363729834,-0.0349093363724382,
-0.0119800821051503));
#24336=CARTESIAN_POINT('Ctrl Pts',(-0.0140318364186023,-0.0349098770088289,
-0.0119904787904951));
#24337=CARTESIAN_POINT('Ctrl Pts',(-0.0140325602275405,-0.0349101910230965,
-0.0119965611545858));
#24338=CARTESIAN_POINT('Ctrl Pts',(-0.014034679258444,-0.034911152879147,
-0.0120153192144296));
#24339=CARTESIAN_POINT('Ctrl Pts',(-0.0140359536117413,-0.0349117943095468,
-0.0120280083099307));
#24340=CARTESIAN_POINT('Ctrl Pts',(-0.0140410215997774,-0.0349146720774839,
-0.0120856506686283));
#24341=CARTESIAN_POINT('Ctrl Pts',(-0.0140430000000296,-0.0349168242222948,
-0.0121307411443307));
#24342=CARTESIAN_POINT('Ctrl Pts',(-0.014043,-0.0349189332996453,-0.012175853287569));
#24343=CARTESIAN_POINT('Origin',(-0.0125,-0.0375520664398416,-0.0121758532865581));
#24344=CARTESIAN_POINT('',(-0.014043,-0.0354167228394876,-0.0121758532865582));
#24345=CARTESIAN_POINT('',(-0.014043,-0.0353007220219321,-0.0121758532865564));
#24346=CARTESIAN_POINT('',(-0.014043,-0.0375520664398416,-0.012175853286558));
#24347=CARTESIAN_POINT('Ctrl Pts',(-0.014043,-0.0353007220219321,-0.0121758532865547));
#24348=CARTESIAN_POINT('Ctrl Pts',(-0.0140429999999998,-0.0352954039244155,
-0.0120668252355584));
#24349=CARTESIAN_POINT('Ctrl Pts',(-0.0140314443207502,-0.0352905409360675,
-0.0119580939458071));
#24350=CARTESIAN_POINT('Ctrl Pts',(-0.013992016855839,-0.0352819214273844,
-0.0117747332594792));
#24351=CARTESIAN_POINT('Ctrl Pts',(-0.0139696823889352,-0.0352782525208751,
-0.0116993622952759));
#24352=CARTESIAN_POINT('Ctrl Pts',(-0.0139342467037295,-0.0352733685094644,
-0.0116064462491928));
#24353=CARTESIAN_POINT('Ctrl Pts',(-0.0139263830231519,-0.0352723273106245,
-0.011587024449181));
#24354=CARTESIAN_POINT('Ctrl Pts',(-0.0139139625982418,-0.0352707410170081,
-0.0115580584905924));
#24355=CARTESIAN_POINT('Ctrl Pts',(-0.0139096990796995,-0.035270205883243,
-0.0115483908282159));
#24356=CARTESIAN_POINT('Ctrl Pts',(-0.0139018164013339,-0.0352692327480824,
-0.0115310025523506));
#24357=CARTESIAN_POINT('Ctrl Pts',(-0.0138982318747997,-0.0352687959559578,
-0.0115232666540929));
#24358=CARTESIAN_POINT('Ctrl Pts',(-0.0138903910347189,-0.0352678524384189,
-0.0115067062526937));
#24359=CARTESIAN_POINT('Ctrl Pts',(-0.0138861144327696,-0.0352673450184413,
-0.0114978918159259));
#24360=CARTESIAN_POINT('Ctrl Pts',(-0.0138742990390152,-0.0352659620091812,
-0.011474118477497));
#24361=CARTESIAN_POINT('Ctrl Pts',(-0.0138666002714438,-0.0352650808339306,
-0.0114592409373305));
#24362=CARTESIAN_POINT('Ctrl Pts',(-0.013814677765236,-0.035259262822918,
-0.011362783696945));
#24363=CARTESIAN_POINT('Ctrl Pts',(-0.0137634199271336,-0.0352540703848136,
-0.0112852212326224));
#24364=CARTESIAN_POINT('Ctrl Pts',(-0.013653473927396,-0.0352439889131749,
-0.0111476032717579));
#24365=CARTESIAN_POINT('Ctrl Pts',(-0.0135962395857289,-0.0352391429977949,
-0.0110867897838852));
#24366=CARTESIAN_POINT('Ctrl Pts',(-0.0135163933747742,-0.0352331068429438,
-0.0110146553940041));
#24367=CARTESIAN_POINT('Ctrl Pts',(-0.0134980338822266,-0.0352317634746433,
-0.0109988382010494));
#24368=CARTESIAN_POINT('Ctrl Pts',(-0.013466604489085,-0.035229547708235,
-0.0109730253575504));
#24369=CARTESIAN_POINT('Ctrl Pts',(-0.0134537337931488,-0.0352286629071687,
-0.0109627946896621));
#24370=CARTESIAN_POINT('Ctrl Pts',(-0.0134353434495738,-0.0352274330920666,
-0.0109486502374509));
#24371=CARTESIAN_POINT('Ctrl Pts',(-0.013429958218279,-0.0352270770411098,
-0.0109445643651442));
#24372=CARTESIAN_POINT('Ctrl Pts',(-0.0134206484985942,-0.0352264687515745,
-0.0109375968334244));
#24373=CARTESIAN_POINT('Ctrl Pts',(-0.0134167369357639,-0.0352262153485278,
-0.0109346981412629));
#24374=CARTESIAN_POINT('Ctrl Pts',(-0.01340847136182,-0.0352256845293894,
-0.0109286332721922));
#24375=CARTESIAN_POINT('Ctrl Pts',(-0.0134041144373421,-0.0352254073949649,
-0.0109254713187599));
#24376=CARTESIAN_POINT('Ctrl Pts',(-0.0133922405522074,-0.0352246590822618,
-0.0109169485893466));
#24377=CARTESIAN_POINT('Ctrl Pts',(-0.0133846917712237,-0.035224190855451,
-0.0109116322941855));
#24378=CARTESIAN_POINT('Ctrl Pts',(-0.0133479044577275,-0.0352219428535436,
-0.0108862153831996));
#24379=CARTESIAN_POINT('Ctrl Pts',(-0.0133180243757956,-0.0352202192728915,
-0.0108670582879946));
#24380=CARTESIAN_POINT('Ctrl Pts',(-0.0132122357564922,-0.0352143702231927,
-0.0108042735573172));
#24381=CARTESIAN_POINT('Ctrl Pts',(-0.0131332944278842,-0.0352104329567915,
-0.0107660835988117));
#24382=CARTESIAN_POINT('Ctrl Pts',(-0.0129683167857677,-0.0352023251367187,
-0.0107029417246487));
#24383=CARTESIAN_POINT('Ctrl Pts',(-0.012882500628084,-0.0351981634880242,
-0.010678362021703));
#24384=CARTESIAN_POINT('Ctrl Pts',(-0.012778655598113,-0.0351929239911381,
-0.010658131625068));
#24385=CARTESIAN_POINT('Ctrl Pts',(-0.0127622106391915,-0.0351920888212098,
-0.0106552042352081));
#24386=CARTESIAN_POINT('Ctrl Pts',(-0.0127361543326203,-0.0351907556674694,
-0.0106510011464575));
#24387=CARTESIAN_POINT('Ctrl Pts',(-0.0127265726986002,-0.0351902633375946,
-0.01064954803379));
#24388=CARTESIAN_POINT('Ctrl Pts',(-0.0127085249136169,-0.0351893318289823,
-0.0106469846659262));
#24389=CARTESIAN_POINT('Ctrl Pts',(-0.0127000619727321,-0.0351888933111071,
-0.0106458542336471));
#24390=CARTESIAN_POINT('Ctrl Pts',(-0.0126809545641554,-0.0351878992136181,
-0.0106434632142573));
#24391=CARTESIAN_POINT('Ctrl Pts',(-0.0126703055404811,-0.0351873423692668,
-0.0106422431982268));
#24392=CARTESIAN_POINT('Ctrl Pts',(-0.0126387363420048,-0.035185682980067,
-0.010638959300821));
#24393=CARTESIAN_POINT('Ctrl Pts',(-0.0126177863232004,-0.0351845705588175,
-0.0106372119316136));
#24394=CARTESIAN_POINT('Ctrl Pts',(-0.0124852085743953,-0.0351774578972247,
-0.01062887758477));
#24395=CARTESIAN_POINT('Ctrl Pts',(-0.0123731930680936,-0.0351710867988278,
-0.010634014935825));
#24396=CARTESIAN_POINT('Ctrl Pts',(-0.0122005870972706,-0.0351610376918551,
-0.0106608757977568));
#24397=CARTESIAN_POINT('Ctrl Pts',(-0.0121390862371291,-0.0351574179871451,
-0.0106743384554941));
#24398=CARTESIAN_POINT('Ctrl Pts',(-0.0120585119157,-0.0351527471264743,
-0.0106972146149091));
#24399=CARTESIAN_POINT('Ctrl Pts',(-0.0120385638115219,-0.0351515970117509,
-0.0107033177982365));
#24400=CARTESIAN_POINT('Ctrl Pts',(-0.0120047685959642,-0.0351496663071883,
-0.010714411792339));
#24401=CARTESIAN_POINT('Ctrl Pts',(-0.0119908581818634,-0.035148876834957,
-0.0107191995786856));
#24402=CARTESIAN_POINT('Ctrl Pts',(-0.0119709322680835,-0.0351477556995824,
-0.0107263781483005));
#24403=CARTESIAN_POINT('Ctrl Pts',(-0.0119648603949052,-0.0351474153798778,
-0.0107286088540636));
#24404=CARTESIAN_POINT('Ctrl Pts',(-0.0119542818187599,-0.0351468249986837,
-0.0107325709263451));
#24405=CARTESIAN_POINT('Ctrl Pts',(-0.0119497689460431,-0.035146573956988,
-0.010734285357502));
#24406=CARTESIAN_POINT('Ctrl Pts',(-0.0119401016879257,-0.0351460380040336,
-0.0107380099412361));
#24407=CARTESIAN_POINT('Ctrl Pts',(-0.0119349500096747,-0.0351457534843036,
-0.0107400266550166));
#24408=CARTESIAN_POINT('Ctrl Pts',(-0.0119208348724951,-0.0351449766368309,
-0.0107456400048453));
#24409=CARTESIAN_POINT('Ctrl Pts',(-0.011911894021667,-0.035144487579214,
-0.0107492932130306));
#24410=CARTESIAN_POINT('Ctrl Pts',(-0.0118626904962162,-0.0351418098454449,
-0.0107699388598854));
#24411=CARTESIAN_POINT('Ctrl Pts',(-0.011823126447455,-0.0351397073037646,
-0.0107885531898061));
#24412=CARTESIAN_POINT('Ctrl Pts',(-0.0117119147232486,-0.0351338015823805,
-0.0108467689940691));
#24413=CARTESIAN_POINT('Ctrl Pts',(-0.0116425566594987,-0.0351301181076973,
-0.0108904212873636));
#24414=CARTESIAN_POINT('Ctrl Pts',(-0.0115141668459892,-0.0351227544551838,
-0.0109862621410874));
#24415=CARTESIAN_POINT('Ctrl Pts',(-0.011455017796256,-0.0351190903796698,
-0.0110378705478477));
#24416=CARTESIAN_POINT('Ctrl Pts',(-0.011385365521147,-0.0351142123956274,
-0.0111086713064869));
#24417=CARTESIAN_POINT('Ctrl Pts',(-0.0113709874800098,-0.0351131718672164,
-0.0111238941253043));
#24418=CARTESIAN_POINT('Ctrl Pts',(-0.011349828628903,-0.0351115863931175,
-0.0111472297408439));
#24419=CARTESIAN_POINT('Ctrl Pts',(-0.0113428138672507,-0.0351110513925958,
-0.011155127648273));
#24420=CARTESIAN_POINT('Ctrl Pts',(-0.0113302849055304,-0.035110078398942,
-0.0111695291404365));
#24421=CARTESIAN_POINT('Ctrl Pts',(-0.0113247424344345,-0.0351096416134206,
-0.0111760076284687));
#24422=CARTESIAN_POINT('Ctrl Pts',(-0.0113129457698155,-0.0351086979963888,
-0.0111900301400834));
#24423=CARTESIAN_POINT('Ctrl Pts',(-0.0113067092040792,-0.0351081904690234,
-0.011197588449242));
#24424=CARTESIAN_POINT('Ctrl Pts',(-0.0112900021719658,-0.0351068068798073,
-0.0112182337664188));
#24425=CARTESIAN_POINT('Ctrl Pts',(-0.0112796724576945,-0.0351059252241669,
-0.011231432538834));
#24426=CARTESIAN_POINT('Ctrl Pts',(-0.0112142025544493,-0.0351001625459669,
-0.0113179544302265));
#24427=CARTESIAN_POINT('Ctrl Pts',(-0.0111654876927915,-0.0350950321715532,
-0.01139589293744));
#24428=CARTESIAN_POINT('Ctrl Pts',(-0.0110937374019318,-0.0350859598421296,
-0.0115373048732213));
#24429=CARTESIAN_POINT('Ctrl Pts',(-0.0110673942372996,-0.0350820868188733,
-0.0115988270375849));
#24430=CARTESIAN_POINT('Ctrl Pts',(-0.0110334265828864,-0.0350762875489232,
-0.0116949743341376));
#24431=CARTESIAN_POINT('Ctrl Pts',(-0.0110228620762184,-0.0350743124266521,
-0.0117284765310563));
#24432=CARTESIAN_POINT('Ctrl Pts',(-0.011007709068249,-0.035071203459733,
-0.0117829467605495));
#24433=CARTESIAN_POINT('Ctrl Pts',(-0.011002398593164,-0.0350700423918871,
-0.0118037002549353));
#24434=CARTESIAN_POINT('Ctrl Pts',(-0.0109958182990081,-0.0350685055922548,
-0.0118318439993315));
#24435=CARTESIAN_POINT('Ctrl Pts',(-0.0109941678664211,-0.0350681104843747,
-0.0118391418830467));
#24436=CARTESIAN_POINT('Ctrl Pts',(-0.0109915026899573,-0.0350674561582841,
-0.0118513384381392));
#24437=CARTESIAN_POINT('Ctrl Pts',(-0.0109904585788777,-0.0350671953104402,
-0.0118562305071027));
#24438=CARTESIAN_POINT('Ctrl Pts',(-0.0109883911160468,-0.0350666695781939,
-0.0118661535323106));
#24439=CARTESIAN_POINT('Ctrl Pts',(-0.01098736905088,-0.0350664047657853,
-0.0118711846647692));
#24440=CARTESIAN_POINT('Ctrl Pts',(-0.0109847998184951,-0.0350657259018598,
-0.0118841634403861));
#24441=CARTESIAN_POINT('Ctrl Pts',(-0.010983290044503,-0.0350653139284998,
-0.0118921184230557));
#24442=CARTESIAN_POINT('Ctrl Pts',(-0.010977497935617,-0.0350636777271097,
-0.0119240050983901));
#24443=CARTESIAN_POINT('Ctrl Pts',(-0.0109737186508502,-0.0350624792140348,
-0.0119480256991938));
#24444=CARTESIAN_POINT('Ctrl Pts',(-0.0109578393397728,-0.0350566554285851,
-0.012067240766773));
#24445=CARTESIAN_POINT('Ctrl Pts',(-0.0109540690501827,-0.0350523409907202,
-0.0121633367238258));
#24446=CARTESIAN_POINT('Ctrl Pts',(-0.0109643183224831,-0.0350436425809516,
-0.0123528815474466));
#24447=CARTESIAN_POINT('Ctrl Pts',(-0.0109779249888903,-0.03503927645826,
-0.012445931836608));
#24448=CARTESIAN_POINT('Ctrl Pts',(-0.0110038376878683,-0.0350337974195278,
-0.0125535176383299));
#24449=CARTESIAN_POINT('Ctrl Pts',(-0.0110080441755761,-0.0350329563818056,
-0.0125698073661045));
#24450=CARTESIAN_POINT('Ctrl Pts',(-0.0110150990930963,-0.0350316159939692,
-0.0125953919798349));
#24451=CARTESIAN_POINT('Ctrl Pts',(-0.0110177705011337,-0.0350311224051761,
-0.0126047345352977));
#24452=CARTESIAN_POINT('Ctrl Pts',(-0.0110229537242415,-0.0350301898307496,
-0.0126222344479279));
#24453=CARTESIAN_POINT('Ctrl Pts',(-0.0110254453359723,-0.0350297515230363,
-0.0126303974327609));
#24454=CARTESIAN_POINT('Ctrl Pts',(-0.0110312070057516,-0.0350287596830806,
-0.0126487276895015));
#24455=CARTESIAN_POINT('Ctrl Pts',(-0.0110345151401086,-0.0350282049095644,
-0.0126588824560726));
#24456=CARTESIAN_POINT('Ctrl Pts',(-0.011044811823034,-0.0350265207837027,
-0.0126894097408411));
#24457=CARTESIAN_POINT('Ctrl Pts',(-0.0110521215511163,-0.0350253808629573,
-0.012709670480015));
#24458=CARTESIAN_POINT('Ctrl Pts',(-0.0110978815623562,-0.0350185527313626,
-0.0128286433225629));
#24459=CARTESIAN_POINT('Ctrl Pts',(-0.0111459859520115,-0.0350125365676485,
-0.0129233228953379));
#24460=CARTESIAN_POINT('Ctrl Pts',(-0.0112397372329089,-0.0350025907139899,
-0.0130686469408664));
#24461=CARTESIAN_POINT('Ctrl Pts',(-0.0112797108605154,-0.034998723634024,
-0.0131225516702715));
#24462=CARTESIAN_POINT('Ctrl Pts',(-0.0113370428704942,-0.0349937727506698,
-0.0131901742023993));
#24463=CARTESIAN_POINT('Ctrl Pts',(-0.0113513663993812,-0.0349925793479096,
-0.0132063663307641));
#24464=CARTESIAN_POINT('Ctrl Pts',(-0.0113762711407729,-0.0349905842334855,
-0.0132333553820207));
#24465=CARTESIAN_POINT('Ctrl Pts',(-0.0113866791912224,-0.0349897728961346,
-0.0132443073291911));
#24466=CARTESIAN_POINT('Ctrl Pts',(-0.0114018193870056,-0.0349886266938911,
-0.0132597772134039));
#24467=CARTESIAN_POINT('Ctrl Pts',(-0.0114064217201269,-0.0349882826494873,
-0.0132644203661504));
#24468=CARTESIAN_POINT('Ctrl Pts',(-0.0114144798494721,-0.0349876880765889,
-0.0132724472823926));
#24469=CARTESIAN_POINT('Ctrl Pts',(-0.0114179222583034,-0.0349874365242794,
-0.01327584426474));
#24470=CARTESIAN_POINT('Ctrl Pts',(-0.0114253089867612,-0.034986902011804,
-0.0132830652825972));
#24471=CARTESIAN_POINT('Ctrl Pts',(-0.0114292578018425,-0.034986619415297,
-0.0132868844854979));
#24472=CARTESIAN_POINT('Ctrl Pts',(-0.0114400816704452,-0.0349858530587617,
-0.0132972417760865));
#24473=CARTESIAN_POINT('Ctrl Pts',(-0.0114469968651873,-0.0349853724250091,
-0.0133037377737417));
#24474=CARTESIAN_POINT('Ctrl Pts',(-0.0114839047410759,-0.0349828515031324,
-0.0133377729699757));
#24475=CARTESIAN_POINT('Ctrl Pts',(-0.0115149209544446,-0.0349808857910871,
-0.0133641826541099));
#24476=CARTESIAN_POINT('Ctrl Pts',(-0.0116129575030509,-0.0349749998726223,
-0.0134411791733277));
#24477=CARTESIAN_POINT('Ctrl Pts',(-0.0116830898665416,-0.0349712227064863,
-0.01348755183374));
#24478=CARTESIAN_POINT('Ctrl Pts',(-0.0118328091226443,-0.0349633739712203,
-0.0135698614872455));
#24479=CARTESIAN_POINT('Ctrl Pts',(-0.0119123648486291,-0.0349593075518563,
-0.0136052186328943));
#24480=CARTESIAN_POINT('Ctrl Pts',(-0.0120101869478757,-0.0349541793007366,
-0.0136391403398384));
#24481=CARTESIAN_POINT('Ctrl Pts',(-0.0120259934568373,-0.0349533472806077,
-0.0136443367206617));
#24482=CARTESIAN_POINT('Ctrl Pts',(-0.0120511214400963,-0.0349520180101334,
-0.0136521495603865));
#24483=CARTESIAN_POINT('Ctrl Pts',(-0.0120603890306984,-0.0349515263564394,
-0.0136549357182527));
#24484=CARTESIAN_POINT('Ctrl Pts',(-0.012077883232411,-0.0349505954142842,
-0.0136600161366901));
#24485=CARTESIAN_POINT('Ctrl Pts',(-0.0120861039010516,-0.0349501567774791,
-0.0136623296390623));
#24486=CARTESIAN_POINT('Ctrl Pts',(-0.0121047052241171,-0.0349491614382916,
-0.0136673982516778));
#24487=CARTESIAN_POINT('Ctrl Pts',(-0.0121150962177201,-0.034948603458306,
-0.0136701134423976));
#24488=CARTESIAN_POINT('Ctrl Pts',(-0.0121460073498791,-0.0349469374493509,
-0.0136778467765611));
#24489=CARTESIAN_POINT('Ctrl Pts',(-0.012166602548647,-0.0349458194270115,
-0.0136825521018522));
#24490=CARTESIAN_POINT('Ctrl Pts',(-0.0122947255159789,-0.0349388126536597,
-0.0137090684689962));
#24491=CARTESIAN_POINT('Ctrl Pts',(-0.0124042139206035,-0.034932568645501,
-0.0137197783838096));
#24492=CARTESIAN_POINT('Ctrl Pts',(-0.0125782423052445,-0.034922557396283,
-0.0137182112837191));
#24493=CARTESIAN_POINT('Ctrl Pts',(-0.0126424939810499,-0.0349188507740264,
-0.0137136068998331));
#24494=CARTESIAN_POINT('Ctrl Pts',(-0.0127272114952592,-0.0349140812326848,
-0.0137021790571953));
#24495=CARTESIAN_POINT('Ctrl Pts',(-0.0127480912002074,-0.0349129156397414,
-0.0136989246082645));
#24496=CARTESIAN_POINT('Ctrl Pts',(-0.0127835237595683,-0.0349109618661706,
-0.0136926538278739));
#24497=CARTESIAN_POINT('Ctrl Pts',(-0.0127981116420341,-0.0349101645404439,
-0.0136898543054446));
#24498=CARTESIAN_POINT('Ctrl Pts',(-0.0128190160397944,-0.0349090343917211,
-0.0136855287254055));
#24499=CARTESIAN_POINT('Ctrl Pts',(-0.0128253664859997,-0.0349086927259179,
-0.0136841728206991));
#24500=CARTESIAN_POINT('Ctrl Pts',(-0.0128364259129553,-0.0349081008337498,
-0.0136817383882204));
#24501=CARTESIAN_POINT('Ctrl Pts',(-0.0128411386736466,-0.0349078496114162,
-0.0136806777752841));
#24502=CARTESIAN_POINT('Ctrl Pts',(-0.0128512241017425,-0.0349073141969859,
-0.0136783582209965));
#24503=CARTESIAN_POINT('Ctrl Pts',(-0.0128565950578364,-0.0349070303861969,
-0.0136770925793525));
#24504=CARTESIAN_POINT('Ctrl Pts',(-0.0128712864437572,-0.0349062574096767,
-0.0136735473275669));
#24505=CARTESIAN_POINT('Ctrl Pts',(-0.012880592725105,-0.0349057714606663,
-0.0136712095151038));
#24506=CARTESIAN_POINT('Ctrl Pts',(-0.0129310147463276,-0.034903155717133,
-0.0136580418819085));
#24507=CARTESIAN_POINT('Ctrl Pts',(-0.0129716942854991,-0.0349011073682053,
-0.013645602173136));
#24508=CARTESIAN_POINT('Ctrl Pts',(-0.0130897874220151,-0.0348952097961284,
-0.0136040801035105));
#24509=CARTESIAN_POINT('Ctrl Pts',(-0.0131654377561261,-0.0348914892833095,
-0.0135704409539774));
#24510=CARTESIAN_POINT('Ctrl Pts',(-0.0133072120882321,-0.0348840708646198,
-0.0134932231306809));
#24511=CARTESIAN_POINT('Ctrl Pts',(-0.0133734004358846,-0.0348803900787379,
-0.0134503040488251));
#24512=CARTESIAN_POINT('Ctrl Pts',(-0.0134527021743808,-0.0348754912438697,
-0.0133897923203613));
#24513=CARTESIAN_POINT('Ctrl Pts',(-0.0134691238115638,-0.0348744483983488,
-0.0133767231361152));
#24514=CARTESIAN_POINT('Ctrl Pts',(-0.0134934098695993,-0.0348728600915784,
-0.013356572394316));
#24515=CARTESIAN_POINT('Ctrl Pts',(-0.0135014766692104,-0.0348723246302969,
-0.0133497379717983));
#24516=CARTESIAN_POINT('Ctrl Pts',(-0.0135159210123895,-0.0348713511465354,
-0.0133372430562134));
#24517=CARTESIAN_POINT('Ctrl Pts',(-0.0135223231194179,-0.0348709143374003,
-0.0133316115381396));
#24518=CARTESIAN_POINT('Ctrl Pts',(-0.0135359767387985,-0.0348699710615018,
-0.0133193991245462));
#24519=CARTESIAN_POINT('Ctrl Pts',(-0.013543212911812,-0.0348694639033336,
-0.0133128017029724));
#24520=CARTESIAN_POINT('Ctrl Pts',(-0.0135626401476217,-0.0348680823095054,
-0.0132947477319779));
#24521=CARTESIAN_POINT('Ctrl Pts',(-0.0135747082449835,-0.0348672023069664,
-0.0132831612932567));
#24522=CARTESIAN_POINT('Ctrl Pts',(-0.0136545150602694,-0.0348612326709022,
-0.0132040059324208));
#24523=CARTESIAN_POINT('Ctrl Pts',(-0.0137160212583936,-0.0348558698931575,
-0.0131304685845076));
#24524=CARTESIAN_POINT('Ctrl Pts',(-0.0138110048715943,-0.0348462834566206,
-0.0129927089973075));
#24525=CARTESIAN_POINT('Ctrl Pts',(-0.0138475318622819,-0.0348421281719534,
-0.0129309328142644));
#24526=CARTESIAN_POINT('Ctrl Pts',(-0.0138928827958914,-0.0348364036879076,
-0.0128403847166573));
#24527=CARTESIAN_POINT('Ctrl Pts',(-0.0139053702691509,-0.0348347505952777,
-0.0128135515545336));
#24528=CARTESIAN_POINT('Ctrl Pts',(-0.0139245957692367,-0.034832090178242,
-0.0127689273191175));
#24529=CARTESIAN_POINT('Ctrl Pts',(-0.0139317901106737,-0.0348310637794803,
-0.0127513418240695));
#24530=CARTESIAN_POINT('Ctrl Pts',(-0.0139412429097299,-0.0348296752538405,
-0.0127269603568708));
#24531=CARTESIAN_POINT('Ctrl Pts',(-0.013943781350078,-0.0348292980797765,
-0.0127202754985326));
#24532=CARTESIAN_POINT('Ctrl Pts',(-0.0139479936249754,-0.0348286650946708,
-0.0127089459912977));
#24533=CARTESIAN_POINT('Ctrl Pts',(-0.0139496917931445,-0.0348284078696832,
-0.0127043105478727));
#24534=CARTESIAN_POINT('Ctrl Pts',(-0.0139531438102045,-0.0348278808408587,
-0.0126947457982177));
#24535=CARTESIAN_POINT('Ctrl Pts',(-0.0139548948755508,-0.0348276111967017,
-0.0126898156144382));
#24536=CARTESIAN_POINT('Ctrl Pts',(-0.0139594391953792,-0.0348269050366806,
-0.0126768115897947));
#24537=CARTESIAN_POINT('Ctrl Pts',(-0.0139621905670056,-0.0348264709284387,
-0.0126687231869728));
#24538=CARTESIAN_POINT('Ctrl Pts',(-0.0139737160628962,-0.0348246219355165,
-0.0126338947237922));
#24539=CARTESIAN_POINT('Ctrl Pts',(-0.0139818253670753,-0.0348232419263447,
-0.0126069388390049));
#24540=CARTESIAN_POINT('Ctrl Pts',(-0.0140135310494007,-0.0348174170145163,
-0.0124900451124282));
#24541=CARTESIAN_POINT('Ctrl Pts',(-0.0140297109697846,-0.0348132365962009,
-0.0123982932890866));
#24542=CARTESIAN_POINT('Ctrl Pts',(-0.0140411772148268,-0.0348069865052287,
-0.0122624549177015));
#24543=CARTESIAN_POINT('Ctrl Pts',(-0.0140430000010343,-0.0348049870032333,
-0.0122191549896209));
#24544=CARTESIAN_POINT('Ctrl Pts',(-0.014043,-0.0348029487975611,-0.0121758532497038));
#24545=CARTESIAN_POINT('',(-0.0140429998634136,-0.0354166912456805,-0.0121752040518626));
#24546=CARTESIAN_POINT('Ctrl Pts',(-0.014043,-0.0349189332996453,-0.012175853287569));
#24547=CARTESIAN_POINT('Ctrl Pts',(-0.0140429999999959,-0.0349192278748801,
-0.0121821541091974));
#24548=CARTESIAN_POINT('Ctrl Pts',(-0.0140429614060005,-0.0349195216032071,
-0.0121884553538268));
#24549=CARTESIAN_POINT('Ctrl Pts',(-0.014041484780039,-0.0349251257502518,
-0.0123089768072391));
#24550=CARTESIAN_POINT('Ctrl Pts',(-0.014027406816373,-0.0349302046700773,
-0.0124226862737504));
#24551=CARTESIAN_POINT('Ctrl Pts',(-0.0139904944307964,-0.0349377505488585,
-0.0125774624844816));
#24552=CARTESIAN_POINT('Ctrl Pts',(-0.0139781827078049,-0.0349399234980106,
-0.0126206442839973));
#24553=CARTESIAN_POINT('Ctrl Pts',(-0.0139594304292141,-0.0349428784164322,
-0.0126769738016862));
#24554=CARTESIAN_POINT('Ctrl Pts',(-0.0139546604213203,-0.0349436056922872,
-0.0126906561506721));
#24555=CARTESIAN_POINT('Ctrl Pts',(-0.0139465337035157,-0.0349448073080629,
-0.0127129516471389));
#24556=CARTESIAN_POINT('Ctrl Pts',(-0.0139432909845762,-0.0349452778305313,
-0.0127216055502295));
#24557=CARTESIAN_POINT('Ctrl Pts',(-0.0139368426242571,-0.0349461967441564,
-0.0127383549112451));
#24558=CARTESIAN_POINT('Ctrl Pts',(-0.0139336458089462,-0.0349466448238317,
-0.0127464534048471));
#24559=CARTESIAN_POINT('Ctrl Pts',(-0.0139259663413774,-0.034947704170217,
-0.0127654358001774));
#24560=CARTESIAN_POINT('Ctrl Pts',(-0.0139214273891821,-0.034948317332994,
-0.0127762962180796));
#24561=CARTESIAN_POINT('Ctrl Pts',(-0.0139058782018645,-0.0349503762370247,
-0.0128123363557482));
#24562=CARTESIAN_POINT('Ctrl Pts',(-0.0138943200499805,-0.0349518405603365,
-0.0128372727324749));
#24563=CARTESIAN_POINT('Ctrl Pts',(-0.0138361285420905,-0.0349589184051529,
-0.0129545071121626));
#24564=CARTESIAN_POINT('Ctrl Pts',(-0.0137809659904748,-0.0349648241834418,
-0.0130422608974412));
#24565=CARTESIAN_POINT('Ctrl Pts',(-0.0136661962118816,-0.0349755709059691,
-0.0131896560518137));
#24566=CARTESIAN_POINT('Ctrl Pts',(-0.0136096804700388,-0.0349803719604161,
-0.0132512234284747));
#24567=CARTESIAN_POINT('Ctrl Pts',(-0.0135379507941278,-0.0349856741910349,
-0.0133176555160852));
#24568=CARTESIAN_POINT('Ctrl Pts',(-0.0135273060148863,-0.0349864424581803,
-0.013327242257742));
#24569=CARTESIAN_POINT('Ctrl Pts',(-0.0135117531071228,-0.0349875364436436,
-0.0133408618483028));
#24570=CARTESIAN_POINT('Ctrl Pts',(-0.0135069514517016,-0.0349878703568017,
-0.0133450145566205));
#24571=CARTESIAN_POINT('Ctrl Pts',(-0.0134984409179205,-0.0349884552476121,
-0.0133522835638559));
#24572=CARTESIAN_POINT('Ctrl Pts',(-0.0134947427932698,-0.0349887071138764,
-0.0133554122046813));
#24573=CARTESIAN_POINT('Ctrl Pts',(-0.0134867521285533,-0.0349892463678287,
-0.0133621080588484));
#24574=CARTESIAN_POINT('Ctrl Pts',(-0.0134824549228922,-0.0349895333432447,
-0.0133656694380615));
#24575=CARTESIAN_POINT('Ctrl Pts',(-0.0134703436270403,-0.034990334012746,
-0.0133755965191546));
#24576=CARTESIAN_POINT('Ctrl Pts',(-0.0134624862230763,-0.0349908440360555,
-0.0133819091970804));
#24577=CARTESIAN_POINT('Ctrl Pts',(-0.0134091896442855,-0.0349942448185815,
-0.0134238753260312));
#24578=CARTESIAN_POINT('Ctrl Pts',(-0.0133618371648448,-0.0349969829915576,
-0.0134570335008771));
#24579=CARTESIAN_POINT('Ctrl Pts',(-0.0132315907913201,-0.0350040962160063,
-0.0135377402091237));
#24580=CARTESIAN_POINT('Ctrl Pts',(-0.0131459584125612,-0.0350083691588784,
-0.0135803814538955));
#24581=CARTESIAN_POINT('Ctrl Pts',(-0.0130018016638577,-0.0350155952728165,
-0.0136361747908962));
#24582=CARTESIAN_POINT('Ctrl Pts',(-0.0129454938790591,-0.0350184221681892,
-0.0136543248269263));
#24583=CARTESIAN_POINT('Ctrl Pts',(-0.0128730171721841,-0.0350221383638682,
-0.0136731695911866));
#24584=CARTESIAN_POINT('Ctrl Pts',(-0.0128576878572948,-0.0350229284737961,
-0.01367690535106));
#24585=CARTESIAN_POINT('Ctrl Pts',(-0.0128330231942587,-0.0350242073967137,
-0.0136825168686683));
#24586=CARTESIAN_POINT('Ctrl Pts',(-0.0128237228934832,-0.0350246913664161,
-0.0136845424793624));
#24587=CARTESIAN_POINT('Ctrl Pts',(-0.0128059709390309,-0.0350256186493354,
-0.0136882371636811));
#24588=CARTESIAN_POINT('Ctrl Pts',(-0.0127975228641939,-0.0350260614431616,
-0.0136899217620818));
#24589=CARTESIAN_POINT('Ctrl Pts',(-0.0127781253379242,-0.0350270817398846,
-0.0136936211344696));
#24590=CARTESIAN_POINT('Ctrl Pts',(-0.0127671673870795,-0.035027660743206,
-0.0136955883036771));
#24591=CARTESIAN_POINT('Ctrl Pts',(-0.0127327164854055,-0.035029489647266,
-0.0137013888087877));
#24592=CARTESIAN_POINT('Ctrl Pts',(-0.0127091563228732,-0.0350307529073,
-0.0137047970852208));
#24593=CARTESIAN_POINT('Ctrl Pts',(-0.0126535838033979,-0.0350337629107386,
-0.0137115278581568));
#24594=CARTESIAN_POINT('Ctrl Pts',(-0.0126215284635323,-0.0350355227270624,
-0.0137143964324962));
#24595=CARTESIAN_POINT('Ctrl Pts',(-0.0124947106963579,-0.0350425710299601,
-0.0137217571884371));
#24596=CARTESIAN_POINT('Ctrl Pts',(-0.0123997140466747,-0.0350480559704158,
-0.0137185090355401));
#24597=CARTESIAN_POINT('Ctrl Pts',(-0.0122351309786807,-0.0350575769048951,
-0.0136976099306512));
#24598=CARTESIAN_POINT('Ctrl Pts',(-0.0121653303295028,-0.0350616147864906,
-0.0136837978905335));
#24599=CARTESIAN_POINT('Ctrl Pts',(-0.0120866529293196,-0.0350659933987778,
-0.01366249449768));
#24600=CARTESIAN_POINT('Ctrl Pts',(-0.0120766081790851,-0.0350665490356654,
-0.0136596650229496));
#24601=CARTESIAN_POINT('Ctrl Pts',(-0.0120611021319024,-0.0350674006743878,
-0.0136551268884433));
#24602=CARTESIAN_POINT('Ctrl Pts',(-0.0120556205113603,-0.0350677005544777,
-0.0136534894393385));
#24603=CARTESIAN_POINT('Ctrl Pts',(-0.012045533926267,-0.0350682499957669,
-0.0136504152064394));
#24604=CARTESIAN_POINT('Ctrl Pts',(-0.0120409265519993,-0.0350685000410071,
-0.0136489873055105));
#24605=CARTESIAN_POINT('Ctrl Pts',(-0.0120303661320681,-0.0350690710863216,
-0.0136456601013735));
#24606=CARTESIAN_POINT('Ctrl Pts',(-0.0120244178638815,-0.0350693912335158,
-0.0136437462244846));
#24607=CARTESIAN_POINT('Ctrl Pts',(-0.0120057471240004,-0.035070391873913,
-0.0136376134410386));
#24608=CARTESIAN_POINT('Ctrl Pts',(-0.0119930675950396,-0.0350710651850754,
-0.0136332647639384));
#24609=CARTESIAN_POINT('Ctrl Pts',(-0.0119266660968784,-0.0350745660782618,
-0.0136095196918036));
#24610=CARTESIAN_POINT('Ctrl Pts',(-0.0118739907908064,-0.0350772568707838,
-0.0135873151821283));
#24611=CARTESIAN_POINT('Ctrl Pts',(-0.0116959210881877,-0.0350864258207977,
-0.0135003170642539));
#24612=CARTESIAN_POINT('Ctrl Pts',(-0.0115782757134133,-0.0350926835113507,
-0.0134213137138952));
#24613=CARTESIAN_POINT('Ctrl Pts',(-0.01145758237785,-0.035100626472104,
-0.0133136762919159));
#24614=CARTESIAN_POINT('Ctrl Pts',(-0.0114424441622214,-0.0351016528845517,
-0.0132996198503045));
#24615=CARTESIAN_POINT('Ctrl Pts',(-0.0114199215459087,-0.0351032290829109,
-0.0132778484672597));
#24616=CARTESIAN_POINT('Ctrl Pts',(-0.01141232723575,-0.0351037693533707,
-0.0132703535358799));
#24617=CARTESIAN_POINT('Ctrl Pts',(-0.0113987764453279,-0.0351047497196259,
-0.013256699750894));
#24618=CARTESIAN_POINT('Ctrl Pts',(-0.0113927923334941,-0.0351051885599997,
-0.0132505688657363));
#24619=CARTESIAN_POINT('Ctrl Pts',(-0.0113800740682142,-0.035106134168763,
-0.0132373196875376));
#24620=CARTESIAN_POINT('Ctrl Pts',(-0.0113733560675464,-0.0351066416109347,
-0.0132301864675762));
#24621=CARTESIAN_POINT('Ctrl Pts',(-0.0113551126602553,-0.0351080419031602,
-0.0132104420193764));
#24622=CARTESIAN_POINT('Ctrl Pts',(-0.0113437282836082,-0.035108940681098,
-0.0131977028610675));
#24623=CARTESIAN_POINT('Ctrl Pts',(-0.0112615186880988,-0.0351156199649834,
-0.013102576870036));
#24624=CARTESIAN_POINT('Ctrl Pts',(-0.0111993705232442,-0.0351217599111498,
-0.0130131158575664));
#24625=CARTESIAN_POINT('Ctrl Pts',(-0.0111013513515596,-0.0351334747941228,
-0.0128344092911922));
#24626=CARTESIAN_POINT('Ctrl Pts',(-0.011063386164316,-0.0351389916492257,
-0.0127468673381362));
#24627=CARTESIAN_POINT('Ctrl Pts',(-0.0110294001501643,-0.035144904557628,
-0.0126431631692948));
#24628=CARTESIAN_POINT('Ctrl Pts',(-0.0110252474810955,-0.0351456499822229,
-0.0126298879540799));
#24629=CARTESIAN_POINT('Ctrl Pts',(-0.0110194827658824,-0.0351467176415384,
-0.0126105452276401));
#24630=CARTESIAN_POINT('Ctrl Pts',(-0.0110177274486277,-0.0351470475529177,
-0.0126045215152663));
#24631=CARTESIAN_POINT('Ctrl Pts',(-0.0110146844059113,-0.0351476279859805,
-0.0125938365025539));
#24632=CARTESIAN_POINT('Ctrl Pts',(-0.0110133817824504,-0.0351478793500546,
-0.0125891796227748));
#24633=CARTESIAN_POINT('Ctrl Pts',(-0.0110106101979945,-0.035148420513058,
-0.0125790885809712));
#24634=CARTESIAN_POINT('Ctrl Pts',(-0.0110091490643315,-0.0351487098659902,
-0.0125736524501426));
#24635=CARTESIAN_POINT('Ctrl Pts',(-0.0110050978289862,-0.0351495241837776,
-0.0125582439917753));
#24636=CARTESIAN_POINT('Ctrl Pts',(-0.0110025777692413,-0.0351500452738054,
-0.0125482533752353));
#24637=CARTESIAN_POINT('Ctrl Pts',(-0.0109848017237453,-0.0351538369924973,
-0.0124746816727093));
#24638=CARTESIAN_POINT('Ctrl Pts',(-0.0109734993320685,-0.0351569117924867,
-0.0124102068762238));
#24639=CARTESIAN_POINT('Ctrl Pts',(-0.0109550633142776,-0.0351646666328646,
-0.0122432461221478));
#24640=CARTESIAN_POINT('Ctrl Pts',(-0.0109540000424025,-0.0351692610412371,
-0.0121404227228415));
#24641=CARTESIAN_POINT('Ctrl Pts',(-0.0109672701340439,-0.0351763072216525,
-0.0119922088521544));
#24642=CARTESIAN_POINT('Ctrl Pts',(-0.0109734595736708,-0.0351785425438435,
-0.0119463756987252));
#24643=CARTESIAN_POINT('Ctrl Pts',(-0.0109843050854499,-0.0351815706909719,
-0.0118864881278773));
#24644=CARTESIAN_POINT('Ctrl Pts',(-0.0109871183260745,-0.0351823052110926,
-0.011872122664027));
#24645=CARTESIAN_POINT('Ctrl Pts',(-0.0109920469091079,-0.0351835157210243,
-0.0118487256859834));
#24646=CARTESIAN_POINT('Ctrl Pts',(-0.0109940400868623,-0.0351839877799489,
-0.0118396692201924));
#24647=CARTESIAN_POINT('Ctrl Pts',(-0.0109980596333535,-0.0351849074789414,
-0.0118221589264326));
#24648=CARTESIAN_POINT('Ctrl Pts',(-0.011000076052585,-0.035185354782227,
-0.0118137031613598));
#24649=CARTESIAN_POINT('Ctrl Pts',(-0.0110049701676435,-0.0351864088082339,
-0.0117939222265011));
#24650=CARTESIAN_POINT('Ctrl Pts',(-0.0110079052477468,-0.0351870173730948,
-0.011782611917395));
#24651=CARTESIAN_POINT('Ctrl Pts',(-0.011018037372148,-0.0351890441199869,
-0.0117453154597867));
#24652=CARTESIAN_POINT('Ctrl Pts',(-0.0110257868167337,-0.0351904800997411,
-0.0117194856524783));
#24653=CARTESIAN_POINT('Ctrl Pts',(-0.0110460925637809,-0.035193992795591,
-0.0116577320933375));
#24654=CARTESIAN_POINT('Ctrl Pts',(-0.011059308314014,-0.035196089284498,
-0.0116220450534919));
#24655=CARTESIAN_POINT('Ctrl Pts',(-0.0111198453258141,-0.0352049649548892,
-0.0114754563411682));
#24656=CARTESIAN_POINT('Ctrl Pts',(-0.0111787567257122,-0.0352120470701014,
-0.0113698164392069));
#24657=CARTESIAN_POINT('Ctrl Pts',(-0.0112710303650416,-0.0352208989449371,
-0.0112421232346664));
#24658=CARTESIAN_POINT('Ctrl Pts',(-0.0112937761695284,-0.0352229423963625,
-0.0112129188984447));
#24659=CARTESIAN_POINT('Ctrl Pts',(-0.0113235723120526,-0.0352254249107107,
-0.0111773770868772));
#24660=CARTESIAN_POINT('Ctrl Pts',(-0.0113296584923796,-0.0352259224642264,
-0.011170250188713));
#24661=CARTESIAN_POINT('Ctrl Pts',(-0.0113393717949308,-0.0352267010280163,
-0.0111590835815567));
#24662=CARTESIAN_POINT('Ctrl Pts',(-0.0113429558569228,-0.0352269850458421,
-0.0111550069140975));
#24663=CARTESIAN_POINT('Ctrl Pts',(-0.0113498048887272,-0.0352275214898538,
-0.0111472989367761));
#24664=CARTESIAN_POINT('Ctrl Pts',(-0.0113530656527687,-0.0352277741982832,
-0.0111436641334304));
#24665=CARTESIAN_POINT('Ctrl Pts',(-0.0113608726695489,-0.0352283730004217,
-0.0111350442537846));
#24666=CARTESIAN_POINT('Ctrl Pts',(-0.0113654345124865,-0.0352287179314594,
-0.0111300733501051));
#24667=CARTESIAN_POINT('Ctrl Pts',(-0.011381097972403,-0.0352298861196759,
-0.0111132284791137));
#24668=CARTESIAN_POINT('Ctrl Pts',(-0.0113923548849554,-0.0352306983474067,
-0.0111014997286535));
#24669=CARTESIAN_POINT('Ctrl Pts',(-0.0114205685227779,-0.0352326743002262,
-0.0110730184298032));
#24670=CARTESIAN_POINT('Ctrl Pts',(-0.0114377323623434,-0.0352338251371262,
-0.0110564764084946));
#24671=CARTESIAN_POINT('Ctrl Pts',(-0.0115145281002074,-0.0352387906107325,
-0.010985820762947));
#24672=CARTESIAN_POINT('Ctrl Pts',(-0.0115779624968361,-0.0352424291992976,
-0.0109360224433093));
#24673=CARTESIAN_POINT('Ctrl Pts',(-0.0117251191616811,-0.0352505241307344,
-0.0108380667512559));
#24674=CARTESIAN_POINT('Ctrl Pts',(-0.0118100502824741,-0.0352549921551669,
-0.0107923504942044));
#24675=CARTESIAN_POINT('Ctrl Pts',(-0.0119141253550243,-0.0352605857024441,
-0.0107483095134318));
#24676=CARTESIAN_POINT('Ctrl Pts',(-0.0119296771278133,-0.0352614239192091,
-0.0107420255013818));
#24677=CARTESIAN_POINT('Ctrl Pts',(-0.0119544985938413,-0.0352627668352553,
-0.0107324635960763));
#24678=CARTESIAN_POINT('Ctrl Pts',(-0.0119637027052372,-0.0352632658933655,
-0.0107290185383925));
#24679=CARTESIAN_POINT('Ctrl Pts',(-0.0119809879928628,-0.0352642053984294,
-0.0107227363328822));
#24680=CARTESIAN_POINT('Ctrl Pts',(-0.0119890611271197,-0.03526464511637,
-0.0107198780776865));
#24681=CARTESIAN_POINT('Ctrl Pts',(-0.0120072063384381,-0.0352656356422503,
-0.0107136233511478));
#24682=CARTESIAN_POINT('Ctrl Pts',(-0.0120172904929665,-0.0352661876429202,
-0.0107102634731803));
#24683=CARTESIAN_POINT('Ctrl Pts',(-0.0120475281325399,-0.0352678476598518,
-0.0107005347046513));
#24684=CARTESIAN_POINT('Ctrl Pts',(-0.0120677780318011,-0.0352689657604726,
-0.010694475610447));
#24685=CARTESIAN_POINT('Ctrl Pts',(-0.0121649566631374,-0.0352743635739593,
-0.010667560366849));
#24686=CARTESIAN_POINT('Ctrl Pts',(-0.0122432914515529,-0.0352788187375334,
-0.0106522721270687));
#24687=CARTESIAN_POINT('Ctrl Pts',(-0.0124065346341412,-0.0352882018671932,
-0.0106333622253194));
#24688=CARTESIAN_POINT('Ctrl Pts',(-0.0124912793349515,-0.0352931262060502,
-0.0106305577064839));
#24689=CARTESIAN_POINT('Ctrl Pts',(-0.0126154323267523,-0.0353001288900669,
-0.0106366662222009));
#24690=CARTESIAN_POINT('Ctrl Pts',(-0.0126549517083395,-0.0353023243949546,
-0.0106401411136288));
#24691=CARTESIAN_POINT('Ctrl Pts',(-0.0127037679935924,-0.0353049597878984,
-0.0106463374253121));
#24692=CARTESIAN_POINT('Ctrl Pts',(-0.0127132289046396,-0.0353054669332946,
-0.0106476276460621));
#24693=CARTESIAN_POINT('Ctrl Pts',(-0.0127280867004815,-0.0353062570289947,
-0.0106497945264506));
#24694=CARTESIAN_POINT('Ctrl Pts',(-0.012733491793894,-0.0353065431320929,
-0.0106506121691469));
#24695=CARTESIAN_POINT('Ctrl Pts',(-0.0127437050289793,-0.0353070810823052,
-0.0106522127160859));
#24696=CARTESIAN_POINT('Ctrl Pts',(-0.0127485139094776,-0.0353073332398516,
-0.0106529896793348));
#24697=CARTESIAN_POINT('Ctrl Pts',(-0.0127598957869477,-0.0353079274855676,
-0.010654883980213));
#24698=CARTESIAN_POINT('Ctrl Pts',(-0.0127664654294669,-0.035308268461373,
-0.0106560211810382));
#24699=CARTESIAN_POINT('Ctrl Pts',(-0.0127885528853254,-0.035309408632534,
-0.0106599921262914));
#24700=CARTESIAN_POINT('Ctrl Pts',(-0.0128040350168475,-0.0353101975013507,
-0.0106630213164853));
#24701=CARTESIAN_POINT('Ctrl Pts',(-0.0128418563300488,-0.0353121051373797,
-0.0106710254189021));
#24702=CARTESIAN_POINT('Ctrl Pts',(-0.0128641368900721,-0.0353132121502159,
-0.0106762609847965));
#24703=CARTESIAN_POINT('Ctrl Pts',(-0.0129583190584852,-0.0353178505673233,
-0.0107006152743959));
#24704=CARTESIAN_POINT('Ctrl Pts',(-0.0130289072199716,-0.035321228262489,
-0.0107244257399117));
#24705=CARTESIAN_POINT('Ctrl Pts',(-0.013185720711164,-0.0353290055307256,
-0.0107902881063701));
#24706=CARTESIAN_POINT('Ctrl Pts',(-0.0132702936924813,-0.0353334137029007,
-0.0108354618222048));
#24707=CARTESIAN_POINT('Ctrl Pts',(-0.0133684374919634,-0.035339179324623,
-0.010900256788681));
#24708=CARTESIAN_POINT('Ctrl Pts',(-0.0133864817561702,-0.0353402679167725,
-0.0109127301181926));
#24709=CARTESIAN_POINT('Ctrl Pts',(-0.0134129913189206,-0.0353419134508962,
-0.0109319030709441));
#24710=CARTESIAN_POINT('Ctrl Pts',(-0.0134216625192168,-0.0353424592987653,
-0.0109383140021867));
#24711=CARTESIAN_POINT('Ctrl Pts',(-0.0134371083636149,-0.0353434456833796,
-0.0109499860526849));
#24712=CARTESIAN_POINT('Ctrl Pts',(-0.0134439077311533,-0.0353438848950614,
-0.0109552138019583));
#24713=CARTESIAN_POINT('Ctrl Pts',(-0.013458320403366,-0.0353448267868719,
-0.0109664875374962));
#24714=CARTESIAN_POINT('Ctrl Pts',(-0.0134659208347509,-0.0353453300899173,
-0.0109725493159497));
#24715=CARTESIAN_POINT('Ctrl Pts',(-0.0134864388355817,-0.0353467071232581,
-0.0109892332519152));
#24716=CARTESIAN_POINT('Ctrl Pts',(-0.0134992415538547,-0.0353475864587699,
-0.0109999940389266));
#24717=CARTESIAN_POINT('Ctrl Pts',(-0.0135785132529602,-0.0353531606049416,
-0.0110688522031373));
#24718=CARTESIAN_POINT('Ctrl Pts',(-0.0136400596206086,-0.0353580851422487,
-0.011132348395693));
#24719=CARTESIAN_POINT('Ctrl Pts',(-0.0137504600378492,-0.0353680644443494,
-0.0112677396009183));
#24720=CARTESIAN_POINT('Ctrl Pts',(-0.0137993595571494,-0.0353730947626295,
-0.0113392018376263));
#24721=CARTESIAN_POINT('Ctrl Pts',(-0.0138603335630965,-0.0353800376867678,
-0.0114466626058166));
#24722=CARTESIAN_POINT('Ctrl Pts',(-0.0138774801042879,-0.0353820875318691,
-0.0114795951385183));
#24723=CARTESIAN_POINT('Ctrl Pts',(-0.0138974519739828,-0.0353845765205087,
-0.011521586553736));
#24724=CARTESIAN_POINT('Ctrl Pts',(-0.0139014034144621,-0.0353850745115089,
-0.0115300936905956));
#24725=CARTESIAN_POINT('Ctrl Pts',(-0.0139075194814681,-0.0353858536018432,
-0.0115435816741634));
#24726=CARTESIAN_POINT('Ctrl Pts',(-0.0139097357492781,-0.035386137715287,
-0.0115485386912028));
#24727=CARTESIAN_POINT('Ctrl Pts',(-0.0139138951485842,-0.0353866742301261,
-0.0115579751850743));
#24728=CARTESIAN_POINT('Ctrl Pts',(-0.0139158432281681,-0.0353869269150386,
-0.0115624522815244));
#24729=CARTESIAN_POINT('Ctrl Pts',(-0.0139204310632585,-0.0353875255113124,
-0.0115731343940845));
#24730=CARTESIAN_POINT('Ctrl Pts',(-0.0139230514831374,-0.035387870262338,
-0.0115793476718229));
#24731=CARTESIAN_POINT('Ctrl Pts',(-0.0139318409212051,-0.0353890371443356,
-0.0116005758981555));
#24732=CARTESIAN_POINT('Ctrl Pts',(-0.0139378138853745,-0.0353898482794882,
-0.0116156713807252));
#24733=CARTESIAN_POINT('Ctrl Pts',(-0.0139519499788152,-0.0353918210174683,
-0.0116531141961429));
#24734=CARTESIAN_POINT('Ctrl Pts',(-0.013959836780341,-0.0353929697871273,
-0.0116755618057165));
#24735=CARTESIAN_POINT('Ctrl Pts',(-0.0140173505844951,-0.0354018108256075,
-0.0118522202099648));
#24736=CARTESIAN_POINT('Ctrl Pts',(-0.0140429316914556,-0.0354088077580484,
-0.0120131835640155));
#24737=CARTESIAN_POINT('Ctrl Pts',(-0.0140429998634136,-0.0354166912456806,
-0.0121752040518639));
#24738=CARTESIAN_POINT('Ctrl Pts',(-0.0140429998634136,-0.0354166912456805,
-0.0121752040518624));
#24739=CARTESIAN_POINT('Ctrl Pts',(-0.0140429999558722,-0.035416701937705,
-0.0121754237930612));
#24740=CARTESIAN_POINT('Ctrl Pts',(-0.014043,-0.0354167121449367,-0.012175633545861));
#24741=CARTESIAN_POINT('Ctrl Pts',(-0.014043,-0.0354167228394876,-0.0121758532865585));
#24742=CARTESIAN_POINT('Origin',(-0.0125,-0.0375520664398416,-0.0121758532865581));
#24743=CARTESIAN_POINT('',(-0.014043,-0.0359172995678105,-0.0121758532865606));
#24744=CARTESIAN_POINT('',(-0.014043,-0.035802018678757,-0.0121758532865075));
#24745=CARTESIAN_POINT('',(-0.014043,-0.0375520664398416,-0.012175853286558));
#24746=CARTESIAN_POINT('',(-0.0140429999599998,-0.0353007391609988,-0.0121762046275615));
#24747=CARTESIAN_POINT('Ctrl Pts',(-0.014043,-0.035802018678757,-0.012175853286457));
#24748=CARTESIAN_POINT('Ctrl Pts',(-0.0140429999999942,-0.0357969039511853,
-0.0120869245163723));
#24749=CARTESIAN_POINT('Ctrl Pts',(-0.0140353120831769,-0.0357917698082273,
-0.0119981559031497));
#24750=CARTESIAN_POINT('Ctrl Pts',(-0.0140175842681859,-0.0357861805132807,
-0.0118965909125327));
#24751=CARTESIAN_POINT('Ctrl Pts',(-0.0140149576625064,-0.0357854213234747,
-0.0118826762184364));
#24752=CARTESIAN_POINT('Ctrl Pts',(-0.0140108854541471,-0.0357843386179533,
-0.0118626219404954));
#24753=CARTESIAN_POINT('Ctrl Pts',(-0.0140095932455082,-0.0357840071050992,
-0.0118564523354713));
#24754=CARTESIAN_POINT('Ctrl Pts',(-0.0140072460029681,-0.0357834257958607,
-0.0118455780520453));
#24755=CARTESIAN_POINT('Ctrl Pts',(-0.0140062066735373,-0.0357831751292779,
-0.0118408701486142));
#24756=CARTESIAN_POINT('Ctrl Pts',(-0.0140039198885508,-0.0357826378450967,
-0.0118307374355294));
#24757=CARTESIAN_POINT('Ctrl Pts',(-0.0140026651343067,-0.0357823516428319,
-0.0118253144472818));
#24758=CARTESIAN_POINT('Ctrl Pts',(-0.0139990564962871,-0.0357815518511041,
-0.0118100935887655));
#24759=CARTESIAN_POINT('Ctrl Pts',(-0.0139966359028222,-0.035781041938553,
-0.0118003116508037));
#24760=CARTESIAN_POINT('Ctrl Pts',(-0.0139794992746883,-0.0357776015109178,
-0.0117338589862703));
#24761=CARTESIAN_POINT('Ctrl Pts',(-0.0139616623912841,-0.0357748279314554,
-0.0116780366703213));
#24762=CARTESIAN_POINT('Ctrl Pts',(-0.0139062743513583,-0.0357676511346147,
-0.0115336058452449));
#24763=CARTESIAN_POINT('Ctrl Pts',(-0.0138635433588903,-0.0357633483770738,
-0.0114472660511692));
#24764=CARTESIAN_POINT('Ctrl Pts',(-0.0137826698329396,-0.0357561417055771,
-0.0113162287481834));
#24765=CARTESIAN_POINT('Ctrl Pts',(-0.0137495414647113,-0.0357533721258981,
-0.0112687471686669));
#24766=CARTESIAN_POINT('Ctrl Pts',(-0.0137041572123496,-0.0357497232978149,
-0.0112109181841473));
#24767=CARTESIAN_POINT('Ctrl Pts',(-0.0136943001222839,-0.0357489387544438,
-0.0111987445213389));
#24768=CARTESIAN_POINT('Ctrl Pts',(-0.0136781904338011,-0.0357476680119432,
-0.0111794568098598));
#24769=CARTESIAN_POINT('Ctrl Pts',(-0.0136720545768633,-0.0357471865762327,
-0.0111722464408795));
#24770=CARTESIAN_POINT('Ctrl Pts',(-0.0136602328312253,-0.0357462636257307,
-0.0111586107477681));
#24771=CARTESIAN_POINT('Ctrl Pts',(-0.0136545589341768,-0.0357458226191196,
-0.0111521754715607));
#24772=CARTESIAN_POINT('Ctrl Pts',(-0.013641420283427,-0.0357448057215296,
-0.0111375219362815));
#24773=CARTESIAN_POINT('Ctrl Pts',(-0.0136339199665133,-0.0357442283325195,
-0.0111293363219425));
#24774=CARTESIAN_POINT('Ctrl Pts',(-0.0136100729922263,-0.0357424018719868,
-0.0111038678190353));
#24775=CARTESIAN_POINT('Ctrl Pts',(-0.0135934151578517,-0.0357411394408294,
-0.0110868821675252));
#24776=CARTESIAN_POINT('Ctrl Pts',(-0.0135533121968993,-0.0357381300090292,
-0.0110478381235019));
#24777=CARTESIAN_POINT('Ctrl Pts',(-0.0135295568871957,-0.0357363699005796,
-0.0110261153977616));
#24778=CARTESIAN_POINT('Ctrl Pts',(-0.0134330285084361,-0.0357293110005793,
-0.0109432380339284));
#24779=CARTESIAN_POINT('Ctrl Pts',(-0.0133553543197461,-0.0357238147747226,
-0.0108881232248371));
#24780=CARTESIAN_POINT('Ctrl Pts',(-0.0132117020613102,-0.0357142892220465,
-0.010804954074116));
#24781=CARTESIAN_POINT('Ctrl Pts',(-0.0131479053382555,-0.035710257547409,
-0.0107736746321215));
#24782=CARTESIAN_POINT('Ctrl Pts',(-0.0130725396235192,-0.0357058862499264,
-0.0107429695942542));
#24783=CARTESIAN_POINT('Ctrl Pts',(-0.0130628624889502,-0.0357053321656911,
-0.0107391406756869));
#24784=CARTESIAN_POINT('Ctrl Pts',(-0.0130478259484627,-0.0357044831574408,
-0.01073336646848));
#24785=CARTESIAN_POINT('Ctrl Pts',(-0.0130424934253114,-0.0357041843724694,
-0.0107313525507736));
#24786=CARTESIAN_POINT('Ctrl Pts',(-0.0130326481964725,-0.0357036371428417,
-0.0107276965417633));
#24787=CARTESIAN_POINT('Ctrl Pts',(-0.0130281389472009,-0.0357033882152627,
-0.010726045950438));
#24788=CARTESIAN_POINT('Ctrl Pts',(-0.0130177780869906,-0.0357028201148599,
-0.0107223081558072));
#24789=CARTESIAN_POINT('Ctrl Pts',(-0.0130119215159286,-0.0357025017821357,
-0.0107202352189984));
#24790=CARTESIAN_POINT('Ctrl Pts',(-0.0129934923365365,-0.035701508350312,
-0.0107138371836837));
#24791=CARTESIAN_POINT('Ctrl Pts',(-0.012980875950078,-0.035700840313235,
-0.0107096390749429));
#24792=CARTESIAN_POINT('Ctrl Pts',(-0.0129145144581758,-0.0356973817815611,
-0.010688505998918));
#24793=CARTESIAN_POINT('Ctrl Pts',(-0.0128599213965291,-0.0356947246143362,
-0.0106743600863118));
#24794=CARTESIAN_POINT('Ctrl Pts',(-0.0127079168213646,-0.0356875463643613,
-0.0106437432627425));
#24795=CARTESIAN_POINT('Ctrl Pts',(-0.0126095157178928,-0.0356831282475872,
-0.0106335831483342));
#24796=CARTESIAN_POINT('Ctrl Pts',(-0.0124577272187848,-0.0356759918334553,
-0.0106325190068169));
#24797=CARTESIAN_POINT('Ctrl Pts',(-0.0124046574529035,-0.035673439853699,
-0.0106348870995712));
#24798=CARTESIAN_POINT('Ctrl Pts',(-0.0123366432010291,-0.0356700450042746,
-0.0106414491754506));
#24799=CARTESIAN_POINT('Ctrl Pts',(-0.0123214912351247,-0.0356692808543534,
-0.0106431380423654));
#24800=CARTESIAN_POINT('Ctrl Pts',(-0.0122970638029911,-0.0356680352380575,
-0.0106462278957082));
#24801=CARTESIAN_POINT('Ctrl Pts',(-0.012287771554196,-0.0356675581945331,
-0.0106474894496113));
#24802=CARTESIAN_POINT('Ctrl Pts',(-0.0122699770666586,-0.0356666382926994,
-0.0106500707098385));
#24803=CARTESIAN_POINT('Ctrl Pts',(-0.0122614732176514,-0.0356661958777746,
-0.0106513769858636));
#24804=CARTESIAN_POINT('Ctrl Pts',(-0.0122418396092341,-0.0356651677907679,
-0.0106545612025663));
#24805=CARTESIAN_POINT('Ctrl Pts',(-0.0122307187373199,-0.0356645805074265,
-0.010656490267197));
#24806=CARTESIAN_POINT('Ctrl Pts',(-0.0121952144602948,-0.0356626893136001,
-0.0106630510010518));
#24807=CARTESIAN_POINT('Ctrl Pts',(-0.0121709220996311,-0.0356613706630401,
-0.0106681488662015));
#24808=CARTESIAN_POINT('Ctrl Pts',(-0.0120493794043543,-0.035654646179712,
-0.0106967324722927));
#24809=CARTESIAN_POINT('Ctrl Pts',(-0.0119544652589708,-0.0356489609153181,
-0.0107290484677886));
#24810=CARTESIAN_POINT('Ctrl Pts',(-0.0117803691321364,-0.0356379703138455,
-0.0108079056507223));
#24811=CARTESIAN_POINT('Ctrl Pts',(-0.0117008662078673,-0.0356327038727902,
-0.0108527747752512));
#24812=CARTESIAN_POINT('Ctrl Pts',(-0.0116153408069296,-0.0356270786123029,
-0.0109115796960468));
#24813=CARTESIAN_POINT('Ctrl Pts',(-0.0116049867755636,-0.0356263985281629,
-0.0109188883119078));
#24814=CARTESIAN_POINT('Ctrl Pts',(-0.0115896934242431,-0.0356253968597755,
-0.0109299682506319));
#24815=CARTESIAN_POINT('Ctrl Pts',(-0.0115846851647509,-0.03562506929708,
-0.0109336430227286));
#24816=CARTESIAN_POINT('Ctrl Pts',(-0.0115760916967042,-0.0356245082482817,
-0.0109400286038204));
#24817=CARTESIAN_POINT('Ctrl Pts',(-0.0115724959260372,-0.0356242737941744,
-0.0109427249910546));
#24818=CARTESIAN_POINT('Ctrl Pts',(-0.011564903393968,-0.0356237794848083,
-0.0109484704582584));
#24819=CARTESIAN_POINT('Ctrl Pts',(-0.0115609096511328,-0.0356235199187744,
-0.0109515234341272));
#24820=CARTESIAN_POINT('Ctrl Pts',(-0.0115509148455304,-0.0356228712518423,
-0.0109592415391782));
#24821=CARTESIAN_POINT('Ctrl Pts',(-0.0115449331246344,-0.0356224838824401,
-0.0109639316544165));
#24822=CARTESIAN_POINT('Ctrl Pts',(-0.0115214987256851,-0.03562096858775,
-0.0109825872341537));
#24823=CARTESIAN_POINT('Ctrl Pts',(-0.011504314973799,-0.0356198625128401,
-0.0109968876210711));
#24824=CARTESIAN_POINT('Ctrl Pts',(-0.0114592437712256,-0.0356169568934583,
-0.0110360846639483));
#24825=CARTESIAN_POINT('Ctrl Pts',(-0.0114319393593185,-0.0356151917118042,
-0.0110616303313854));
#24826=CARTESIAN_POINT('Ctrl Pts',(-0.0113262129776787,-0.0356082136566246,
-0.0111680081443195));
#24827=CARTESIAN_POINT('Ctrl Pts',(-0.0112558188348658,-0.0356032060506992,
-0.0112563197107745));
#24828=CARTESIAN_POINT('Ctrl Pts',(-0.0111705938449963,-0.035595657845881,
-0.0113911688753597));
#24829=CARTESIAN_POINT('Ctrl Pts',(-0.0111473514117971,-0.0355933904449234,
-0.0114319503066239));
#24830=CARTESIAN_POINT('Ctrl Pts',(-0.0111193267175715,-0.0355903265330415,
-0.0114867918859883));
#24831=CARTESIAN_POINT('Ctrl Pts',(-0.0111128363343671,-0.035589590268226,
-0.0114999529444264));
#24832=CARTESIAN_POINT('Ctrl Pts',(-0.0111025602892601,-0.0355883789456883,
-0.0115215621395346));
#24833=CARTESIAN_POINT('Ctrl Pts',(-0.011098661128386,-0.0355879078610364,
-0.011529955452356));
#24834=CARTESIAN_POINT('Ctrl Pts',(-0.011091265594989,-0.0355869915607104,
-0.0115462572753471));
#24835=CARTESIAN_POINT('Ctrl Pts',(-0.0110877597246949,-0.0355865466957615,
-0.0115541611103725));
#24836=CARTESIAN_POINT('Ctrl Pts',(-0.0110797155400832,-0.0355855007956478,
-0.0115727155914201));
#24837=CARTESIAN_POINT('Ctrl Pts',(-0.0110752303385841,-0.0355848979699681,
-0.0115833885800852));
#24838=CARTESIAN_POINT('Ctrl Pts',(-0.0110608758472488,-0.0355829018932249,
-0.0116186524590689));
#24839=CARTESIAN_POINT('Ctrl Pts',(-0.0110515202176966,-0.035581491517141,
-0.0116434462127955));
#24840=CARTESIAN_POINT('Ctrl Pts',(-0.0110305784778562,-0.0355780527125094,
-0.011703590075391));
#24841=CARTESIAN_POINT('Ctrl Pts',(-0.0110196235604196,-0.035576005540787,
-0.0117391411899085));
#24842=CARTESIAN_POINT('Ctrl Pts',(-0.0109926936782248,-0.0355702105554153,
-0.011839256749101));
#24843=CARTESIAN_POINT('Ctrl Pts',(-0.0109795921172323,-0.0355663966691419,
-0.0119045075947239));
#24844=CARTESIAN_POINT('Ctrl Pts',(-0.0109594743588605,-0.0355577051302924,
-0.0120542479737002));
#24845=CARTESIAN_POINT('Ctrl Pts',(-0.0109551236424415,-0.0355528331275439,
-0.0121388908996066));
#24846=CARTESIAN_POINT('Ctrl Pts',(-0.0109581753140536,-0.035547470599006,
-0.0122377352119439));
#24847=CARTESIAN_POINT('Ctrl Pts',(-0.0109588137371642,-0.0355467051249706,
-0.0122519956968508));
#24848=CARTESIAN_POINT('Ctrl Pts',(-0.0109600204030318,-0.035545615202657,
-0.0122725581161415));
#24849=CARTESIAN_POINT('Ctrl Pts',(-0.0109604296369369,-0.0355452826126924,
-0.0122788682518567));
#24850=CARTESIAN_POINT('Ctrl Pts',(-0.010961219392323,-0.0355447001101853,
-0.0122899870060016));
#24851=CARTESIAN_POINT('Ctrl Pts',(-0.0109615836874813,-0.0355444493149205,
-0.0122947966175866));
#24852=CARTESIAN_POINT('Ctrl Pts',(-0.0109624159173361,-0.0355439125552217,
-0.0123051398915939));
#24853=CARTESIAN_POINT('Ctrl Pts',(-0.0109628911751381,-0.0355436269971503,
-0.0123106727952155));
#24854=CARTESIAN_POINT('Ctrl Pts',(-0.0109643073634688,-0.0355428308784808,
-0.012326177769754));
#24855=CARTESIAN_POINT('Ctrl Pts',(-0.0109653155522594,-0.0355423239408678,
-0.0123361435858477));
#24856=CARTESIAN_POINT('Ctrl Pts',(-0.0109726862327671,-0.0355389742721936,
-0.0124025388817137));
#24857=CARTESIAN_POINT('Ctrl Pts',(-0.0109820632692576,-0.0355362791101029,
-0.0124585951352789));
#24858=CARTESIAN_POINT('Ctrl Pts',(-0.0110203320101982,-0.0355281658738612,
-0.0126289687648708));
#24859=CARTESIAN_POINT('Ctrl Pts',(-0.0110592340137502,-0.0355229309491022,
-0.0127405879390835));
#24860=CARTESIAN_POINT('Ctrl Pts',(-0.0111284041509055,-0.0355153537855548,
-0.0128838626344016));
#24861=CARTESIAN_POINT('Ctrl Pts',(-0.0111478308226674,-0.0355133490449166,
-0.0129202930553938));
#24862=CARTESIAN_POINT('Ctrl Pts',(-0.0111758023790196,-0.0355105923519372,
-0.0129680321832902));
#24863=CARTESIAN_POINT('Ctrl Pts',(-0.0111830767039385,-0.0355098859813953,
-0.01298006703893));
#24864=CARTESIAN_POINT('Ctrl Pts',(-0.0111953405075296,-0.0355087113334865,
-0.0129997439717324));
#24865=CARTESIAN_POINT('Ctrl Pts',(-0.0112002351783702,-0.0355082465677578,
-0.0130074443255663));
#24866=CARTESIAN_POINT('Ctrl Pts',(-0.0112099335575592,-0.0355073332891935,
-0.0130224071154273));
#24867=CARTESIAN_POINT('Ctrl Pts',(-0.0112147310176271,-0.0355068850215266,
-0.0130296732030951));
#24868=CARTESIAN_POINT('Ctrl Pts',(-0.0112262558779372,-0.0355058161847234,
-0.0130468111597219));
#24869=CARTESIAN_POINT('Ctrl Pts',(-0.0112330368650322,-0.0355051935931092,
-0.0130566461731665));
#24870=CARTESIAN_POINT('Ctrl Pts',(-0.0112565252736293,-0.0355030576417126,
-0.0130898807772476));
#24871=CARTESIAN_POINT('Ctrl Pts',(-0.0112737714947859,-0.0355015236816646,
-0.0131128907204594));
#24872=CARTESIAN_POINT('Ctrl Pts',(-0.0113175172855969,-0.0354977125856331,
-0.0131679792242129));
#24873=CARTESIAN_POINT('Ctrl Pts',(-0.0113446898662361,-0.0354954108714996,
-0.013199492551242));
#24874=CARTESIAN_POINT('Ctrl Pts',(-0.0114188087639352,-0.0354893111225179,
-0.0132787367259381));
#24875=CARTESIAN_POINT('Ctrl Pts',(-0.0114676452390555,-0.0354854589165813,
-0.0133245783195241));
#24876=CARTESIAN_POINT('Ctrl Pts',(-0.0115329903724915,-0.035480591339684,
-0.0133783739068904));
#24877=CARTESIAN_POINT('Ctrl Pts',(-0.0115468742989383,-0.035479572469939,
-0.013389407928267));
#24878=CARTESIAN_POINT('Ctrl Pts',(-0.0116123473635524,-0.0354748470711335,
-0.0134396247242715));
#24879=CARTESIAN_POINT('Ctrl Pts',(-0.0116661860400421,-0.0354711834050243,
-0.0134757768415772));
#24880=CARTESIAN_POINT('Ctrl Pts',(-0.011731094231683,-0.0354671468820992,
-0.0135136650672111));
#24881=CARTESIAN_POINT('Ctrl Pts',(-0.0117400987833732,-0.0354665950421411,
-0.0135188002674091));
#24882=CARTESIAN_POINT('Ctrl Pts',(-0.0117541263285647,-0.0354657487326962,
-0.0135266137586506));
#24883=CARTESIAN_POINT('Ctrl Pts',(-0.0117591133854929,-0.0354654504392737,
-0.0135293555633174));
#24884=CARTESIAN_POINT('Ctrl Pts',(-0.011768337141258,-0.0354649036533949,
-0.0135343603824996));
#24885=CARTESIAN_POINT('Ctrl Pts',(-0.0117725692703024,-0.0354646546842331,
-0.0135366312268464));
#24886=CARTESIAN_POINT('Ctrl Pts',(-0.0117823110393535,-0.0354640859098827,
-0.0135417999569554));
#24887=CARTESIAN_POINT('Ctrl Pts',(-0.0117878276699755,-0.0354637669526756,
-0.0135446842934925));
#24888=CARTESIAN_POINT('Ctrl Pts',(-0.0118052405366685,-0.0354627695423985,
-0.0135536547394338));
#24889=CARTESIAN_POINT('Ctrl Pts',(-0.0118171987489832,-0.0354620982320017,
-0.0135596198961374));
#24890=CARTESIAN_POINT('Ctrl Pts',(-0.0118805234644829,-0.0354586069941102,
-0.0135901875755987));
#24891=CARTESIAN_POINT('Ctrl Pts',(-0.0119331495835205,-0.0354559231943394,
-0.0136120894594758));
#24892=CARTESIAN_POINT('Ctrl Pts',(-0.0120805363248874,-0.0354486917767345,
-0.0136640614326879));
#24893=CARTESIAN_POINT('Ctrl Pts',(-0.012177170877928,-0.0354442456487917,
-0.0136879693251362));
#24894=CARTESIAN_POINT('Ctrl Pts',(-0.0123266286244941,-0.0354371353458193,
-0.0137099553001116));
#24895=CARTESIAN_POINT('Ctrl Pts',(-0.0123781659979896,-0.0354346458527557,
-0.0137149057378052));
#24896=CARTESIAN_POINT('Ctrl Pts',(-0.0124450920885785,-0.0354313173935996,
-0.013717951488272));
#24897=CARTESIAN_POINT('Ctrl Pts',(-0.0124603412969363,-0.0354305527272303,
-0.0137184189767821));
#24898=CARTESIAN_POINT('Ctrl Pts',(-0.0124849732334615,-0.0354293064703981,
-0.0137188086252244));
#24899=CARTESIAN_POINT('Ctrl Pts',(-0.0124943528870484,-0.0354288293111643,
-0.0137188714607378));
#24900=CARTESIAN_POINT('Ctrl Pts',(-0.0125123353986931,-0.0354279093235751,
-0.0137188279623061));
#24901=CARTESIAN_POINT('Ctrl Pts',(-0.0125209379551196,-0.0354274669402418,
-0.0137187352036501));
#24902=CARTESIAN_POINT('Ctrl Pts',(-0.0125408192668135,-0.0354264391310958,
-0.0137183545263135));
#24903=CARTESIAN_POINT('Ctrl Pts',(-0.0125520964428259,-0.0354258520969612,
-0.0137180148340955));
#24904=CARTESIAN_POINT('Ctrl Pts',(-0.0125881398599833,-0.0354239625815609,
-0.0137165333354301));
#24905=CARTESIAN_POINT('Ctrl Pts',(-0.0126128818459542,-0.03542264539729,
-0.0137149183405773));
#24906=CARTESIAN_POINT('Ctrl Pts',(-0.012729021647587,-0.0354163657331576,
-0.0137045219568074));
#24907=CARTESIAN_POINT('Ctrl Pts',(-0.0128195454793205,-0.0354111728501523,
-0.0136881910773662));
#24908=CARTESIAN_POINT('Ctrl Pts',(-0.0130047128766322,-0.0354001462547104,
-0.0136374127751207));
#24909=CARTESIAN_POINT('Ctrl Pts',(-0.0130985494428649,-0.0353943240570536,
-0.0136015573800375));
#24910=CARTESIAN_POINT('Ctrl Pts',(-0.0132003161283345,-0.0353881695729477,
-0.0135508398608999));
#24911=CARTESIAN_POINT('Ctrl Pts',(-0.0132123035581187,-0.0353874475750909,
-0.0135446682574568));
#24912=CARTESIAN_POINT('Ctrl Pts',(-0.0132296667885471,-0.0353864078475456,
-0.0135354390991178));
#24913=CARTESIAN_POINT('Ctrl Pts',(-0.0132351072423483,-0.0353860829464431,
-0.013532505249609));
#24914=CARTESIAN_POINT('Ctrl Pts',(-0.0132447481074795,-0.0353855089708859,
-0.0135272312400917));
#24915=CARTESIAN_POINT('Ctrl Pts',(-0.0132489554029518,-0.0353852591022197,
-0.0135249040354987));
#24916=CARTESIAN_POINT('Ctrl Pts',(-0.0132580813174181,-0.0353847184987099,
-0.0135198003149205));
#24917=CARTESIAN_POINT('Ctrl Pts',(-0.0132629956168666,-0.0353844282362377,
-0.0135170164345293));
#24918=CARTESIAN_POINT('Ctrl Pts',(-0.0132769685716638,-0.0353836050470774,
-0.0135089992955165));
#24919=CARTESIAN_POINT('Ctrl Pts',(-0.0132859896018094,-0.0353830761505662,
-0.0135037007174639));
#24920=CARTESIAN_POINT('Ctrl Pts',(-0.0133590446671285,-0.0353788082271515,
-0.0134597858181012));
#24921=CARTESIAN_POINT('Ctrl Pts',(-0.0134202549907116,-0.0353753257478028,
-0.0134166488323846));
#24922=CARTESIAN_POINT('Ctrl Pts',(-0.0135767124135399,-0.035366033529131,
-0.0132884160783385));
#24923=CARTESIAN_POINT('Ctrl Pts',(-0.0136649187121481,-0.0353603083418362,
-0.0131956907410332));
#24924=CARTESIAN_POINT('Ctrl Pts',(-0.0137532075334448,-0.0353530188981106,
-0.013076276204333));
#24925=CARTESIAN_POINT('Ctrl Pts',(-0.0137653530709777,-0.0353519752543415,
-0.0130591268032346));
#24926=CARTESIAN_POINT('Ctrl Pts',(-0.0137831582557623,-0.0353503791444993,
-0.0130328648051373));
#24927=CARTESIAN_POINT('Ctrl Pts',(-0.0137890795647408,-0.0353498366123341,
-0.0130239321275609));
#24928=CARTESIAN_POINT('Ctrl Pts',(-0.0137995501911555,-0.0353488555306339,
-0.0130077734733189));
#24929=CARTESIAN_POINT('Ctrl Pts',(-0.0138041335205856,-0.035348418282341,
-0.0130005699973533));
#24930=CARTESIAN_POINT('Ctrl Pts',(-0.0138137916906811,-0.0353474798734455,
-0.0129851087056279));
#24931=CARTESIAN_POINT('Ctrl Pts',(-0.0138188489630555,-0.0353469780868683,
-0.0129768403942403));
#24932=CARTESIAN_POINT('Ctrl Pts',(-0.013832411201842,-0.035345603410027,
-0.012954190326563));
#24933=CARTESIAN_POINT('Ctrl Pts',(-0.0138407608375782,-0.035344724912894,
-0.0129397174795719));
#24934=CARTESIAN_POINT('Ctrl Pts',(-0.0138922347644605,-0.0353390977301337,
-0.0128470501612627));
#24935=CARTESIAN_POINT('Ctrl Pts',(-0.0139287317140502,-0.0353341135310749,
-0.0127653824252391));
#24936=CARTESIAN_POINT('Ctrl Pts',(-0.0139873036985356,-0.035323889821245,
-0.0125963407799078));
#24937=CARTESIAN_POINT('Ctrl Pts',(-0.0140092129194892,-0.0353186705221667,
-0.0125092579559972));
#24938=CARTESIAN_POINT('Ctrl Pts',(-0.0140287593860278,-0.0353117780849695,
-0.0123876721089134));
#24939=CARTESIAN_POINT('Ctrl Pts',(-0.0140330001986164,-0.0353099337113886,
-0.0123544118673696));
#24940=CARTESIAN_POINT('Ctrl Pts',(-0.0140370069540922,-0.0353076566286295,
-0.0123120175797208));
#24941=CARTESIAN_POINT('Ctrl Pts',(-0.0140377800268162,-0.0353071759668753,
-0.0123029897823005));
#24942=CARTESIAN_POINT('Ctrl Pts',(-0.0140388827043345,-0.0353064184909591,
-0.0122886256116348));
#24943=CARTESIAN_POINT('Ctrl Pts',(-0.0140392641630286,-0.0353061389109068,
-0.0122832935635803));
#24944=CARTESIAN_POINT('Ctrl Pts',(-0.0140399228468762,-0.0353056212513196,
-0.0122733615447578));
#24945=CARTESIAN_POINT('Ctrl Pts',(-0.0140402071831392,-0.0353053827895653,
-0.0122687622094284));
#24946=CARTESIAN_POINT('Ctrl Pts',(-0.0140407476026397,-0.0353048964943224,
-0.0122593350075553));
#24947=CARTESIAN_POINT('Ctrl Pts',(-0.0140410016089317,-0.0353046487738411,
-0.0122545070548441));
#24948=CARTESIAN_POINT('Ctrl Pts',(-0.0140417001238575,-0.0353039043255891,
-0.0122399241972072));
#24949=CARTESIAN_POINT('Ctrl Pts',(-0.0140420747354765,-0.035303411297403,
-0.012230166018556));
#24950=CARTESIAN_POINT('Ctrl Pts',(-0.0140427821474273,-0.0353021853411504,
-0.0122056756323501));
#24951=CARTESIAN_POINT('Ctrl Pts',(-0.014042996604584,-0.0353014580834576,
-0.012190940756967));
#24952=CARTESIAN_POINT('Ctrl Pts',(-0.0140429999599998,-0.0353007391609988,
-0.0121762046275615));
#24953=CARTESIAN_POINT('Ctrl Pts',(-0.0140429999576932,-0.0353007396482844,
-0.0121762146156828));
#24954=CARTESIAN_POINT('Ctrl Pts',(-0.0140429999866775,-0.0353007336098254,
-0.0121760908428857));
#24955=CARTESIAN_POINT('Ctrl Pts',(-0.014043,-0.0353007280592019,-0.0121759770585901));
#24956=CARTESIAN_POINT('Ctrl Pts',(-0.014043,-0.0353007220219321,-0.0121758532865547));
#24957=CARTESIAN_POINT('Ctrl Pts',(-0.014043,-0.0354167228394876,-0.0121758532865585));
#24958=CARTESIAN_POINT('Ctrl Pts',(-0.014043,-0.035417538263066,-0.0121926077765226));
#24959=CARTESIAN_POINT('Ctrl Pts',(-0.0140427271104671,-0.0354183611678139,
-0.0122093607612358));
#24960=CARTESIAN_POINT('Ctrl Pts',(-0.0140417685719733,-0.0354198211756583,
-0.012238777109034));
#24961=CARTESIAN_POINT('Ctrl Pts',(-0.0140411995180436,-0.0354204547183743,
-0.0122514427736288));
#24962=CARTESIAN_POINT('Ctrl Pts',(-0.0140399887678596,-0.035421520736642,
-0.0122725782331701));
#24963=CARTESIAN_POINT('Ctrl Pts',(-0.0140394330952479,-0.0354219505219931,
-0.0122810524402915));
#24964=CARTESIAN_POINT('Ctrl Pts',(-0.0140382045355412,-0.0354227988691123,
-0.0122976843243592));
#24965=CARTESIAN_POINT('Ctrl Pts',(-0.0140375366342218,-0.0354232172607349,
-0.0123058420935309));
#24966=CARTESIAN_POINT('Ctrl Pts',(-0.0140359793582494,-0.0354241107987572,
-0.0123231666507131));
#24967=CARTESIAN_POINT('Ctrl Pts',(-0.0140350727566955,-0.0354245864744903,
-0.0123323315372455));
#24968=CARTESIAN_POINT('Ctrl Pts',(-0.0140325448714191,-0.0354258094854592,
-0.0123557444887567));
#24969=CARTESIAN_POINT('Ctrl Pts',(-0.014030806934916,-0.0354265604788053,
-0.0123699788561657));
#24970=CARTESIAN_POINT('Ctrl Pts',(-0.0140229833542211,-0.0354296204633904,
-0.0124273928316668));
#24971=CARTESIAN_POINT('Ctrl Pts',(-0.014015267400232,-0.0354319802695828,
-0.0124703267818655));
#24972=CARTESIAN_POINT('Ctrl Pts',(-0.0139822027321551,-0.0354403440093628,
-0.0126180535266602));
#24973=CARTESIAN_POINT('Ctrl Pts',(-0.0139477065189253,-0.0354466011298809,
-0.0127204701704748));
#24974=CARTESIAN_POINT('Ctrl Pts',(-0.0138763762887735,-0.0354564035862904,
-0.0128761901813467));
#24975=CARTESIAN_POINT('Ctrl Pts',(-0.0138463810887516,-0.0354599911032783,
-0.0129322545595041));
#24976=CARTESIAN_POINT('Ctrl Pts',(-0.0138076263626106,-0.0354639511183184,
-0.012995040352923));
#24977=CARTESIAN_POINT('Ctrl Pts',(-0.0138021532101693,-0.0354644967010965,
-0.0130037126841737));
#24978=CARTESIAN_POINT('Ctrl Pts',(-0.0137935479553903,-0.0354653328691484,
-0.0130170513939889));
#24979=CARTESIAN_POINT('Ctrl Pts',(-0.0137904762307793,-0.0354656272164334,
-0.0130217561584067));
#24980=CARTESIAN_POINT('Ctrl Pts',(-0.0137847122174207,-0.0354661717675542,
-0.0130304800577772));
#24981=CARTESIAN_POINT('Ctrl Pts',(-0.0137820267200105,-0.0354664223849583,
-0.0130345033254885));
#24982=CARTESIAN_POINT('Ctrl Pts',(-0.0137758058959943,-0.0354669959460088,
-0.0130437287809533));
#24983=CARTESIAN_POINT('Ctrl Pts',(-0.0137722576408999,-0.0354673180164202,
-0.0130489220443681));
#24984=CARTESIAN_POINT('Ctrl Pts',(-0.0137607121587926,-0.0354683502437189,
-0.0130656002768523));
#24985=CARTESIAN_POINT('Ctrl Pts',(-0.0137525902033759,-0.0354690524408411,
-0.0130769984815103));
#24986=CARTESIAN_POINT('Ctrl Pts',(-0.0136885109390342,-0.0354744236599395,
-0.0131643855469434));
#24987=CARTESIAN_POINT('Ctrl Pts',(-0.0136258378970183,-0.0354787124484996,
-0.013235214955224));
#24988=CARTESIAN_POINT('Ctrl Pts',(-0.0134868969734785,-0.0354874302268959,
-0.013365880687416));
#24989=CARTESIAN_POINT('Ctrl Pts',(-0.0134106907122304,-0.0354918474751161,
-0.0134251616558607));
#24990=CARTESIAN_POINT('Ctrl Pts',(-0.0133082669836429,-0.035497770110377,
-0.0134904578721875));
#24991=CARTESIAN_POINT('Ctrl Pts',(-0.0132867470097625,-0.0354990126198941,
-0.0135034487772144));
#24992=CARTESIAN_POINT('Ctrl Pts',(-0.0132550445462775,-0.0355008450225241,
-0.013521544943571));
#24993=CARTESIAN_POINT('Ctrl Pts',(-0.013245107186957,-0.0355014196621042,
-0.0135270725780204));
#24994=CARTESIAN_POINT('Ctrl Pts',(-0.0132275083114406,-0.0355024381831614,
-0.0135366087404738));
#24995=CARTESIAN_POINT('Ctrl Pts',(-0.0132198724372623,-0.0355028803783177,
-0.0135406636831382));
#24996=CARTESIAN_POINT('Ctrl Pts',(-0.0132038619605968,-0.0355038082845106,
-0.0135489941199081));
#24997=CARTESIAN_POINT('Ctrl Pts',(-0.0131954815653213,-0.0355042943957357,
-0.0135532576552256));
#24998=CARTESIAN_POINT('Ctrl Pts',(-0.013173416306837,-0.0355055756006282,
-0.0135642306707867));
#24999=CARTESIAN_POINT('Ctrl Pts',(-0.0131596703157171,-0.0355063750508658,
-0.0135708143381179));
#25000=CARTESIAN_POINT('Ctrl Pts',(-0.0130993785241876,-0.0355098880897902,
-0.0135986007525472));
#25001=CARTESIAN_POINT('Ctrl Pts',(-0.0130518961096092,-0.0355126730668131,
-0.0136176836676285));
#25002=CARTESIAN_POINT('Ctrl Pts',(-0.0129106772181637,-0.0355209940506767,
-0.0136664398268578));
#25003=CARTESIAN_POINT('Ctrl Pts',(-0.0128149509892039,-0.035526696481029,
-0.0136895597022195));
#25004=CARTESIAN_POINT('Ctrl Pts',(-0.0126598867444597,-0.0355356611436972,
-0.0137116573244957));
#25005=CARTESIAN_POINT('Ctrl Pts',(-0.0126016597900705,-0.0355389627120218,
-0.0137166077098071));
#25006=CARTESIAN_POINT('Ctrl Pts',(-0.0125297516509561,-0.0355428570120161,
-0.0137186258642752));
#25007=CARTESIAN_POINT('Ctrl Pts',(-0.0125162100491415,-0.0355435823238261,
-0.0137188275721978));
#25008=CARTESIAN_POINT('Ctrl Pts',(-0.0124963930115429,-0.0355446302373783,
-0.0137188618263989));
#25009=CARTESIAN_POINT('Ctrl Pts',(-0.0124901188003424,-0.035544960030483,
-0.0137188344040641));
#25010=CARTESIAN_POINT('Ctrl Pts',(-0.012479019540911,-0.0355455397215488,
-0.013718718188697));
#25011=CARTESIAN_POINT('Ctrl Pts',(-0.0124741945214161,-0.0355457904663236,
-0.0137186450304713));
#25012=CARTESIAN_POINT('Ctrl Pts',(-0.0124636688862054,-0.0355463346864205,
-0.0137184360436819));
#25013=CARTESIAN_POINT('Ctrl Pts',(-0.0124579686271335,-0.0355466276652384,
-0.0137182912522884));
#25014=CARTESIAN_POINT('Ctrl Pts',(-0.0124419238167432,-0.0355474477251486,
-0.0137177946883889));
#25015=CARTESIAN_POINT('Ctrl Pts',(-0.0124315816373423,-0.035547970932797,
-0.0137173704186023));
#25016=CARTESIAN_POINT('Ctrl Pts',(-0.0123588578895035,-0.0355516168853343,
-0.013713653705422));
#25017=CARTESIAN_POINT('Ctrl Pts',(-0.0122967164334764,-0.0355545619364441,
-0.0137066793692749));
#25018=CARTESIAN_POINT('Ctrl Pts',(-0.0122155560241945,-0.0355583716479132,
-0.0136925394000703));
#25019=CARTESIAN_POINT('Ctrl Pts',(-0.0121960157883835,-0.0355592859007906,
-0.0136887441476266));
#25020=CARTESIAN_POINT('Ctrl Pts',(-0.0121113871561957,-0.0355632507623223,
-0.0136706010892576));
#25021=CARTESIAN_POINT('Ctrl Pts',(-0.0120471940633684,-0.0355662751546393,
-0.0136524227997781));
#25022=CARTESIAN_POINT('Ctrl Pts',(-0.0119449645359015,-0.0355713323502744,
-0.0136161773507942));
#25023=CARTESIAN_POINT('Ctrl Pts',(-0.0119061364059356,-0.0355733118418777,
-0.0136006071292289));
#25024=CARTESIAN_POINT('Ctrl Pts',(-0.0118416398519728,-0.0355767388122657,
-0.0135716488398111));
#25025=CARTESIAN_POINT('Ctrl Pts',(-0.0118156281260667,-0.035578160656025,
-0.0135590807864966));
#25026=CARTESIAN_POINT('Ctrl Pts',(-0.0117793336648419,-0.0355802087655277,
-0.0135402700007129));
#25027=CARTESIAN_POINT('Ctrl Pts',(-0.0117687468842372,-0.0355808140967,
-0.0135346254553647));
#25028=CARTESIAN_POINT('Ctrl Pts',(-0.0117505594061091,-0.0355818682492176,
-0.0135246543330535));
#25029=CARTESIAN_POINT('Ctrl Pts',(-0.0117429276040978,-0.0355823149901962,
-0.0135203854914519));
#25030=CARTESIAN_POINT('Ctrl Pts',(-0.0117273726661433,-0.0355832347480198,
-0.0135115104244732));
#25031=CARTESIAN_POINT('Ctrl Pts',(-0.0117194534695483,-0.0355837079773526,
-0.0135068980251071));
#25032=CARTESIAN_POINT('Ctrl Pts',(-0.0116994321632487,-0.0355849172845839,
-0.0134949968413004));
#25033=CARTESIAN_POINT('Ctrl Pts',(-0.0116873883797606,-0.0355856568624891,
-0.0134876119975843));
#25034=CARTESIAN_POINT('Ctrl Pts',(-0.0116403393984216,-0.0355885948941978,
-0.0134578665250885));
#25035=CARTESIAN_POINT('Ctrl Pts',(-0.0116061439513489,-0.0355908390715005,
-0.0134342630841133));
#25036=CARTESIAN_POINT('Ctrl Pts',(-0.0114790364240769,-0.0355996040285156,
-0.0133387301642425));
#25037=CARTESIAN_POINT('Ctrl Pts',(-0.0113935022152167,-0.0356064499641351,
-0.013257660257279));
#25038=CARTESIAN_POINT('Ctrl Pts',(-0.0112932882785753,-0.0356153425541661,
-0.0131382328369357));
#25039=CARTESIAN_POINT('Ctrl Pts',(-0.0112696796450308,-0.0356175132074002,
-0.0131078617142498));
#25040=CARTESIAN_POINT('Ctrl Pts',(-0.0112339166844679,-0.0356208896384625,
-0.0130581242507803));
#25041=CARTESIAN_POINT('Ctrl Pts',(-0.0112210154245895,-0.0356221280695043,
-0.0130393158384932));
#25042=CARTESIAN_POINT('Ctrl Pts',(-0.01120433420036,-0.0356237500805105,
-0.0130138020142348));
#25043=CARTESIAN_POINT('Ctrl Pts',(-0.0112001811113789,-0.035624155722908,
-0.0130073451964266));
#25044=CARTESIAN_POINT('Ctrl Pts',(-0.011193372102047,-0.0356248234552689,
-0.0129965835199921));
#25045=CARTESIAN_POINT('Ctrl Pts',(-0.0111906888870229,-0.0356250872966508,
-0.0129922961755423));
#25046=CARTESIAN_POINT('Ctrl Pts',(-0.0111856539079778,-0.0356255836202184,
-0.0129841624318032));
#25047=CARTESIAN_POINT('Ctrl Pts',(-0.0111832978414756,-0.0356258163942267,
-0.0129803187927589));
#25048=CARTESIAN_POINT('Ctrl Pts',(-0.0111771081509562,-0.0356264294688649,
-0.012970121015926));
#25049=CARTESIAN_POINT('Ctrl Pts',(-0.0111733034174747,-0.0356268079148198,
-0.0129637493789283));
#25050=CARTESIAN_POINT('Ctrl Pts',(-0.0111598008641189,-0.0356281576818971,
-0.0129407620350326));
#25051=CARTESIAN_POINT('Ctrl Pts',(-0.0111503676755422,-0.0356291133641934,
-0.0129239921566899));
#25052=CARTESIAN_POINT('Ctrl Pts',(-0.0110937802677852,-0.0356349547750304,
-0.0128188382703318));
#25053=CARTESIAN_POINT('Ctrl Pts',(-0.011055008709352,-0.0356394595560296,
-0.0127262055578693));
#25054=CARTESIAN_POINT('Ctrl Pts',(-0.0109972071381422,-0.0356484442081871,
-0.0125387272801521));
#25055=CARTESIAN_POINT('Ctrl Pts',(-0.010977548926401,-0.0356529017668573,
-0.0124445615224224));
#25056=CARTESIAN_POINT('Ctrl Pts',(-0.0109648666206234,-0.0356584903818084,
-0.0123323800309566));
#25057=CARTESIAN_POINT('Ctrl Pts',(-0.010963243024204,-0.0356593358806267,
-0.0123155425240403));
#25058=CARTESIAN_POINT('Ctrl Pts',(-0.0109611194310561,-0.0356606831066016,
-0.0122889501884429));
#25059=CARTESIAN_POINT('Ctrl Pts',(-0.0109604346580237,-0.0356611790062028,
-0.0122792112409949));
#25060=CARTESIAN_POINT('Ctrl Pts',(-0.0109593223034823,-0.0356621158097155,
-0.0122609104097332));
#25061=CARTESIAN_POINT('Ctrl Pts',(-0.0109588735602583,-0.0356625560275748,
-0.0122523501591947));
#25062=CARTESIAN_POINT('Ctrl Pts',(-0.0109580240645614,-0.035663552040944,
-0.0122330739255528));
#25063=CARTESIAN_POINT('Ctrl Pts',(-0.0109576636510691,-0.035664109086248,
-0.0122223566835455));
#25064=CARTESIAN_POINT('Ctrl Pts',(-0.0109569136485729,-0.0356657997806266,
-0.0121900249013261));
#25065=CARTESIAN_POINT('Ctrl Pts',(-0.0109568665669177,-0.0356669440732218,
-0.0121684057175958));
#25066=CARTESIAN_POINT('Ctrl Pts',(-0.0109592410085505,-0.0356736985751078,
-0.0120423518205215));
#25067=CARTESIAN_POINT('Ctrl Pts',(-0.0109718087919673,-0.035679626460196,
-0.0119383944508523));
#25068=CARTESIAN_POINT('Ctrl Pts',(-0.0110097316105512,-0.0356895421858127,
-0.011770175775862));
#25069=CARTESIAN_POINT('Ctrl Pts',(-0.0110290581599853,-0.0356934675244374,
-0.0117048916354903));
#25070=CARTESIAN_POINT('Ctrl Pts',(-0.0110601871920318,-0.0356984853357591,
-0.0116206383538668));
#25071=CARTESIAN_POINT('Ctrl Pts',(-0.011068177974536,-0.035699689769178,
-0.0116003445464052));
#25072=CARTESIAN_POINT('Ctrl Pts',(-0.0110824716121913,-0.0357017019349492,
-0.0115661862422581));
#25073=CARTESIAN_POINT('Ctrl Pts',(-0.0110885542779068,-0.0357025194664206,
-0.0115522334961816));
#25074=CARTESIAN_POINT('Ctrl Pts',(-0.0110975583502747,-0.0357036736439031,
-0.0115323864046457));
#25075=CARTESIAN_POINT('Ctrl Pts',(-0.0111003123642749,-0.0357040196075081,
-0.011526417581899));
#25076=CARTESIAN_POINT('Ctrl Pts',(-0.0111051679466173,-0.0357046172303319,
-0.0115160683642111));
#25077=CARTESIAN_POINT('Ctrl Pts',(-0.0111072521887665,-0.0357048699269926,
-0.0115116800128579));
#25078=CARTESIAN_POINT('Ctrl Pts',(-0.011111746590513,-0.0357054066688588,
-0.0115023312881098));
#25079=CARTESIAN_POINT('Ctrl Pts',(-0.0111141626440735,-0.0357056903493329,
-0.0114973739308591));
#25080=CARTESIAN_POINT('Ctrl Pts',(-0.0111208218361023,-0.0357064594261836,
-0.0114838943122178));
#25081=CARTESIAN_POINT('Ctrl Pts',(-0.0111251174143067,-0.0357069416761742,
-0.0114753980673129));
#25082=CARTESIAN_POINT('Ctrl Pts',(-0.0111482697008385,-0.035709471740201,
-0.0114306387248139));
#25083=CARTESIAN_POINT('Ctrl Pts',(-0.0111684844176995,-0.0357114444378021,
-0.0113950932149696));
#25084=CARTESIAN_POINT('Ctrl Pts',(-0.0112343653579111,-0.0357173289109132,
-0.0112892659824057));
#25085=CARTESIAN_POINT('Ctrl Pts',(-0.0112843632695977,-0.0357210991646329,
-0.0112218634153045));
#25086=CARTESIAN_POINT('Ctrl Pts',(-0.0113918466557909,-0.0357285905173704,
-0.0110992235615449));
#25087=CARTESIAN_POINT('Ctrl Pts',(-0.0114486195185337,-0.0357322931406509,
-0.0110437168676197));
#25088=CARTESIAN_POINT('Ctrl Pts',(-0.0115255665755736,-0.0357372208744698,
-0.0109792861058802));
#25089=CARTESIAN_POINT('Ctrl Pts',(-0.0115420067217226,-0.0357382684137658,
-0.0109660837459334));
#25090=CARTESIAN_POINT('Ctrl Pts',(-0.0115671252196121,-0.0357398637809694,
-0.0109467453222488));
#25091=CARTESIAN_POINT('Ctrl Pts',(-0.0115756051946543,-0.0357404015124628,
-0.0109403550144667));
#25092=CARTESIAN_POINT('Ctrl Pts',(-0.0115910412616539,-0.0357413791122815,
-0.0109289706433845));
#25093=CARTESIAN_POINT('Ctrl Pts',(-0.0115979742973058,-0.0357418177561619,
-0.0109239459650628));
#25094=CARTESIAN_POINT('Ctrl Pts',(-0.0116129585651714,-0.0357427650096174,
-0.0109132752942515));
#25095=CARTESIAN_POINT('Ctrl Pts',(-0.0116210226409081,-0.0357432743163894,
-0.0109076480626554));
#25096=CARTESIAN_POINT('Ctrl Pts',(-0.0116430094375146,-0.0357446619019811,
-0.0108926157944065));
#25097=CARTESIAN_POINT('Ctrl Pts',(-0.011657032607279,-0.035745545796952,
-0.0108833606443831));
#25098=CARTESIAN_POINT('Ctrl Pts',(-0.0117484809983781,-0.0357513044388423,
-0.0108251269832672));
#25099=CARTESIAN_POINT('Ctrl Pts',(-0.0118299762477806,-0.0357564277451144,
-0.010782904518244));
#25100=CARTESIAN_POINT('Ctrl Pts',(-0.0119926333580017,-0.0357664852478599,
-0.0107162238407659));
#25101=CARTESIAN_POINT('Ctrl Pts',(-0.0120730268582602,-0.0357713809695852,
-0.010690715827138));
#25102=CARTESIAN_POINT('Ctrl Pts',(-0.0121788509745417,-0.035777472936617,
-0.0106664474247667));
#25103=CARTESIAN_POINT('Ctrl Pts',(-0.0122027282525893,-0.03577882431594,
-0.0106615638936586));
#25104=CARTESIAN_POINT('Ctrl Pts',(-0.0122429724663214,-0.0357810524983995,
-0.0106543215560742));
#25105=CARTESIAN_POINT('Ctrl Pts',(-0.0122592793707944,-0.0357819418388727,
-0.0106516565860661));
#25106=CARTESIAN_POINT('Ctrl Pts',(-0.0122823438622849,-0.035783177681601,
-0.0106482666596645));
#25107=CARTESIAN_POINT('Ctrl Pts',(-0.0122890677373651,-0.0357835353283668,
-0.010647323705256));
#25108=CARTESIAN_POINT('Ctrl Pts',(-0.012300643912423,-0.0357841462860588,
-0.0106457781072292));
#25109=CARTESIAN_POINT('Ctrl Pts',(-0.0123054932135286,-0.0357844007720166,
-0.0106451540945236));
#25110=CARTESIAN_POINT('Ctrl Pts',(-0.0123157120487281,-0.0357849339146059,
-0.0106438884723644));
#25111=CARTESIAN_POINT('Ctrl Pts',(-0.0123210820699328,-0.035785212286465,
-0.010643252028253));
#25112=CARTESIAN_POINT('Ctrl Pts',(-0.0123356752054156,-0.0357859641576637,
-0.0106416002253992));
#25113=CARTESIAN_POINT('Ctrl Pts',(-0.0123449044475783,-0.0357864346750686,
-0.0106406397927773));
#25114=CARTESIAN_POINT('Ctrl Pts',(-0.0123897463113916,-0.0357886989309618,
-0.0106363818771694));
#25115=CARTESIAN_POINT('Ctrl Pts',(-0.0124254598653898,-0.0357904355883029,
-0.0106342397785467));
#25116=CARTESIAN_POINT('Ctrl Pts',(-0.0125485986406493,-0.0357962896463038,
-0.0106311437973323));
#25117=CARTESIAN_POINT('Ctrl Pts',(-0.0126360124487232,-0.0358002211655603,
-0.0106363756144821));
#25118=CARTESIAN_POINT('Ctrl Pts',(-0.0127963420740552,-0.0358076581588916,
-0.0106597410437196));
#25119=CARTESIAN_POINT('Ctrl Pts',(-0.0128692853572265,-0.0358111313058451,
-0.0106758392841192));
#25120=CARTESIAN_POINT('Ctrl Pts',(-0.0129652689056642,-0.0358160115089282,
-0.010704450157234));
#25121=CARTESIAN_POINT('Ctrl Pts',(-0.0129895778562697,-0.035817274444655,
-0.010712358922853));
#25122=CARTESIAN_POINT('Ctrl Pts',(-0.0130244713756424,-0.0358191315425556,
-0.0107246779749105));
#25123=CARTESIAN_POINT('Ctrl Pts',(-0.013035221477153,-0.0358197098504035,
-0.0107286083279273));
#25124=CARTESIAN_POINT('Ctrl Pts',(-0.0130540235151206,-0.0358207325892026,
-0.0107357206938683));
#25125=CARTESIAN_POINT('Ctrl Pts',(-0.0130620943239165,-0.0358211752876358,
-0.0107388515792498));
#25126=CARTESIAN_POINT('Ctrl Pts',(-0.013078845384833,-0.0358221019787196,
-0.0107455124802516));
#25127=CARTESIAN_POINT('Ctrl Pts',(-0.0130875206639524,-0.0358225863471656,
-0.0107490539783336));
#25128=CARTESIAN_POINT('Ctrl Pts',(-0.0131100806439124,-0.0358238577821161,
-0.0107585042479233));
#25129=CARTESIAN_POINT('Ctrl Pts',(-0.0131239116442288,-0.035824649084183,
-0.0107645379682441));
#25130=CARTESIAN_POINT('Ctrl Pts',(-0.0131837227946175,-0.0358281236661638,
-0.0107916813906519));
#25131=CARTESIAN_POINT('Ctrl Pts',(-0.0132287337563207,-0.0358308768061549,
-0.0108148407845955));
#25132=CARTESIAN_POINT('Ctrl Pts',(-0.0133580888275027,-0.035839193754723,
-0.0108896560860379));
#25133=CARTESIAN_POINT('Ctrl Pts',(-0.0134386966940992,-0.0358449296268151,
-0.0109472502910151));
#25134=CARTESIAN_POINT('Ctrl Pts',(-0.0135574242818815,-0.0358539404575158,
-0.0110506261666084));
#25135=CARTESIAN_POINT('Ctrl Pts',(-0.0135993906310767,-0.0358572543292559,
-0.0110915915455285));
#25136=CARTESIAN_POINT('Ctrl Pts',(-0.0136480799681388,-0.0358611613542917,
-0.0111448608462335));
#25137=CARTESIAN_POINT('Ctrl Pts',(-0.0136571000404844,-0.0358618879504305,
-0.0111549945567507));
#25138=CARTESIAN_POINT('Ctrl Pts',(-0.0136700982185564,-0.0358629373931393,
-0.0111699911751856));
#25139=CARTESIAN_POINT('Ctrl Pts',(-0.0136741819175222,-0.0358632674573547,
-0.0111747612551081));
#25140=CARTESIAN_POINT('Ctrl Pts',(-0.0136813536579705,-0.0358638475325092,
-0.0111832426671715));
#25141=CARTESIAN_POINT('Ctrl Pts',(-0.0136844535431825,-0.0358640983920467,
-0.0111869437290948));
#25142=CARTESIAN_POINT('Ctrl Pts',(-0.0136911777512973,-0.0358646428065021,
-0.0111950489766623));
#25143=CARTESIAN_POINT('Ctrl Pts',(-0.0136947950605076,-0.0358649358653873,
-0.0111994587480089));
#25144=CARTESIAN_POINT('Ctrl Pts',(-0.0137049057401215,-0.0358657558476487,
-0.0112119247516473));
#25145=CARTESIAN_POINT('Ctrl Pts',(-0.0137113427571681,-0.0358662789044783,
-0.011220026524731));
#25146=CARTESIAN_POINT('Ctrl Pts',(-0.0137558875444062,-0.0358699104599345,
-0.0112772644152026));
#25147=CARTESIAN_POINT('Ctrl Pts',(-0.0137910797333647,-0.0358728430552178,
-0.0113286047588747));
#25148=CARTESIAN_POINT('Ctrl Pts',(-0.0138590239319443,-0.0358789514660897,
-0.0114418348156645));
#25149=CARTESIAN_POINT('Ctrl Pts',(-0.0138908587964206,-0.0358821075324161,
-0.0115041083911386));
#25150=CARTESIAN_POINT('Ctrl Pts',(-0.0139466453468204,-0.0358886443007121,
-0.0116343504305186));
#25151=CARTESIAN_POINT('Ctrl Pts',(-0.0139702790972508,-0.0358920218825581,
-0.0117022647089915));
#25152=CARTESIAN_POINT('Ctrl Pts',(-0.0139943697395063,-0.0358965446035975,
-0.0117909984710678));
#25153=CARTESIAN_POINT('Ctrl Pts',(-0.0139992627618673,-0.0358975459972766,
-0.0118105242962637));
#25154=CARTESIAN_POINT('Ctrl Pts',(-0.014006109641926,-0.0358990850461903,
-0.0118403066050354));
#25155=CARTESIAN_POINT('Ctrl Pts',(-0.0140083437815026,-0.0358996136832455,
-0.011850496776193));
#25156=CARTESIAN_POINT('Ctrl Pts',(-0.0140120526384652,-0.0359005397057748,
-0.0118682731650658));
#25157=CARTESIAN_POINT('Ctrl Pts',(-0.0140135740262824,-0.0359009355747758,
-0.0118758493254116));
#25158=CARTESIAN_POINT('Ctrl Pts',(-0.0140168739668857,-0.0359018317763048,
-0.0118929466232066));
#25159=CARTESIAN_POINT('Ctrl Pts',(-0.0140186198956436,-0.0359023331364207,
-0.0119024736633533));
#25160=CARTESIAN_POINT('Ctrl Pts',(-0.0140231048398058,-0.0359036986921826,
-0.0119283167217085));
#25161=CARTESIAN_POINT('Ctrl Pts',(-0.0140256712723982,-0.0359045683313978,
-0.0119446610640595));
#25162=CARTESIAN_POINT('Ctrl Pts',(-0.0140379803374731,-0.0359092602595188,
-0.0120322171326661));
#25163=CARTESIAN_POINT('Ctrl Pts',(-0.014043,-0.0359132300652073,-0.0121039945751363));
#25164=CARTESIAN_POINT('Ctrl Pts',(-0.014043,-0.0359172995678105,-0.0121758532865631));
#25165=CARTESIAN_POINT('Origin',(-0.0125,-0.0375520664398416,-0.0121758532865581));
#25166=CARTESIAN_POINT('',(-0.0140437065963746,-0.0364192084819633,-0.0121758951269253));
#25167=CARTESIAN_POINT('',(-0.014043,-0.0363035228772662,-0.012175853286558));
#25168=CARTESIAN_POINT('',(-0.014043,-0.0375520664398416,-0.012175853286558));
#25169=CARTESIAN_POINT('',(-0.0118291591918074,-0.0365787743898683,-0.0135653933579797));
#25170=CARTESIAN_POINT('Ctrl Pts',(-0.0140437065963746,-0.0364192084819633,
-0.0121758951269253));
#25171=CARTESIAN_POINT('Ctrl Pts',(-0.0140437112943485,-0.036419761179091,
-0.0121864484221882));
#25172=CARTESIAN_POINT('Ctrl Pts',(-0.0140436034281201,-0.0364203105081606,
-0.0121969992050036));
#25173=CARTESIAN_POINT('Ctrl Pts',(-0.0140433816474543,-0.036420856696369,
-0.0122075457453187));
#25174=CARTESIAN_POINT('Ctrl Pts',(-0.0140366019703916,-0.0364375532810555,
-0.0125299459744092));
#25175=CARTESIAN_POINT('Ctrl Pts',(-0.0139230960548442,-0.0364513147894128,
-0.012850374408135));
#25176=CARTESIAN_POINT('Ctrl Pts',(-0.0137289094917718,-0.0364686314224829,
-0.0131077331936447));
#25177=CARTESIAN_POINT('Ctrl Pts',(-0.0136165391819018,-0.0364786520716628,
-0.0132566594943009));
#25178=CARTESIAN_POINT('Ctrl Pts',(-0.0134773604198345,-0.0364896481824746,
-0.0133847691368121));
#25179=CARTESIAN_POINT('Ctrl Pts',(-0.0133205998717288,-0.036499396683921,
-0.0134832463847913));
#25180=CARTESIAN_POINT('Ctrl Pts',(-0.0133159948840397,-0.0364996830552669,
-0.0134861392460379));
#25181=CARTESIAN_POINT('Ctrl Pts',(-0.0133113740270396,-0.0364999685740012,
-0.0134890066645617));
#25182=CARTESIAN_POINT('Ctrl Pts',(-0.0133067374026243,-0.0365002532689413,
-0.0134918483279206));
#25183=CARTESIAN_POINT('Ctrl Pts',(-0.0130296930677077,-0.0365172641616254,
-0.013661641406849));
#25184=CARTESIAN_POINT('Ctrl Pts',(-0.0126940553902617,-0.0365313339299439,
-0.0137398854281534));
#25185=CARTESIAN_POINT('Ctrl Pts',(-0.0123670284176581,-0.0365486100887429,
-0.0137121595855382));
#25186=CARTESIAN_POINT('Ctrl Pts',(-0.0121807148347873,-0.0365584526501025,
-0.0136963636374712));
#25187=CARTESIAN_POINT('Ctrl Pts',(-0.0119971991141735,-0.0365691508384448,
-0.0136465196655769));
#25188=CARTESIAN_POINT('Ctrl Pts',(-0.0118291591918087,-0.0365787743898699,
-0.0135653933579771));
#25189=CARTESIAN_POINT('',(-0.0110424215937398,-0.0365780008767028,-0.0116655070342102));
#25190=CARTESIAN_POINT('Origin',(-0.01249999999999,-0.0365787743898623,
-0.0121758532865681));
#25191=CARTESIAN_POINT('Ctrl Pts',(-0.0110436695558073,-0.0365772219729834,
-0.0116659997415889));
#25192=CARTESIAN_POINT('Ctrl Pts',(-0.0110413413253198,-0.0365768613442727,
-0.0116726500296443));
#25193=CARTESIAN_POINT('Ctrl Pts',(-0.0110390586313932,-0.0365765033099709,
-0.0116793163109309));
#25194=CARTESIAN_POINT('Ctrl Pts',(-0.0110331441531789,-0.0365755630462582,
-0.0116969826275963));
#25195=CARTESIAN_POINT('Ctrl Pts',(-0.0110295903814817,-0.0365749849430677,
-0.0117080084925528));
#25196=CARTESIAN_POINT('Ctrl Pts',(-0.0110018695876898,-0.0365703579284431,
-0.0117974520234474));
#25197=CARTESIAN_POINT('Ctrl Pts',(-0.0109838665983412,-0.0365665919497779,
-0.0118776513718294));
#25198=CARTESIAN_POINT('Ctrl Pts',(-0.0109610197781968,-0.0365591623540998,
-0.0120385331394252));
#25199=CARTESIAN_POINT('Ctrl Pts',(-0.0109559550810136,-0.0365555071961878,
-0.0121189184109854));
#25200=CARTESIAN_POINT('Ctrl Pts',(-0.0109576515052428,-0.03655022296515,
-0.0122304092373323));
#25201=CARTESIAN_POINT('Ctrl Pts',(-0.0109590634848909,-0.0365487288644723,
-0.0122614672222852));
#25202=CARTESIAN_POINT('Ctrl Pts',(-0.0109631698988874,-0.0365460697877951,
-0.012315649868047));
#25203=CARTESIAN_POINT('Ctrl Pts',(-0.0109654513753443,-0.036544917066,
-0.0123387958887093));
#25204=CARTESIAN_POINT('Ctrl Pts',(-0.0109695920243148,-0.0365431907320122,
-0.0123728898705308));
#25205=CARTESIAN_POINT('Ctrl Pts',(-0.0109710476816302,-0.03654262967808,
-0.0123838840232355));
#25206=CARTESIAN_POINT('Ctrl Pts',(-0.0109738529018824,-0.0365416231574254,
-0.0124034478349961));
#25207=CARTESIAN_POINT('Ctrl Pts',(-0.0109751564699005,-0.0365411791495177,
-0.0124120236662987));
#25208=CARTESIAN_POINT('Ctrl Pts',(-0.010978068081404,-0.0365402346714895,
-0.0124301483828666));
#25209=CARTESIAN_POINT('Ctrl Pts',(-0.010979693837407,-0.0365397336622288,
-0.0124396940096787));
#25210=CARTESIAN_POINT('Ctrl Pts',(-0.0109842970108224,-0.0365383817039533,
-0.0124652649548254));
#25211=CARTESIAN_POINT('Ctrl Pts',(-0.0109874386312575,-0.036537525648099,
-0.0124812591541087));
#25212=CARTESIAN_POINT('Ctrl Pts',(-0.0110048757141424,-0.0365330878068891,
-0.0125631503139248));
#25213=CARTESIAN_POINT('Ctrl Pts',(-0.0110232247437051,-0.0365293801249451,
-0.0126281018280259));
#25214=CARTESIAN_POINT('Ctrl Pts',(-0.0110792690894689,-0.0365199418545631,
-0.0127861167056582));
#25215=CARTESIAN_POINT('Ctrl Pts',(-0.0111219029326016,-0.0365141171036886,
-0.0128770987029434));
#25216=CARTESIAN_POINT('Ctrl Pts',(-0.0111864714025118,-0.0365070199561684,
-0.012985904180547));
#25217=CARTESIAN_POINT('Ctrl Pts',(-0.011200460812554,-0.0365055618840411,
-0.0130081620321976));
#25218=CARTESIAN_POINT('Ctrl Pts',(-0.0112246982922675,-0.0365031760519759,
-0.0130446229127339));
#25219=CARTESIAN_POINT('Ctrl Pts',(-0.0112346315146955,-0.0365022341795758,
-0.0130590281018188));
#25220=CARTESIAN_POINT('Ctrl Pts',(-0.0112488954723028,-0.0365009342774367,
-0.0130789788889831));
#25221=CARTESIAN_POINT('Ctrl Pts',(-0.0112530220518657,-0.0365005641265106,
-0.0130846681155898));
#25222=CARTESIAN_POINT('Ctrl Pts',(-0.0112601502576373,-0.0364999350416149,
-0.0130943556590413));
#25223=CARTESIAN_POINT('Ctrl Pts',(-0.011263132681514,-0.0364996748537728,
-0.0130983679097475));
#25224=CARTESIAN_POINT('Ctrl Pts',(-0.0112693765992203,-0.0364991364985014,
-0.0131066831295149));
#25225=CARTESIAN_POINT('Ctrl Pts',(-0.0112726412832027,-0.0364988585582687,
-0.0131109836160336));
#25226=CARTESIAN_POINT('Ctrl Pts',(-0.0112815235986745,-0.036498111607591,
-0.0131225574195308));
#25227=CARTESIAN_POINT('Ctrl Pts',(-0.0112871838259889,-0.0364976454637784,
-0.0131297979347385));
#25228=CARTESIAN_POINT('Ctrl Pts',(-0.0113143539787749,-0.0364954518495148,
-0.0131639210106748));
#25229=CARTESIAN_POINT('Ctrl Pts',(-0.0113366962779269,-0.036493776475585,
-0.0131901308971525));
#25230=CARTESIAN_POINT('Ctrl Pts',(-0.0114191879601148,-0.0364879423349833,
-0.0132805869397727));
#25231=CARTESIAN_POINT('Ctrl Pts',(-0.0114839332225997,-0.0364839774412235,
-0.0133404137763914));
#25232=CARTESIAN_POINT('Ctrl Pts',(-0.0116236752279367,-0.0364758436404758,
-0.0134489660993623));
#25233=CARTESIAN_POINT('Ctrl Pts',(-0.0116985037441817,-0.0364716849115544,
-0.0134973535182993));
#25234=CARTESIAN_POINT('Ctrl Pts',(-0.0117918364787748,-0.0364664504687041,
-0.0135468501986224));
#25235=CARTESIAN_POINT('Ctrl Pts',(-0.0118067216300561,-0.0364656147820267,
-0.0135544370454084));
#25236=CARTESIAN_POINT('Ctrl Pts',(-0.0118304430635244,-0.0364642803300907,
-0.0135660463239072));
#25237=CARTESIAN_POINT('Ctrl Pts',(-0.011839199355654,-0.0364637871813342,
-0.0135702297332574));
#25238=CARTESIAN_POINT('Ctrl Pts',(-0.0118557496459913,-0.0364628537850768,
-0.0135779459006358));
#25239=CARTESIAN_POINT('Ctrl Pts',(-0.0118635347276592,-0.0364624141931766,
-0.0135814969719489));
#25240=CARTESIAN_POINT('Ctrl Pts',(-0.0118811676824705,-0.0364614171746888,
-0.0135893635131932));
#25241=CARTESIAN_POINT('Ctrl Pts',(-0.0118910318671119,-0.036460858477707,
-0.0135936411420864));
#25242=CARTESIAN_POINT('Ctrl Pts',(-0.0119210661205281,-0.0364591541865196,
-0.0136062943118299));
#25243=CARTESIAN_POINT('Ctrl Pts',(-0.011941369454711,-0.0364579977204633,
-0.0136143447921375));
#25244=CARTESIAN_POINT('Ctrl Pts',(-0.0120527574339059,-0.0364516274201177,
-0.0136557974226373));
#25245=CARTESIAN_POINT('Ctrl Pts',(-0.0121466548019251,-0.0364461451595593,
-0.0136809788599299));
#25246=CARTESIAN_POINT('Ctrl Pts',(-0.0123415290797136,-0.0364347883212946,
-0.0137139913812855));
#25247=CARTESIAN_POINT('Ctrl Pts',(-0.0124421895407285,-0.0364289365899841,
-0.0137210530108708));
#25248=CARTESIAN_POINT('Ctrl Pts',(-0.0125550736832121,-0.0364228218462438,
-0.0137179187985579));
#25249=CARTESIAN_POINT('Ctrl Pts',(-0.012567318580438,-0.0364221647166439,
-0.013717432794944));
#25250=CARTESIAN_POINT('Ctrl Pts',(-0.0125856534854465,-0.036421191296847,
-0.0137164861921277));
#25251=CARTESIAN_POINT('Ctrl Pts',(-0.0125917484028276,-0.0364208694574206,
-0.0137161352420211));
#25252=CARTESIAN_POINT('Ctrl Pts',(-0.0126027345821641,-0.036420292685185,
-0.0137154372068821));
#25253=CARTESIAN_POINT('Ctrl Pts',(-0.0126076265510193,-0.0364200370559862,
-0.0137151029638449));
#25254=CARTESIAN_POINT('Ctrl Pts',(-0.0126176258330754,-0.0364195171130362,
-0.0137143718610214));
#25255=CARTESIAN_POINT('Ctrl Pts',(-0.0126227329326062,-0.0364192529242134,
-0.0137139728753217));
#25256=CARTESIAN_POINT('Ctrl Pts',(-0.0126359960318198,-0.0364185701728793,
-0.0137128702325989));
#25257=CARTESIAN_POINT('Ctrl Pts',(-0.0126441486869814,-0.0364181537836636,
-0.0137121270820833));
#25258=CARTESIAN_POINT('Ctrl Pts',(-0.0126801668027033,-0.0364163272435666,
-0.0137085546243455));
#25259=CARTESIAN_POINT('Ctrl Pts',(-0.0127079595924972,-0.0364149523757724,
-0.0137050316462605));
#25260=CARTESIAN_POINT('Ctrl Pts',(-0.0127881091964472,-0.0364110489374761,
-0.0136926461434163));
#25261=CARTESIAN_POINT('Ctrl Pts',(-0.012840125523996,-0.0364085914089047,
-0.0136818356039508));
#25262=CARTESIAN_POINT('Ctrl Pts',(-0.0130152296410503,-0.0364002894449418,
-0.0136359060510962));
#25263=CARTESIAN_POINT('Ctrl Pts',(-0.0131344473943982,-0.0363945393897937,
-0.0135881883457398));
#25264=CARTESIAN_POINT('Ctrl Pts',(-0.0132618881358502,-0.0363873732161357,
-0.0135177505513322));
#25265=CARTESIAN_POINT('Ctrl Pts',(-0.0132772186293565,-0.0363864939817884,
-0.0135089297925464));
#25266=CARTESIAN_POINT('Ctrl Pts',(-0.0133017351985128,-0.0363850581900037,
-0.0134942569389985));
#25267=CARTESIAN_POINT('Ctrl Pts',(-0.0133110170662623,-0.0363845075691182,
-0.0134885675851075));
#25268=CARTESIAN_POINT('Ctrl Pts',(-0.0133274176793357,-0.0363835217115884,
-0.0134782744319408));
#25269=CARTESIAN_POINT('Ctrl Pts',(-0.0133345602036579,-0.0363830879287251,
-0.0134737092564782));
#25270=CARTESIAN_POINT('Ctrl Pts',(-0.0133495578165482,-0.0363821675132236,
-0.0134639484723184));
#25271=CARTESIAN_POINT('Ctrl Pts',(-0.0133574036588562,-0.0363816803791029,
-0.0134587393499677));
#25272=CARTESIAN_POINT('Ctrl Pts',(-0.0133782216519824,-0.0363803724984877,
-0.0134446412950377));
#25273=CARTESIAN_POINT('Ctrl Pts',(-0.0133911061947453,-0.0363795469151349,
-0.0134356254902591));
#25274=CARTESIAN_POINT('Ctrl Pts',(-0.0134589528571959,-0.0363751116892407,
-0.0133865889232085));
#25275=CARTESIAN_POINT('Ctrl Pts',(-0.0135113565166372,-0.0363713689783282,
-0.0133431696584503));
#25276=CARTESIAN_POINT('Ctrl Pts',(-0.0136300417414365,-0.0363621389831824,
-0.0132308250161338));
#25277=CARTESIAN_POINT('Ctrl Pts',(-0.0136931189529005,-0.0363565699079917,
-0.0131589226767223));
#25278=CARTESIAN_POINT('Ctrl Pts',(-0.0137784575429079,-0.0363483039904904,
-0.0130412365326283));
#25279=CARTESIAN_POINT('Ctrl Pts',(-0.0138057910623317,-0.0363455122864103,
-0.012999414091956));
#25280=CARTESIAN_POINT('Ctrl Pts',(-0.0138360674834308,-0.036342300838994,
-0.0129477801386804));
#25281=CARTESIAN_POINT('Ctrl Pts',(-0.0138410022080424,-0.0363417731941031,
-0.0129391752851103));
#25282=CARTESIAN_POINT('Ctrl Pts',(-0.013848569380809,-0.0363409581287575,
-0.0129256802362088));
#25283=CARTESIAN_POINT('Ctrl Pts',(-0.0138512589063317,-0.0363406672233578,
-0.0129208225471677));
#25284=CARTESIAN_POINT('Ctrl Pts',(-0.0138559859010768,-0.0363401539126488,
-0.0129121750558806));
#25285=CARTESIAN_POINT('Ctrl Pts',(-0.0138580337537298,-0.0363399308538065,
-0.0129083912281472));
#25286=CARTESIAN_POINT('Ctrl Pts',(-0.0138629145975095,-0.0363393974964837,
-0.0128992820548153));
#25287=CARTESIAN_POINT('Ctrl Pts',(-0.0138657322196297,-0.036339088170409,
-0.0128939486071689));
#25288=CARTESIAN_POINT('Ctrl Pts',(-0.0138742494954952,-0.0363381482922685,
-0.012877594871444));
#25289=CARTESIAN_POINT('Ctrl Pts',(-0.0138798476981278,-0.0363375237742507,
-0.0128665220032575));
#25290=CARTESIAN_POINT('Ctrl Pts',(-0.0139225301212537,-0.0363326990408032,
-0.0127795081289901));
#25291=CARTESIAN_POINT('Ctrl Pts',(-0.0139534560740148,-0.0363288136101808,
-0.0127006957296058));
#25292=CARTESIAN_POINT('Ctrl Pts',(-0.0140114615447175,-0.0363195886396248,
-0.0125075858141706));
#25293=CARTESIAN_POINT('Ctrl Pts',(-0.014032270353752,-0.0363142705475785,
-0.0123919727712827));
#25294=CARTESIAN_POINT('Ctrl Pts',(-0.0140410174835801,-0.036307579139371,
-0.0122562906716157));
#25295=CARTESIAN_POINT('Ctrl Pts',(-0.0140418858837587,-0.0363066405351284,
-0.0122374401385291));
#25296=CARTESIAN_POINT('Ctrl Pts',(-0.0140426307508922,-0.0363052870875798,
-0.0122105502030893));
#25297=CARTESIAN_POINT('Ctrl Pts',(-0.0140427904568757,-0.0363048810602615,
-0.0122025199818726));
#25298=CARTESIAN_POINT('Ctrl Pts',(-0.0140429624864267,-0.0363041575108634,
-0.0121882772977707));
#25299=CARTESIAN_POINT('Ctrl Pts',(-0.014043,-0.0363038407833747,-0.0121820652889604));
#25300=CARTESIAN_POINT('Ctrl Pts',(-0.014043,-0.0363035228772662,-0.012175853286558));
#25301=CARTESIAN_POINT('Origin',(0.006,-0.0412787743898723,-0.0121758532865581));
#25302=CARTESIAN_POINT('',(0.00473550001147424,-0.0374057743898623,-0.0121760236343295));
#25303=CARTESIAN_POINT('',(0.00473550000005949,-0.0373433241596449,-0.0121758410210368));
#25304=CARTESIAN_POINT('',(0.0047355,-0.0412787743898723,-0.0121758532865581));
#25305=CARTESIAN_POINT('',(0.00648836437725255,-0.0369998285136293,-0.013342241080151));
#25306=CARTESIAN_POINT('Ctrl Pts',(0.00473550025703334,-0.0373432743898623,
-0.0121750470376861));
#25307=CARTESIAN_POINT('Ctrl Pts',(0.00473568325203442,-0.0373252099538459,
-0.0118880424416283));
#25308=CARTESIAN_POINT('Ctrl Pts',(0.00483793644636973,-0.0373071455178294,
-0.0116004870680416));
#25309=CARTESIAN_POINT('Ctrl Pts',(0.00501920341792046,-0.0372890810818129,
-0.0113777315448538));
#25310=CARTESIAN_POINT('Ctrl Pts',(0.00512512778104792,-0.0372785250281429,
-0.0112475631157962));
#25311=CARTESIAN_POINT('Ctrl Pts',(0.00525693102794947,-0.0372679689744728,
-0.0111393205108283));
#25312=CARTESIAN_POINT('Ctrl Pts',(0.00540338669147187,-0.0372574129208027,
-0.0110609484430458));
#25313=CARTESIAN_POINT('Ctrl Pts',(0.00564541444099014,-0.0372399683382436,
-0.0109314333752479));
#25314=CARTESIAN_POINT('Ctrl Pts',(0.00593538390252328,-0.0372225237556846,
-0.0108827068727731));
#25315=CARTESIAN_POINT('Ctrl Pts',(0.00620981161123333,-0.0372050791731255,
-0.0109288812187909));
#25316=CARTESIAN_POINT('Ctrl Pts',(0.00638562427830956,-0.037193903265998,
-0.0109584629070323));
#25317=CARTESIAN_POINT('Ctrl Pts',(0.0065544278780534,-0.0371827273588706,
-0.0110258476768364));
#25318=CARTESIAN_POINT('Ctrl Pts',(0.0067008437840681,-0.0371715514517431,
-0.0111233428398959));
#25319=CARTESIAN_POINT('Ctrl Pts',(0.00692938580140116,-0.0371541068691841,
-0.011275523991878));
#25320=CARTESIAN_POINT('Ctrl Pts',(0.00710929857406147,-0.037136662286625,
-0.0115081326048137));
#25321=CARTESIAN_POINT('Ctrl Pts',(0.00719821248300049,-0.0371192177040659,
-0.01177181480376));
#25322=CARTESIAN_POINT('Ctrl Pts',(0.00725517535874009,-0.0371080417969385,
-0.0119407433382553));
#25323=CARTESIAN_POINT('Ctrl Pts',(0.00727550551639853,-0.0370968658898111,
-0.0121213293802333));
#25324=CARTESIAN_POINT('Ctrl Pts',(0.0072587419762938,-0.0370856899826836,
-0.0122963891198857));
#25325=CARTESIAN_POINT('Ctrl Pts',(0.00723164584045649,-0.0370676255466671,
-0.0125793509797095));
#25326=CARTESIAN_POINT('Ctrl Pts',(0.00710450570407131,-0.0370495611106507,
-0.0128555001058568));
#25327=CARTESIAN_POINT('Ctrl Pts',(0.00690294869731533,-0.0370314966746343,
-0.0130610899215979));
#25328=CARTESIAN_POINT('Ctrl Pts',(0.00678516773925136,-0.0370209406209642,
-0.0131812274740249));
#25329=CARTESIAN_POINT('Ctrl Pts',(0.00664306435621841,-0.0370103845672941,
-0.0132774684896714));
#25330=CARTESIAN_POINT('Ctrl Pts',(0.00648836437725186,-0.036999828513624,
-0.0133422410801462));
#25331=CARTESIAN_POINT('',(0.00629997434768202,-0.0370498280494119,-0.0134042879004366));
#25332=CARTESIAN_POINT('Ctrl Pts',(0.00648836437725163,-0.0369998285136324,
-0.0133422410801463));
#25333=CARTESIAN_POINT('Ctrl Pts',(0.00642782011983403,-0.0370199281538104,
-0.0133675908469498));
#25334=CARTESIAN_POINT('Ctrl Pts',(0.00636459046969111,-0.0370367243067544,
-0.0133884784301787));
#25335=CARTESIAN_POINT('Ctrl Pts',(0.00629996344159552,-0.0370494722341879,
-0.0134042596459141));
#25336=CARTESIAN_POINT('Ctrl Pts',(0.0062999658725511,-0.0370498392335843,
-0.013404259015438));
#25337=CARTESIAN_POINT('Ctrl Pts',(0.00657769650495509,-0.0370678301487587,
-0.0133364248152246));
#25338=CARTESIAN_POINT('Ctrl Pts',(0.00683220741234104,-0.0370858210639329,
-0.0131699966762561));
#25339=CARTESIAN_POINT('Ctrl Pts',(0.00711803563641934,-0.0371154591215677,
-0.0127949611817838));
#25340=CARTESIAN_POINT('Ctrl Pts',(0.0071968245232809,-0.0371271062640282,
-0.0126231472652464));
#25341=CARTESIAN_POINT('Ctrl Pts',(0.00729359082809241,-0.0371561129842236,
-0.012177703957702));
#25342=CARTESIAN_POINT('Ctrl Pts',(0.00726184701836556,-0.0371734725619587,
-0.0118867675894431));
#25343=CARTESIAN_POINT('Ctrl Pts',(0.00705957405455359,-0.0372031403991936,
-0.0114582842983591));
#25344=CARTESIAN_POINT('Ctrl Pts',(0.00693355052798508,-0.0372154486586936,
-0.0113012882727189));
#25345=CARTESIAN_POINT('Ctrl Pts',(0.00656697755162586,-0.0372451164959285,
-0.0110131261916979));
#25346=CARTESIAN_POINT('Ctrl Pts',(0.00629140300613193,-0.0372624760736636,
-0.0109145405765421));
#25347=CARTESIAN_POINT('Ctrl Pts',(0.00581761467049966,-0.0372921439108985,
-0.0109092292197413));
#25348=CARTESIAN_POINT('Ctrl Pts',(0.00562134440445418,-0.0373044521703985,
-0.0109539728290903));
#25349=CARTESIAN_POINT('Ctrl Pts',(0.00519265839058833,-0.0373347811246729,
-0.0111622673120118));
#25350=CARTESIAN_POINT('Ctrl Pts',(0.00497856419804905,-0.0373528018194475,
-0.0113769651953921));
#25351=CARTESIAN_POINT('Ctrl Pts',(0.00477692330866625,-0.0373824696566824,
-0.0118049823559411));
#25352=CARTESIAN_POINT('Ctrl Pts',(0.00473549949759476,-0.0373941167991429,
-0.0119907730648006));
#25353=CARTESIAN_POINT('Ctrl Pts',(0.00473550000000466,-0.0374057639416033,
-0.0121758567190455));
#25354=CARTESIAN_POINT('Origin',(0.006,-0.0412787743898723,-0.0121758532865581));
#25355=CARTESIAN_POINT('',(0.00473550017865996,-0.037905744212147,-0.0121763258579932));
#25356=CARTESIAN_POINT('',(0.00473550000001974,-0.0378432065283682,-0.0121758603510965));
#25357=CARTESIAN_POINT('',(0.0047355,-0.0412787743898723,-0.0121758532865581));
#25358=CARTESIAN_POINT('Ctrl Pts',(0.00473550000001974,-0.0378432065283682,
-0.0121758603510965));
#25359=CARTESIAN_POINT('Ctrl Pts',(0.00473549837272941,-0.0378248823123293,
-0.0118845874474744));
#25360=CARTESIAN_POINT('Ctrl Pts',(0.00484035109591382,-0.0378065586722709,
-0.0115938253847216));
#25361=CARTESIAN_POINT('Ctrl Pts',(0.00505105497354914,-0.0377857311838847,
-0.011339169850239));
#25362=CARTESIAN_POINT('Ctrl Pts',(0.00507778670136795,-0.0377832298915577,
-0.0113097962795975));
#25363=CARTESIAN_POINT('Ctrl Pts',(0.00530742653977762,-0.0377627394571817,
-0.011080133980301));
#25364=CARTESIAN_POINT('Ctrl Pts',(0.00558084995454937,-0.037744747444154,
-0.0109491016718024));
#25365=CARTESIAN_POINT('Ctrl Pts',(0.00590979445143813,-0.0377239227486984,
-0.0109137688503134));
#25366=CARTESIAN_POINT('Ctrl Pts',(0.00595486118160276,-0.0377210841223431,
-0.0109113574437742));
#25367=CARTESIAN_POINT('Ctrl Pts',(0.00628617625603332,-0.0377001962616308,
-0.0109113268906981));
#25368=CARTESIAN_POINT('Ctrl Pts',(0.00657310567735865,-0.0376821544149174,
-0.0110127817202872));
#25369=CARTESIAN_POINT('Ctrl Pts',(0.00683015446989156,-0.0376613110970863,
-0.0112210002627126));
#25370=CARTESIAN_POINT('Ctrl Pts',(0.00686291103859084,-0.037658534889714,
-0.0112504997221244));
#25371=CARTESIAN_POINT('Ctrl Pts',(0.00709653430797494,-0.0376376773949044,
-0.0114840596727804));
#25372=CARTESIAN_POINT('Ctrl Pts',(0.00722770261872788,-0.0376195658123854,
-0.0117587590126114));
#25373=CARTESIAN_POINT('Ctrl Pts',(0.00726219389305527,-0.0375987847351207,
-0.012087753553734));
#25374=CARTESIAN_POINT('Ctrl Pts',(0.00726449212525363,-0.0375960237122921,
-0.0121317099105978));
#25375=CARTESIAN_POINT('Ctrl Pts',(0.00726455115590598,-0.0375752932001571,
-0.0124617697191545));
#25376=CARTESIAN_POINT('Ctrl Pts',(0.00716322204369515,-0.0375574337462205,
-0.0127485930585501));
#25377=CARTESIAN_POINT('Ctrl Pts',(0.00695507757776487,-0.0375367589298144,
-0.0130057581485678));
#25378=CARTESIAN_POINT('Ctrl Pts',(0.00692547434391714,-0.0375339946126188,
-0.0130386431468708));
#25379=CARTESIAN_POINT('Ctrl Pts',(0.00669183782908888,-0.0375132881525957,
-0.0132723457410711));
#25380=CARTESIAN_POINT('Ctrl Pts',(0.0064171989090472,-0.0374952700466619,
-0.0134035071006325));
#25381=CARTESIAN_POINT('Ctrl Pts',(0.00608817313528417,-0.037474443859945,
-0.0134380452873456));
#25382=CARTESIAN_POINT('Ctrl Pts',(0.00604412422547741,-0.0374716683136219,
-0.0134403492751711));
#25383=CARTESIAN_POINT('Ctrl Pts',(0.005714859243909,-0.0374508977033079,
-0.0134403792481463));
#25384=CARTESIAN_POINT('Ctrl Pts',(0.00542886542456276,-0.0374328769759303,
-0.0133396240874224));
#25385=CARTESIAN_POINT('Ctrl Pts',(0.00517133362640543,-0.0374119654032364,
-0.0131320479206591));
#25386=CARTESIAN_POINT('Ctrl Pts',(0.00513774826390097,-0.0374091118927495,
-0.013101872008473));
#25387=CARTESIAN_POINT('Ctrl Pts',(0.00490049177048049,-0.0373878470509977,
-0.0128646348103454));
#25388=CARTESIAN_POINT('Ctrl Pts',(0.00476861571028705,-0.037369395015102,
-0.0125852190580139));
#25389=CARTESIAN_POINT('Ctrl Pts',(0.00473737972636936,-0.037348379083743,
-0.012255451925681));
#25390=CARTESIAN_POINT('Ctrl Pts',(0.00473549961401352,-0.0373458519661643,
-0.0122156399924958));
#25391=CARTESIAN_POINT('Ctrl Pts',(0.00473550000005949,-0.0373433241596449,
-0.0121758410210368));
#25392=CARTESIAN_POINT('Ctrl Pts',(0.00473550001147425,-0.0374057743898623,
-0.0121760236343295));
#25393=CARTESIAN_POINT('Ctrl Pts',(0.0047355392500951,-0.0374241027916517,
-0.0124672938705479));
#25394=CARTESIAN_POINT('Ctrl Pts',(0.00484043094080772,-0.0374424311934411,
-0.0127580388597337));
#25395=CARTESIAN_POINT('Ctrl Pts',(0.0050258589565221,-0.0374607595952306,
-0.0129820849390078));
#25396=CARTESIAN_POINT('Ctrl Pts',(0.00505117584857121,-0.0374632620119649,
-0.0130126744396351));
#25397=CARTESIAN_POINT('Ctrl Pts',(0.00507792113320851,-0.0374657644286992,
-0.0130420540382709));
#25398=CARTESIAN_POINT('Ctrl Pts',(0.00510596839668437,-0.0374682668454335,
-0.0130700947205528));
#25399=CARTESIAN_POINT('Ctrl Pts',(0.00530760914168099,-0.0374862575194625,
-0.0132716881512416));
#25400=CARTESIAN_POINT('Ctrl Pts',(0.00558105531573703,-0.0375042481934915,
-0.0134026753626389));
#25401=CARTESIAN_POINT('Ctrl Pts',(0.00586516527539268,-0.0375222388675206,
-0.0134331439637844));
#25402=CARTESIAN_POINT('Ctrl Pts',(0.00591001703228126,-0.0375250790120153,
-0.0134379539686605));
#25403=CARTESIAN_POINT('Ctrl Pts',(0.0059550942114837,-0.03752791915651,
-0.0134403577815941));
#25404=CARTESIAN_POINT('Ctrl Pts',(0.00600012639762061,-0.0375307593010047,
-0.0134403532802408));
#25405=CARTESIAN_POINT('Ctrl Pts',(0.00628643439849026,-0.0375488165210115,
-0.0134403246613003));
#25406=CARTESIAN_POINT('Ctrl Pts',(0.00657335761958725,-0.0375668737410184,
-0.0133388044586746));
#25407=CARTESIAN_POINT('Ctrl Pts',(0.00679614752363937,-0.0375849309610252,
-0.0131582530883714));
#25408=CARTESIAN_POINT('Ctrl Pts',(0.0068303681704066,-0.0375877045595421,
-0.0131305203026657));
#25409=CARTESIAN_POINT('Ctrl Pts',(0.00686311541701947,-0.0375904781580589,
-0.0131010160491334));
#25410=CARTESIAN_POINT('Ctrl Pts',(0.00689421035965139,-0.0375932517565758,
-0.01306991597043));
#25411=CARTESIAN_POINT('Ctrl Pts',(0.00709661267960903,-0.0376113055854924,
-0.012867480218901));
#25412=CARTESIAN_POINT('Ctrl Pts',(0.0072277038809594,-0.0376293594144089,
-0.0125928676077469));
#25413=CARTESIAN_POINT('Ctrl Pts',(0.00725760438561427,-0.0376474132433254,
-0.0123077299686658));
#25414=CARTESIAN_POINT('Ctrl Pts',(0.00726220359784015,-0.0376501902329326,
-0.012263870892344));
#25415=CARTESIAN_POINT('Ctrl Pts',(0.0072645028681267,-0.0376529672225398,
-0.0122198006318683));
#25416=CARTESIAN_POINT('Ctrl Pts',(0.00726449999731215,-0.037655744212147,
-0.0121757708390885));
#25417=CARTESIAN_POINT('Ctrl Pts',(0.0072644813335063,-0.0376737980410633,
-0.0118895233342346));
#25418=CARTESIAN_POINT('Ctrl Pts',(0.00716301179804758,-0.0376918518699797,
-0.0116026446414172));
#25419=CARTESIAN_POINT('Ctrl Pts',(0.00698252940739209,-0.037709905698896,
-0.0113798657152922));
#25420=CARTESIAN_POINT('Ctrl Pts',(0.00695476810947077,-0.0377126826885034,
-0.0113455984822603));
#25421=CARTESIAN_POINT('Ctrl Pts',(0.00692523078390005,-0.0377154596781108,
-0.0113128080448829));
#25422=CARTESIAN_POINT('Ctrl Pts',(0.006894093763348,-0.0377182366677182,
-0.0112816740023303));
#25423=CARTESIAN_POINT('Ctrl Pts',(0.0066916270241954,-0.0377362938877251,
-0.0110792266274528));
#25424=CARTESIAN_POINT('Ctrl Pts',(0.00641695897599585,-0.0377543511077321,
-0.0109481173224277));
#25425=CARTESIAN_POINT('Ctrl Pts',(0.00613176203582361,-0.037772408327739,
-0.0109182368840269));
#25426=CARTESIAN_POINT('Ctrl Pts',(0.00608795563539476,-0.0377751819262558,
-0.010913647232929));
#25427=CARTESIAN_POINT('Ctrl Pts',(0.00604393856281892,-0.0377779555247726,
-0.0109113519482759));
#25428=CARTESIAN_POINT('Ctrl Pts',(0.00599996150268144,-0.0377807291232894,
-0.0109113532871441));
#25429=CARTESIAN_POINT('Ctrl Pts',(0.00571470862671654,-0.0377987197973184,
-0.0109113619715813));
#25430=CARTESIAN_POINT('Ctrl Pts',(0.0054287293523573,-0.0378167104713474,
-0.0110121498534471));
#25431=CARTESIAN_POINT('Ctrl Pts',(0.00520635007387457,-0.0378347011453764,
-0.0111914346536782));
#25432=CARTESIAN_POINT('Ctrl Pts',(0.00517124359134334,-0.0378375412898711,
-0.0112197379144423));
#25433=CARTESIAN_POINT('Ctrl Pts',(0.00513768018197624,-0.0378403814343658,
-0.011249899223349));
#25434=CARTESIAN_POINT('Ctrl Pts',(0.00510585179227583,-0.0378432215788605,
-0.0112817284448141));
#25435=CARTESIAN_POINT('Ctrl Pts',(0.00490045255438429,-0.0378615499806493,
-0.0114871330503616));
#25436=CARTESIAN_POINT('Ctrl Pts',(0.00476859134920546,-0.0378798783824381,
-0.0117665590362431));
#25437=CARTESIAN_POINT('Ctrl Pts',(0.00474112757943725,-0.0378982067842269,
-0.0120566875249212));
#25438=CARTESIAN_POINT('Ctrl Pts',(0.00473737789095569,-0.0379007092009618,
-0.0120962994012715));
#25439=CARTESIAN_POINT('Ctrl Pts',(0.00473550017150005,-0.0379032116176968,
-0.0121360800717304));
#25440=CARTESIAN_POINT('Ctrl Pts',(0.00473550000001176,-0.0379057140344317,
-0.0121758478337256));
#25441=CARTESIAN_POINT('Origin',(0.006,-0.0412787743898723,-0.0121758532865581));
#25442=CARTESIAN_POINT('',(0.00473550020721395,-0.0384058072487128,-0.0121753454415193));
#25443=CARTESIAN_POINT('',(0.0047355000350514,-0.0383440997603813,-0.0121756391001055));
#25444=CARTESIAN_POINT('',(0.0047355,-0.0412787743898723,-0.0121758532865581));
#25445=CARTESIAN_POINT('Ctrl Pts',(0.00473550006772914,-0.0383440997603812,
-0.0121754394182212));
#25446=CARTESIAN_POINT('Ctrl Pts',(0.00473550974249037,-0.0383423607576411,
-0.0121458799331841));
#25447=CARTESIAN_POINT('Ctrl Pts',(0.0047365559087295,-0.0383405947365542,
-0.0121163319997317));
#25448=CARTESIAN_POINT('Ctrl Pts',(0.0047392614796249,-0.0383382365720843,
-0.0120779882914245));
#25449=CARTESIAN_POINT('Ctrl Pts',(0.00473998013712677,-0.038337687364268,
-0.0120691335163025));
#25450=CARTESIAN_POINT('Ctrl Pts',(0.00474148006416988,-0.0383366639294188,
-0.0120527902944031));
#25451=CARTESIAN_POINT('Ctrl Pts',(0.0047422350368259,-0.0383361910629747,
-0.0120452997736119));
#25452=CARTESIAN_POINT('Ctrl Pts',(0.00474401518407334,-0.0383351586666519,
-0.0120290899894216));
#25453=CARTESIAN_POINT('Ctrl Pts',(0.0047450643631106,-0.038334597825695,
-0.0120203738351233));
#25454=CARTESIAN_POINT('Ctrl Pts',(0.00474813704008429,-0.0383330738420285,
-0.0119969092018068));
#25455=CARTESIAN_POINT('Ctrl Pts',(0.00475033031362653,-0.038332102409206,
-0.0119821847900106));
#25456=CARTESIAN_POINT('Ctrl Pts',(0.00476526810161275,-0.0383261241576951,
-0.0118927647516049));
#25457=CARTESIAN_POINT('Ctrl Pts',(0.00478444511683913,-0.0383208866749639,
-0.0118193046409008));
#25458=CARTESIAN_POINT('Ctrl Pts',(0.00483464073841951,-0.0383107214526994,
-0.0116797009722359));
#25459=CARTESIAN_POINT('Ctrl Pts',(0.00486504012193256,-0.0383058093371502,
-0.0116136272923258));
#25460=CARTESIAN_POINT('Ctrl Pts',(0.00491177218601365,-0.0382996515186367,
-0.0115314933720116));
#25461=CARTESIAN_POINT('Ctrl Pts',(0.00492309079993836,-0.0382982414926402,
-0.0115127498675848));
#25462=CARTESIAN_POINT('Ctrl Pts',(0.00494291424779926,-0.038295901457145,
-0.0114817700391427));
#25463=CARTESIAN_POINT('Ctrl Pts',(0.00495115857748836,-0.0382949624196954,
-0.0114693736037016));
#25464=CARTESIAN_POINT('Ctrl Pts',(0.00496724732943143,-0.0382931920156278,
-0.0114460846667635));
#25465=CARTESIAN_POINT('Ctrl Pts',(0.00497504996397839,-0.0382923592752213,
-0.011435165928765));
#25466=CARTESIAN_POINT('Ctrl Pts',(0.0049961039371682,-0.0382901774441414,
-0.0114066736782037));
#25467=CARTESIAN_POINT('Ctrl Pts',(0.00500964307591435,-0.0382888393892673,
-0.0113893179574066));
#25468=CARTESIAN_POINT('Ctrl Pts',(0.00508173465858396,-0.0382820198826257,
-0.0113017192787193));
#25469=CARTESIAN_POINT('Ctrl Pts',(0.00514732679862287,-0.0382768286806568,
-0.0112376254943765));
#25470=CARTESIAN_POINT('Ctrl Pts',(0.00526278284619604,-0.0382683952347556,
-0.0111470034271226));
#25471=CARTESIAN_POINT('Ctrl Pts',(0.00530849448079938,-0.0382651956540521,
-0.0111157400209426));
#25472=CARTESIAN_POINT('Ctrl Pts',(0.00536956440240138,-0.0382609043601922,
-0.0110796069977995));
#25473=CARTESIAN_POINT('Ctrl Pts',(0.00538317380505029,-0.0382599469161624,
-0.0110718920716276));
#25474=CARTESIAN_POINT('Ctrl Pts',(0.00540477383212506,-0.0382584200137224,
-0.0110601714948468));
#25475=CARTESIAN_POINT('Ctrl Pts',(0.00541267020758086,-0.0382578603180602,
-0.0110559944761936));
#25476=CARTESIAN_POINT('Ctrl Pts',(0.00542827956076714,-0.038256749689617,
-0.0110479479516441));
#25477=CARTESIAN_POINT('Ctrl Pts',(0.00543598913283541,-0.0382561990914316,
-0.0110440730811823));
#25478=CARTESIAN_POINT('Ctrl Pts',(0.0054564351153719,-0.038254734657851,
-0.0110340576016111));
#25479=CARTESIAN_POINT('Ctrl Pts',(0.00546923565599044,-0.0382538135520933,
-0.0110280513251737));
#25480=CARTESIAN_POINT('Ctrl Pts',(0.00555449518481482,-0.0382476629121317,
-0.0109897769218209));
#25481=CARTESIAN_POINT('Ctrl Pts',(0.00562974789262337,-0.0382421731018808,
-0.0109641752842107));
#25482=CARTESIAN_POINT('Ctrl Pts',(0.00576761905774788,-0.0382324667285227,
-0.0109313229128065));
#25483=CARTESIAN_POINT('Ctrl Pts',(0.0058293348778137,-0.0382282386702702,
-0.0109213686212666));
#25484=CARTESIAN_POINT('Ctrl Pts',(0.00591736723567329,-0.0382224340613599,
-0.0109137898627642));
#25485=CARTESIAN_POINT('Ctrl Pts',(0.00594325847525168,-0.0382207532952864,
-0.010912360977878));
#25486=CARTESIAN_POINT('Ctrl Pts',(0.00598479543743047,-0.0382180978577547,
-0.0109113481838971));
#25487=CARTESIAN_POINT('Ctrl Pts',(0.00600042020489185,-0.0382171082066521,
-0.010911256832504));
#25488=CARTESIAN_POINT('Ctrl Pts',(0.00603068216275742,-0.0382152081904866,
-0.0109116408092541));
#25489=CARTESIAN_POINT('Ctrl Pts',(0.00604531721747602,-0.0382142969023267,
-0.0109120807751475));
#25490=CARTESIAN_POINT('Ctrl Pts',(0.00608030479958005,-0.0382121347055097,
-0.0109137411783001));
#25491=CARTESIAN_POINT('Ctrl Pts',(0.00610064221660877,-0.0382108912020008,
-0.0109151998652492));
#25492=CARTESIAN_POINT('Ctrl Pts',(0.00622350986786219,-0.0382034428226632,
-0.0109270050015834));
#25493=CARTESIAN_POINT('Ctrl Pts',(0.00632449174572357,-0.0381976321744983,
-0.0109493602552273));
#25494=CARTESIAN_POINT('Ctrl Pts',(0.00647115471914298,-0.0381886661499864,
-0.0110012336919901));
#25495=CARTESIAN_POINT('Ctrl Pts',(0.00651951942254762,-0.038185606567173,
-0.0110218097854021));
#25496=CARTESIAN_POINT('Ctrl Pts',(0.00657804445378298,-0.0381816149945491,
-0.0110511343181702));
#25497=CARTESIAN_POINT('Ctrl Pts',(0.00658953871713479,-0.0381808164229959,
-0.011057116400786));
#25498=CARTESIAN_POINT('Ctrl Pts',(0.00660833675089142,-0.0381794827906792,
-0.0110672697986541));
#25499=CARTESIAN_POINT('Ctrl Pts',(0.00661569478902127,-0.0381789536344057,
-0.0110713394226018));
#25500=CARTESIAN_POINT('Ctrl Pts',(0.00663110056833495,-0.0381778296042569,
-0.0110800619162578));
#25501=CARTESIAN_POINT('Ctrl Pts',(0.0066391384222595,-0.0381772338804882,
-0.0110847305989748));
#25502=CARTESIAN_POINT('Ctrl Pts',(0.00666213560290017,-0.0381755041835899,
-0.0110984295021851));
#25503=CARTESIAN_POINT('Ctrl Pts',(0.00667695964437776,-0.038174358022301,
-0.0111076814185698));
#25504=CARTESIAN_POINT('Ctrl Pts',(0.0067575427830394,-0.0381679729112217,
-0.0111603257992692));
#25505=CARTESIAN_POINT('Ctrl Pts',(0.00681932475879082,-0.0381625114775893,
-0.0112094821687601));
#25506=CARTESIAN_POINT('Ctrl Pts',(0.00692183586976768,-0.0381527912051747,
-0.0113079840958977));
#25507=CARTESIAN_POINT('Ctrl Pts',(0.00696418053016676,-0.0381485170987116,
-0.0113552827441237));
#25508=CARTESIAN_POINT('Ctrl Pts',(0.00701662100396916,-0.0381428976974481,
-0.0114235524685112));
#25509=CARTESIAN_POINT('Ctrl Pts',(0.00702995305424856,-0.0381414345659435,
-0.0114419107834808));
#25510=CARTESIAN_POINT('Ctrl Pts',(0.00705128360070422,-0.0381390328086286,
-0.0114730099104666));
#25511=CARTESIAN_POINT('Ctrl Pts',(0.00705956124976711,-0.038138084062126,
-0.011485551896358));
#25512=CARTESIAN_POINT('Ctrl Pts',(0.00707567633395429,-0.038136201534902,
-0.0115109419770585));
#25513=CARTESIAN_POINT('Ctrl Pts',(0.00708351187440794,-0.0381352679290252,
-0.011523788356514));
#25514=CARTESIAN_POINT('Ctrl Pts',(0.00710263741586795,-0.03813293968717,
-0.0115564417823842));
#25515=CARTESIAN_POINT('Ctrl Pts',(0.00711362477632549,-0.0381315557282313,
-0.0115764203587779));
#25516=CARTESIAN_POINT('Ctrl Pts',(0.00715127971672568,-0.0381266224545275,
-0.0116495022831765));
#25517=CARTESIAN_POINT('Ctrl Pts',(0.0071747378912722,-0.0381231760691956,
-0.0117041731249888));
#25518=CARTESIAN_POINT('Ctrl Pts',(0.00721098982627317,-0.0381168355051107,
-0.0118083570121928));
#25519=CARTESIAN_POINT('Ctrl Pts',(0.00722479651110265,-0.0381139377163221,
-0.0118573832955558));
#25520=CARTESIAN_POINT('Ctrl Pts',(0.00724436401760256,-0.0381085898082324,
-0.0119473484721064));
#25521=CARTESIAN_POINT('Ctrl Pts',(0.00725114472730231,-0.0381061622998086,
-0.0119879902752478));
#25522=CARTESIAN_POINT('Ctrl Pts',(0.00725736262231289,-0.0381028927799663,
-0.0120411263227455));
#25523=CARTESIAN_POINT('Ctrl Pts',(0.00725861585636101,-0.0381021318306581,
-0.0120533860711974));
#25524=CARTESIAN_POINT('Ctrl Pts',(0.00726041354233924,-0.038100842347413,
-0.0120739368713227));
#25525=CARTESIAN_POINT('Ctrl Pts',(0.00726105581173342,-0.0381003188980919,
-0.0120822184105377));
#25526=CARTESIAN_POINT('Ctrl Pts',(0.00726226173103871,-0.0380991831231867,
-0.0121000445148492));
#25527=CARTESIAN_POINT('Ctrl Pts',(0.00726279877888703,-0.0380985695742431,
-0.0121095895847459));
#25528=CARTESIAN_POINT('Ctrl Pts',(0.00726407406333585,-0.0380967294633223,
-0.0121379949103421));
#25529=CARTESIAN_POINT('Ctrl Pts',(0.00726449827568978,-0.0380954883598766,
-0.0121568658637334));
#25530=CARTESIAN_POINT('Ctrl Pts',(0.00726450241961066,-0.0380924622964117,
-0.0122023563976265));
#25531=CARTESIAN_POINT('Ctrl Pts',(0.00726366435025537,-0.0380906639756224,
-0.012228966828908));
#25532=CARTESIAN_POINT('Ctrl Pts',(0.00725534795666524,-0.0380816772887418,
-0.0123606897285524));
#25533=CARTESIAN_POINT('Ctrl Pts',(0.0072355882239628,-0.0380743637674893,
-0.0124646279259903));
#25534=CARTESIAN_POINT('Ctrl Pts',(0.00719490893095668,-0.0380656643001295,
-0.0125904277038998));
#25535=CARTESIAN_POINT('Ctrl Pts',(0.00718584853738683,-0.0380639234751518,
-0.0126156745212516));
#25536=CARTESIAN_POINT('Ctrl Pts',(0.00717018845937666,-0.0380611981985746,
-0.0126552993258125));
#25537=CARTESIAN_POINT('Ctrl Pts',(0.00716411065595122,-0.0380601973130519,
-0.0126698734801178));
#25538=CARTESIAN_POINT('Ctrl Pts',(0.00715190090495607,-0.0380582898184641,
-0.0126976740887945));
#25539=CARTESIAN_POINT('Ctrl Pts',(0.00714581012024887,-0.0380573820285958,
-0.0127109157505791));
#25540=CARTESIAN_POINT('Ctrl Pts',(0.00713085035341409,-0.0380552503813735,
-0.0127420114142857));
#25541=CARTESIAN_POINT('Ctrl Pts',(0.00712178531407539,-0.0380540333452085,
-0.0127597670833557));
#25542=CARTESIAN_POINT('Ctrl Pts',(0.0070840275256758,-0.0380492375398036,
-0.0128295953985292));
#25543=CARTESIAN_POINT('Ctrl Pts',(0.00705209723552133,-0.0380457700394852,
-0.012879832606127));
#25544=CARTESIAN_POINT('Ctrl Pts',(0.00696865375690912,-0.0380376844199474,
-0.0129926849066957));
#25545=CARTESIAN_POINT('Ctrl Pts',(0.00691443349667901,-0.0380331248422485,
-0.0130529583829421));
#25546=CARTESIAN_POINT('Ctrl Pts',(0.00683812656162111,-0.0380269613655469,
-0.0131229637345937));
#25547=CARTESIAN_POINT('Ctrl Pts',(0.00682101083459093,-0.038025592243267,
-0.0131378384270219));
#25548=CARTESIAN_POINT('Ctrl Pts',(0.00679561599377313,-0.0380235642963763,
-0.0131587367196268));
#25549=CARTESIAN_POINT('Ctrl Pts',(0.0067876481868241,-0.0380229284805302,
-0.0131651333129319));
#25550=CARTESIAN_POINT('Ctrl Pts',(0.00677380894466891,-0.0380218232281778,
-0.0131759703513498));
#25551=CARTESIAN_POINT('Ctrl Pts',(0.00676797479343403,-0.038021356932129,
-0.0131804572558482));
#25552=CARTESIAN_POINT('Ctrl Pts',(0.0067535870498199,-0.0380202061219728,
-0.0131913239486484));
#25553=CARTESIAN_POINT('Ctrl Pts',(0.00674499161463305,-0.0380195180268725,
-0.0131976466039016));
#25554=CARTESIAN_POINT('Ctrl Pts',(0.0067154723950112,-0.0380171557553199,
-0.0132187899779236));
#25555=CARTESIAN_POINT('Ctrl Pts',(0.00669417936215945,-0.03801545329348,
-0.0132330819832831));
#25556=CARTESIAN_POINT('Ctrl Pts',(0.00663635987492588,-0.0380108629301987,
-0.0132693908165886));
#25557=CARTESIAN_POINT('Ctrl Pts',(0.00659912921382913,-0.0380079410605348,
-0.013290224005341));
#25558=CARTESIAN_POINT('Ctrl Pts',(0.00648213702032248,-0.037998983091039,
-0.0133481293932859));
#25559=CARTESIAN_POINT('Ctrl Pts',(0.00639949154536015,-0.0379929775869118,
-0.0133788072659486));
#25560=CARTESIAN_POINT('Ctrl Pts',(0.00629260407273725,-0.0379857782761919,
-0.0134062377196916));
#25561=CARTESIAN_POINT('Ctrl Pts',(0.00627074040808769,-0.0379843326697674,
-0.0134112328759312));
#25562=CARTESIAN_POINT('Ctrl Pts',(0.006235533100476,-0.0379820464431884,
-0.0134182969456217));
#25563=CARTESIAN_POINT('Ctrl Pts',(0.0062222699173018,-0.0379811945105474,
-0.0134207380979277));
#25564=CARTESIAN_POINT('Ctrl Pts',(0.00619435538463652,-0.0379794201362291,
-0.0134254155348955));
#25565=CARTESIAN_POINT('Ctrl Pts',(0.00617969859685401,-0.0379784991908188,
-0.0134276073642931));
#25566=CARTESIAN_POINT('Ctrl Pts',(0.00614369541127588,-0.0379762612079752,
-0.0134323459822949));
#25567=CARTESIAN_POINT('Ctrl Pts',(0.00612231574497327,-0.0379749530432353,
-0.0134346071167305));
#25568=CARTESIAN_POINT('Ctrl Pts',(0.00602535041493018,-0.0379690988733585,
-0.013442368215006));
#25569=CARTESIAN_POINT('Ctrl Pts',(0.00594942007337511,-0.0379647422498225,
-0.013441612294665));
#25570=CARTESIAN_POINT('Ctrl Pts',(0.00580057708008604,-0.0379561647576001,
-0.0134267077843195));
#25571=CARTESIAN_POINT('Ctrl Pts',(0.00572793841787632,-0.0379519561222335,
-0.0134129412246025));
#25572=CARTESIAN_POINT('Ctrl Pts',(0.00564277182284718,-0.0379465904651118,
-0.0133889338560403));
#25573=CARTESIAN_POINT('Ctrl Pts',(0.00562869131434428,-0.0379456885315878,
-0.0133846982959242));
#25574=CARTESIAN_POINT('Ctrl Pts',(0.00560636246622745,-0.0379442297987636,
-0.0133775546476917));
#25575=CARTESIAN_POINT('Ctrl Pts',(0.00559806448833046,-0.0379436813524884,
-0.0133748047051537));
#25576=CARTESIAN_POINT('Ctrl Pts',(0.00558146889480631,-0.0379425704680611,
-0.0133691132997638));
#25577=CARTESIAN_POINT('Ctrl Pts',(0.00557317217116028,-0.0379420080029346,
-0.0133661707815615));
#25578=CARTESIAN_POINT('Ctrl Pts',(0.00555082134023114,-0.0379404747815161,
-0.0133579801140248));
#25579=CARTESIAN_POINT('Ctrl Pts',(0.00553682920953142,-0.0379394955745321,
-0.0133525682385566));
#25580=CARTESIAN_POINT('Ctrl Pts',(0.00547690766188492,-0.0379352277019553,
-0.013328157504644));
#25581=CARTESIAN_POINT('Ctrl Pts',(0.00543202702965478,-0.0379318420215861,
-0.0133067098344694));
#25582=CARTESIAN_POINT('Ctrl Pts',(0.00529989308609221,-0.0379214964607171,
-0.013233711800486));
#25583=CARTESIAN_POINT('Ctrl Pts',(0.00521744341414155,-0.0379145436881024,
-0.0131742651574567));
#25584=CARTESIAN_POINT('Ctrl Pts',(0.00512778334700654,-0.0379066208031836,
-0.013091617761053));
#25585=CARTESIAN_POINT('Ctrl Pts',(0.00511294791782444,-0.0379052942548962,
-0.0130772550537105));
#25586=CARTESIAN_POINT('Ctrl Pts',(0.00508827772630164,-0.0379030597615259,
-0.0130521717353925));
#25587=CARTESIAN_POINT('Ctrl Pts',(0.00507826445866174,-0.0379021442860712,
-0.0130416333670979));
#25588=CARTESIAN_POINT('Ctrl Pts',(0.00505795325030473,-0.0379002682191274,
-0.0130195051294584));
#25589=CARTESIAN_POINT('Ctrl Pts',(0.00504768223712076,-0.0378993088280312,
-0.0130078938034488));
#25590=CARTESIAN_POINT('Ctrl Pts',(0.00502124101069876,-0.0378968077630075,
-0.0129768708898569));
#25591=CARTESIAN_POINT('Ctrl Pts',(0.00500543411081777,-0.0378952804617343,
-0.0129571580784358));
#25592=CARTESIAN_POINT('Ctrl Pts',(0.00494841777285435,-0.0378896245345087,
-0.0128815159692503));
#25593=CARTESIAN_POINT('Ctrl Pts',(0.00491124810562928,-0.0378856370318531,
-0.0128226959007852));
#25594=CARTESIAN_POINT('Ctrl Pts',(0.00484562476919585,-0.0378775073953288,
-0.0126970131589097));
#25595=CARTESIAN_POINT('Ctrl Pts',(0.00481771841867601,-0.0378733786250769,
-0.0126301634951455));
#25596=CARTESIAN_POINT('Ctrl Pts',(0.00479117410996577,-0.0378680993773812,
-0.012547227339326));
#25597=CARTESIAN_POINT('Ctrl Pts',(0.004786915965074,-0.0378671928717547,
-0.0125330728285829));
#25598=CARTESIAN_POINT('Ctrl Pts',(0.00478053159706622,-0.0378657285249005,
-0.0125104183186729));
#25599=CARTESIAN_POINT('Ctrl Pts',(0.00477824380512941,-0.0378651791502191,
-0.0125019648266605));
#25600=CARTESIAN_POINT('Ctrl Pts',(0.00477383729648801,-0.0378640685188387,
-0.0124849850602577));
#25601=CARTESIAN_POINT('Ctrl Pts',(0.00477171926747377,-0.0378635072661903,
-0.0124764591088708));
#25602=CARTESIAN_POINT('Ctrl Pts',(0.00476624464236355,-0.0378619807567758,
-0.0124533970255423));
#25603=CARTESIAN_POINT('Ctrl Pts',(0.00476305627478935,-0.0378610071639272,
-0.012438822839294));
#25604=CARTESIAN_POINT('Ctrl Pts',(0.00474377988958161,-0.0378545343673484,
-0.0123425839117136));
#25605=CARTESIAN_POINT('Ctrl Pts',(0.0047355318393687,-0.0378487591530695,
-0.012259561528838));
#25606=CARTESIAN_POINT('Ctrl Pts',(0.00473550009199991,-0.0378430687134126,
-0.0121763356430332));
#25607=CARTESIAN_POINT('Ctrl Pts',(0.00473550035730815,-0.0379057743898623,
-0.0121768038822607));
#25608=CARTESIAN_POINT('Ctrl Pts',(0.00473571932336438,-0.0379241093214222,
-0.0124680765012176));
#25609=CARTESIAN_POINT('Ctrl Pts',(0.00484079203787322,-0.037942444252982,
-0.0127587586814847));
#25610=CARTESIAN_POINT('Ctrl Pts',(0.00502636095174794,-0.0379607791845419,
-0.0129826910978429));
#25611=CARTESIAN_POINT('Ctrl Pts',(0.00505164742211236,-0.0379632775863154,
-0.0130132051548131));
#25612=CARTESIAN_POINT('Ctrl Pts',(0.00507835596367472,-0.0379657759880888,
-0.0130425131526919));
#25613=CARTESIAN_POINT('Ctrl Pts',(0.00510636083680849,-0.0379682743898623,
-0.0130704868964847));
#25614=CARTESIAN_POINT('Ctrl Pts',(0.00530809385253593,-0.0379862716191963,
-0.0132719956721024));
#25615=CARTESIAN_POINT('Ctrl Pts',(0.00558160283114279,-0.0380042688485303,
-0.0134028631907799));
#25616=CARTESIAN_POINT('Ctrl Pts',(0.00586573071169492,-0.0380222660778642,
-0.0134332044738634));
#25617=CARTESIAN_POINT('Ctrl Pts',(0.00591050517133018,-0.0380251021818636,
-0.0134379858228534));
#25618=CARTESIAN_POINT('Ctrl Pts',(0.00595550318120118,-0.0380279382858629,
-0.0134403694067042));
#25619=CARTESIAN_POINT('Ctrl Pts',(0.00600045576433034,-0.0380307743898623,
-0.0134403532044224));
#25620=CARTESIAN_POINT('Ctrl Pts',(0.00628676884007308,-0.0380488381718,
-0.013440250008459));
#25621=CARTESIAN_POINT('Ctrl Pts',(0.00657366937610735,-0.0380669019537376,
-0.0133386517033703));
#25622=CARTESIAN_POINT('Ctrl Pts',(0.00679641352477234,-0.0380849657356753,
-0.0131580374584728));
#25623=CARTESIAN_POINT('Ctrl Pts',(0.00683056480992067,-0.038087735287071,
-0.0131303455589714));
#25624=CARTESIAN_POINT('Ctrl Pts',(0.00686324754914644,-0.0380905048384666,
-0.0131008889919923));
#25625=CARTESIAN_POINT('Ctrl Pts',(0.00689428383739052,-0.0380932743898623,
-0.013069842474514));
#25626=CARTESIAN_POINT('Ctrl Pts',(0.00709667301988905,-0.0381113347725488,
-0.0128673865866694));
#25627=CARTESIAN_POINT('Ctrl Pts',(0.00722774192794643,-0.0381293951552352,
-0.0125927582940303));
#25628=CARTESIAN_POINT('Ctrl Pts',(0.00725761654397931,-0.0381474555379217,
-0.012307613972309));
#25629=CARTESIAN_POINT('Ctrl Pts',(0.00726220342551396,-0.0381502284885686,
-0.0122638335527523));
#25630=CARTESIAN_POINT('Ctrl Pts',(0.0072644986415305,-0.0381530014392154,
-0.0122198429168089));
#25631=CARTESIAN_POINT('Ctrl Pts',(0.00726449999939651,-0.0381557743898623,
-0.0121758923536699));
#25632=CARTESIAN_POINT('Ctrl Pts',(0.00726450884325376,-0.0381738347725488,
-0.0118896398772787));
#25633=CARTESIAN_POINT('Ctrl Pts',(0.00716306358962789,-0.0381918951552352,
-0.0116027477647218));
#25634=CARTESIAN_POINT('Ctrl Pts',(0.00698259788633582,-0.0382099555379217,
-0.0113799502498957));
#25635=CARTESIAN_POINT('Ctrl Pts',(0.00695488958705057,-0.0382127284885686,
-0.011345742419221));
#25636=CARTESIAN_POINT('Ctrl Pts',(0.00692541153612805,-0.0382155014392154,
-0.011313005901592));
#25637=CARTESIAN_POINT('Ctrl Pts',(0.00689433907581853,-0.0382182743898623,
-0.0112819193586506));
#25638=CARTESIAN_POINT('Ctrl Pts',(0.00669192431307087,-0.0382363381718,
-0.0110794128576707));
#25639=CARTESIAN_POINT('Ctrl Pts',(0.00641728721568636,-0.0382544019537377,
-0.0109482278968322));
#25640=CARTESIAN_POINT('Ctrl Pts',(0.00613209413111397,-0.0382724657356753,
-0.0109182717223941));
#25641=CARTESIAN_POINT('Ctrl Pts',(0.00608836813242027,-0.038275235287071,
-0.0109136788212502));
#25642=CARTESIAN_POINT('Ctrl Pts',(0.00604443161399198,-0.0382780048384666,
-0.0109113719338119));
#25643=CARTESIAN_POINT('Ctrl Pts',(0.00600053389854783,-0.0382807743898623,
-0.0109113533992697));
#25644=CARTESIAN_POINT('Ctrl Pts',(0.00571527569632501,-0.0382987716191963,
-0.0109112329572345));
#25645=CARTESIAN_POINT('Ctrl Pts',(0.00542924685311941,-0.0383167688485304,
-0.0110118949021592));
#25646=CARTESIAN_POINT('Ctrl Pts',(0.00520678506047186,-0.0383347660778645,
-0.0111910841208602));
#25647=CARTESIAN_POINT('Ctrl Pts',(0.00517172828767079,-0.0383376021818637,
-0.011219321759574));
#25648=CARTESIAN_POINT('Ctrl Pts',(0.00513820829682603,-0.038340438285863,
-0.0112494115449752));
#25649=CARTESIAN_POINT('Ctrl Pts',(0.00510641611846888,-0.0383432743898623,
-0.0112811644598324));
#25650=CARTESIAN_POINT('Ctrl Pts',(0.00490088507501357,-0.0383616093214222,
-0.0114864416714168));
#25651=CARTESIAN_POINT('Ctrl Pts',(0.00476884759532968,-0.0383799442529821,
-0.0117657873933289));
#25652=CARTESIAN_POINT('Ctrl Pts',(0.00474120230281209,-0.038398279184542,
-0.0120559007644737));
#25653=CARTESIAN_POINT('Ctrl Pts',(0.00473743522860036,-0.0384007775863154,
-0.0120954329415422));
#25654=CARTESIAN_POINT('Ctrl Pts',(0.00473553270825591,-0.0384032759880889,
-0.012135134417089));
#25655=CARTESIAN_POINT('Ctrl Pts',(0.00473550041846002,-0.0384057743898623,
-0.012174824556656));
#25656=CARTESIAN_POINT('Origin',(0.006,-0.0412787743898723,-0.0121758532865581));
#25657=CARTESIAN_POINT('',(0.00473550000000009,-0.0389057758757622,-0.012175852808333));
#25658=CARTESIAN_POINT('',(0.0047355,-0.0388421555262979,-0.0121758532866954));
#25659=CARTESIAN_POINT('',(0.0047355,-0.0412787743898723,-0.0121758532865581));
#25660=CARTESIAN_POINT('Ctrl Pts',(0.0047355,-0.0388421555262979,-0.0121758532868327));
#25661=CARTESIAN_POINT('Ctrl Pts',(0.00473549999999784,-0.0388415399821669,
-0.0121659214854022));
#25662=CARTESIAN_POINT('Ctrl Pts',(0.00473561701135706,-0.0388409279571186,
-0.0121559896111397));
#25663=CARTESIAN_POINT('Ctrl Pts',(0.00473647966409911,-0.0388386844031961,
-0.0121193870295771));
#25664=CARTESIAN_POINT('Ctrl Pts',(0.00473795231692135,-0.0388370746953837,
-0.0120927396953085));
#25665=CARTESIAN_POINT('Ctrl Pts',(0.00474890807120219,-0.0388295530808997,
-0.011966925207738));
#25666=CARTESIAN_POINT('Ctrl Pts',(0.00476924275858377,-0.0388239662038009,
-0.0118690656231402));
#25667=CARTESIAN_POINT('Ctrl Pts',(0.0048147111782553,-0.0388156631344287,
-0.0117331810071438));
#25668=CARTESIAN_POINT('Ctrl Pts',(0.00483070807381028,-0.0388130966890162,
-0.0116925066000963));
#25669=CARTESIAN_POINT('Ctrl Pts',(0.00485405383383625,-0.0388096527575508,
-0.0116411286413657));
#25670=CARTESIAN_POINT('Ctrl Pts',(0.00485950769434488,-0.0388088658048069,
-0.0116295929694698));
#25671=CARTESIAN_POINT('Ctrl Pts',(0.00486881390676934,-0.0388075479586308,
-0.0116106561080116));
#25672=CARTESIAN_POINT('Ctrl Pts',(0.00487256677516668,-0.0388070227432049,
-0.0116032066689159));
#25673=CARTESIAN_POINT('Ctrl Pts',(0.00488073567539052,-0.0388058915850138,
-0.0115873830332447));
#25674=CARTESIAN_POINT('Ctrl Pts',(0.00488517243658042,-0.0388052845265961,
-0.0115790205141998));
#25675=CARTESIAN_POINT('Ctrl Pts',(0.00489838371634503,-0.0388034994482989,
-0.0115547809255278));
#25676=CARTESIAN_POINT('Ctrl Pts',(0.00490740618781849,-0.0388023081820033,
-0.0115390424823475));
#25677=CARTESIAN_POINT('Ctrl Pts',(0.00496020278593633,-0.038795510442991,
-0.0114513728159497));
#25678=CARTESIAN_POINT('Ctrl Pts',(0.00501073631349636,-0.0387896581593104,
-0.0113837630720211));
#25679=CARTESIAN_POINT('Ctrl Pts',(0.00510973743408634,-0.038779662886571,
-0.0112756967936718));
#25680=CARTESIAN_POINT('Ctrl Pts',(0.00515521074677647,-0.0387754799592953,
-0.0112328887650736));
#25681=CARTESIAN_POINT('Ctrl Pts',(0.00521942814439156,-0.0387701140558503,
-0.0111808257928679));
#25682=CARTESIAN_POINT('Ctrl Pts',(0.00523549907371174,-0.0387688111453847,
-0.0111684255995347));
#25683=CARTESIAN_POINT('Ctrl Pts',(0.00526372769663689,-0.0387665888654258,
-0.0111477093488344));
#25684=CARTESIAN_POINT('Ctrl Pts',(0.0052757445782097,-0.038765662667888,
-0.0111392091941519));
#25685=CARTESIAN_POINT('Ctrl Pts',(0.00530100112828759,-0.0387637554555407,
-0.0111219975620968));
#25686=CARTESIAN_POINT('Ctrl Pts',(0.00531426170359364,-0.0387627758460356,
-0.0111133212474295));
#25687=CARTESIAN_POINT('Ctrl Pts',(0.00535027879207148,-0.0387601699351522,
-0.0110907107018007));
#25688=CARTESIAN_POINT('Ctrl Pts',(0.00537331958859258,-0.0387585602274808,
-0.0110772433078822));
#25689=CARTESIAN_POINT('Ctrl Pts',(0.00548431338809092,-0.0387510386131901,
-0.0110169964038892));
#25690=CARTESIAN_POINT('Ctrl Pts',(0.00557716023196362,-0.0387454517361603,
-0.0109799901722844));
#25691=CARTESIAN_POINT('Ctrl Pts',(0.00571558786153034,-0.0387371486665608,
-0.0109429793781871));
#25692=CARTESIAN_POINT('Ctrl Pts',(0.005758339787551,-0.0387345822208101,
-0.0109338919464912));
#25693=CARTESIAN_POINT('Ctrl Pts',(0.00581407324498526,-0.0387311382889725,
-0.0109250318349941));
#25694=CARTESIAN_POINT('Ctrl Pts',(0.00582670382954977,-0.0387303513362258,
-0.0109232194731103));
#25695=CARTESIAN_POINT('Ctrl Pts',(0.00584763287841279,-0.0387290334900665,
-0.0109205389480718));
#25696=CARTESIAN_POINT('Ctrl Pts',(0.00585591672686075,-0.0387285082746606,
-0.0109195611885365));
#25697=CARTESIAN_POINT('Ctrl Pts',(0.00587362156668634,-0.0387273771165653,
-0.0109176488679723));
#25698=CARTESIAN_POINT('Ctrl Pts',(0.00588304424903874,-0.0387267700582242,
-0.0109167380390071));
#25699=CARTESIAN_POINT('Ctrl Pts',(0.00591055033710448,-0.0387249849802696,
-0.0109143906150102));
#25700=CARTESIAN_POINT('Ctrl Pts',(0.00592865484816423,-0.0387237937142453,
-0.0109132373085436));
#25701=CARTESIAN_POINT('Ctrl Pts',(0.00603090397030049,-0.0387169959796343,
-0.0109089297952436));
#25702=CARTESIAN_POINT('Ctrl Pts',(0.00611517146583091,-0.0387111437003502,
-0.0109137973953982));
#25703=CARTESIAN_POINT('Ctrl Pts',(0.00625991662077184,-0.0387011484259906,
-0.0109367840762009));
#25704=CARTESIAN_POINT('Ctrl Pts',(0.00632070451410851,-0.0386969654931938,
-0.0109511085802484));
#25705=CARTESIAN_POINT('Ctrl Pts',(0.00639954993701431,-0.0386915995844553,
-0.0109759649655577));
#25706=CARTESIAN_POINT('Ctrl Pts',(0.00641875694040768,-0.038690296673864,
-0.0109825323591412));
#25707=CARTESIAN_POINT('Ctrl Pts',(0.00645160591917498,-0.038688074393787,
-0.0109946551849937));
#25708=CARTESIAN_POINT('Ctrl Pts',(0.00646532380762949,-0.0386871481962535,
-0.0109999916261736));
#25709=CARTESIAN_POINT('Ctrl Pts',(0.00649361022399706,-0.0386852409840039,
-0.0110115679876082));
#25710=CARTESIAN_POINT('Ctrl Pts',(0.00650816094992898,-0.0386842613745905,
-0.0110178447398494));
#25711=CARTESIAN_POINT('Ctrl Pts',(0.00654688539386126,-0.0386816554641844,
-0.0110354198413622));
#25712=CARTESIAN_POINT('Ctrl Pts',(0.00657082646709165,-0.0386800457568886,
-0.0110472127913562));
#25713=CARTESIAN_POINT('Ctrl Pts',(0.00668229558573361,-0.0386725241427527,
-0.0111065756376862));
#25714=CARTESIAN_POINT('Ctrl Pts',(0.00676436989454704,-0.0386669372655562,
-0.0111636177792272));
#25715=CARTESIAN_POINT('Ctrl Pts',(0.00687158555002229,-0.0386586341956333,
-0.0112586799290506));
#25716=CARTESIAN_POINT('Ctrl Pts',(0.0069027435334229,-0.0386560677497,
-0.0112893310129275));
#25717=CARTESIAN_POINT('Ctrl Pts',(0.00694087113027838,-0.0386526238176475,
-0.0113309363805012));
#25718=CARTESIAN_POINT('Ctrl Pts',(0.00694934865823438,-0.0386518368648792,
-0.0113404730387649));
#25719=CARTESIAN_POINT('Ctrl Pts',(0.0069631269446376,-0.0386505190186614,
-0.0113564533129963));
#25720=CARTESIAN_POINT('Ctrl Pts',(0.00696851106549649,-0.0386499938032181,
-0.0113628242949652));
#25721=CARTESIAN_POINT('Ctrl Pts',(0.00697987040099121,-0.0386488626449133,
-0.0113765386647298));
#25722=CARTESIAN_POINT('Ctrl Pts',(0.00698582675136782,-0.0386482555863983,
-0.0113838965512263));
#25723=CARTESIAN_POINT('Ctrl Pts',(0.00700295437633025,-0.0386464705077923,
-0.0114055469623153));
#25724=CARTESIAN_POINT('Ctrl Pts',(0.00701390097689067,-0.0386452792412829,
-0.0114200133246907));
#25725=CARTESIAN_POINT('Ctrl Pts',(0.00707388407121027,-0.0386384814994386,
-0.0115029318892635));
#25726=CARTESIAN_POINT('Ctrl Pts',(0.00711629669748798,-0.0386326292130035,
-0.0115759105899205));
#25727=CARTESIAN_POINT('Ctrl Pts',(0.00717694776053939,-0.0386226339415916,
-0.0117093309288648));
#25728=CARTESIAN_POINT('Ctrl Pts',(0.00719852268134543,-0.0386184510180771,
-0.0117679386548639));
#25729=CARTESIAN_POINT('Ctrl Pts',(0.00722127077262911,-0.0386130851181356,
-0.0118474178516646));
#25730=CARTESIAN_POINT('Ctrl Pts',(0.00722638494385483,-0.0386117822076683,
-0.0118670618029199));
#25731=CARTESIAN_POINT('Ctrl Pts',(0.00723438836302389,-0.0386095599275956,
-0.0119011493902246));
#25732=CARTESIAN_POINT('Ctrl Pts',(0.00723750215415133,-0.0386086337299485,
-0.0119155355790618));
#25733=CARTESIAN_POINT('Ctrl Pts',(0.00724344519666881,-0.0386067265172649,
-0.0119455158088585));
#25734=CARTESIAN_POINT('Ctrl Pts',(0.00724623390578158,-0.0386057469075351,
-0.0119611153124359));
#25735=CARTESIAN_POINT('Ctrl Pts',(0.00725292944074801,-0.0386031409957286,
-0.0120031110091382));
#25736=CARTESIAN_POINT('Ctrl Pts',(0.00725629537802834,-0.0386015312873746,
-0.0120295859045205));
#25737=CARTESIAN_POINT('Ctrl Pts',(0.00726825072594748,-0.0385940096722593,
-0.0121553093567262));
#25738=CARTESIAN_POINT('Ctrl Pts',(0.00726593088788882,-0.0385884227950085,
-0.0122552324104382));
#25739=CARTESIAN_POINT('Ctrl Pts',(0.00724576087682851,-0.0385801197262389,
-0.0123970956294928));
#25740=CARTESIAN_POINT('Ctrl Pts',(0.00723737584686981,-0.0385775532816926,
-0.0124399908268264));
#25741=CARTESIAN_POINT('Ctrl Pts',(0.00722369669097977,-0.038574109351185,
-0.0124947411514895));
#25742=CARTESIAN_POINT('Ctrl Pts',(0.00722041672163876,-0.0385733223984535,
-0.0125070723361646));
#25743=CARTESIAN_POINT('Ctrl Pts',(0.0072146849627803,-0.0385720045522725,
-0.0125273789177083));
#25744=CARTESIAN_POINT('Ctrl Pts',(0.00721233973686755,-0.0385714793368279,
-0.01253538379649));
#25745=CARTESIAN_POINT('Ctrl Pts',(0.00720716411001813,-0.0385703481786079,
-0.0125524229067683));
#25746=CARTESIAN_POINT('Ctrl Pts',(0.00720431121107332,-0.0385697411201799,
-0.0125614493980619));
#25747=CARTESIAN_POINT('Ctrl Pts',(0.00719569668621866,-0.0385679560417007,
-0.0125876769729951));
#25748=CARTESIAN_POINT('Ctrl Pts',(0.0071896661421002,-0.0385667647752283,
-0.0126047865088812));
#25749=CARTESIAN_POINT('Ctrl Pts',(0.007153577568203,-0.0385599670326137,
-0.0127005522492241));
#25750=CARTESIAN_POINT('Ctrl Pts',(0.00711609060292571,-0.0385541147452527,
-0.0127761793013874));
#25751=CARTESIAN_POINT('Ctrl Pts',(0.00703824290463211,-0.0385441194736393,
-0.0129003536737599));
#25752=CARTESIAN_POINT('Ctrl Pts',(0.00700125203703263,-0.0385399365507607,
-0.0129506728278678));
#25753=CARTESIAN_POINT('Ctrl Pts',(0.00694749763281084,-0.038534570651652,
-0.0130134811100347));
#25754=CARTESIAN_POINT('Ctrl Pts',(0.0069339315050433,-0.0385332677413893,
-0.0130285807662616));
#25755=CARTESIAN_POINT('Ctrl Pts',(0.00690991020983994,-0.0385310454617495,
-0.0130540561511366));
#25756=CARTESIAN_POINT('Ctrl Pts',(0.00689962679789605,-0.0385301192643296,
-0.0130645875071032));
#25757=CARTESIAN_POINT('Ctrl Pts',(0.00687789548893505,-0.03852821205221,
-0.0130860789844425));
#25758=CARTESIAN_POINT('Ctrl Pts',(0.00686642067633903,-0.0385272324428148,
-0.0130970082989701));
#25759=CARTESIAN_POINT('Ctrl Pts',(0.00683508132462889,-0.0385246265322215,
-0.0131257539436761));
#25760=CARTESIAN_POINT('Ctrl Pts',(0.00681485283729608,-0.0385230168247289,
-0.0131431624805026));
#25761=CARTESIAN_POINT('Ctrl Pts',(0.00671657034115043,-0.0385154952111455,
-0.013222471125496));
#25762=CARTESIAN_POINT('Ctrl Pts',(0.00663193729418693,-0.0385099083346477,
-0.0132756429537757));
#25763=CARTESIAN_POINT('Ctrl Pts',(0.00650247435055353,-0.03850160526459,
-0.0133370543317233));
#25764=CARTESIAN_POINT('Ctrl Pts',(0.00646206775598794,-0.0384990388177094,
-0.0133537161899485));
#25765=CARTESIAN_POINT('Ctrl Pts',(0.00640885218508829,-0.0384955948846451,
-0.0133724998311427));
#25766=CARTESIAN_POINT('Ctrl Pts',(0.00639675688910823,-0.0384948079319144,
-0.0133765643276606));
#25767=CARTESIAN_POINT('Ctrl Pts',(0.00637665654127162,-0.0384934900858757,
-0.0133829819781396));
#25768=CARTESIAN_POINT('Ctrl Pts',(0.00636868566545609,-0.0384929648705775,
-0.0133854402843424));
#25769=CARTESIAN_POINT('Ctrl Pts',(0.00635161768346804,-0.0384918337129794,
-0.013390519854762));
#25770=CARTESIAN_POINT('Ctrl Pts',(0.0063425146265189,-0.0384912266550322,
-0.0133931180830601));
#25771=CARTESIAN_POINT('Ctrl Pts',(0.00631588531458509,-0.038489441578788,
-0.0134003963773452));
#25772=CARTESIAN_POINT('Ctrl Pts',(0.00629828712019421,-0.0384882503141049,
-0.0134048016303946));
#25773=CARTESIAN_POINT('Ctrl Pts',(0.00619849917277322,-0.0384814526010313,
-0.0134275114729418));
#25774=CARTESIAN_POINT('Ctrl Pts',(0.00611473927361995,-0.038475600343232,
-0.0134379485234275));
#25775=CARTESIAN_POINT('Ctrl Pts',(0.00596822298919365,-0.0384656050607384,
-0.0134414912394956));
#25776=CARTESIAN_POINT('Ctrl Pts',(0.00590584703805779,-0.038461422100753,
-0.0134383849690581));
#25777=CARTESIAN_POINT('Ctrl Pts',(0.00582380792404518,-0.0384560561659801,
-0.0134281825115457));
#25778=CARTESIAN_POINT('Ctrl Pts',(0.00580373045855541,-0.0384547532547983,
-0.0134251933036864));
#25779=CARTESIAN_POINT('Ctrl Pts',(0.00576923181709878,-0.0384525309742051,
-0.0134192047682781));
#25780=CARTESIAN_POINT('Ctrl Pts',(0.00575477554214615,-0.0384516047767307,
-0.0134164345436876));
#25781=CARTESIAN_POINT('Ctrl Pts',(0.00572486312737236,-0.0384496975650591,
-0.0134101591690809));
#25782=CARTESIAN_POINT('Ctrl Pts',(0.0057094178421176,-0.0384487179561564,
-0.0134066145771941));
#25783=CARTESIAN_POINT('Ctrl Pts',(0.00566815541335507,-0.0384461120483219,
-0.0133963250172466));
#25784=CARTESIAN_POINT('Ctrl Pts',(0.00564247772660968,-0.0384445023430334,
-0.0133890515577103));
#25785=CARTESIAN_POINT('Ctrl Pts',(0.00552211793547214,-0.0384369807299063,
-0.0133508046434737));
#25786=CARTESIAN_POINT('Ctrl Pts',(0.00543108847832245,-0.0384313938519931,
-0.0133095294927673));
#25787=CARTESIAN_POINT('Ctrl Pts',(0.00530846233895228,-0.0384230907802832,
-0.0132354022490875));
#25788=CARTESIAN_POINT('Ctrl Pts',(0.00527227936838826,-0.0384205243331082,
-0.0132108848382613));
#25789=CARTESIAN_POINT('Ctrl Pts',(0.00522726237521781,-0.0384170803996228,
-0.013176852599856));
#25790=CARTESIAN_POINT('Ctrl Pts',(0.0052172013724121,-0.0384162934467488,
-0.0131690045046441));
#25791=CARTESIAN_POINT('Ctrl Pts',(0.00520076267597678,-0.0384149756002612,
-0.0131557765121691));
#25792=CARTESIAN_POINT('Ctrl Pts',(0.00519431611448294,-0.0384144503846522,
-0.0131504831146578));
#25793=CARTESIAN_POINT('Ctrl Pts',(0.00518066593349501,-0.0384133192253875,
-0.0131390467017707));
#25794=CARTESIAN_POINT('Ctrl Pts',(0.00517347824851354,-0.0384127121660697,
-0.0131328860179246));
#25795=CARTESIAN_POINT('Ctrl Pts',(0.00515272088123464,-0.0384109270845197,
-0.0131146862910231));
#25796=CARTESIAN_POINT('Ctrl Pts',(0.00513934076934827,-0.0384097358158363,
-0.0131024356783558));
#25797=CARTESIAN_POINT('Ctrl Pts',(0.00506536359133869,-0.0384029380420105,
-0.0130317183837278));
#25798=CARTESIAN_POINT('Ctrl Pts',(0.00501046365503673,-0.038397085724011,
-0.0129676029021016));
#25799=CARTESIAN_POINT('Ctrl Pts',(0.00492670594677885,-0.0383870904657682,
-0.0128473359321362));
#25800=CARTESIAN_POINT('Ctrl Pts',(0.00489489778060487,-0.0383829075833806,
-0.0127935910754407));
#25801=CARTESIAN_POINT('Ctrl Pts',(0.00485816483979804,-0.0383775417223395,
-0.0127195302141824));
#25802=CARTESIAN_POINT('Ctrl Pts',(0.00484958576971037,-0.0383762388123558,
-0.0127011335064036));
#25803=CARTESIAN_POINT('Ctrl Pts',(0.00483555547002561,-0.0383740165321598,
-0.0126690528387957));
#25804=CARTESIAN_POINT('Ctrl Pts',(0.00482989377190817,-0.0383730903339322,
-0.0126554659486419));
#25805=CARTESIAN_POINT('Ctrl Pts',(0.00481863200601154,-0.0383711831191316,
-0.0126270527705208));
#25806=CARTESIAN_POINT('Ctrl Pts',(0.00481307082698056,-0.0383702035078833,
-0.0126122137848643));
#25807=CARTESIAN_POINT('Ctrl Pts',(0.00479889810317191,-0.0383675975894454,
-0.0125721187479176));
#25808=CARTESIAN_POINT('Ctrl Pts',(0.0047908043311595,-0.0383659878760986,
-0.0125466875661106));
#25809=CARTESIAN_POINT('Ctrl Pts',(0.00475633134804366,-0.038358466256127,
-0.0124251928999911));
#25810=CARTESIAN_POINT('Ctrl Pts',(0.00474055999840928,-0.0383528793783922,
-0.0123264950548821));
#25811=CARTESIAN_POINT('Ctrl Pts',(0.00473583885136971,-0.0383461116660483,
-0.0122097969690597));
#25812=CARTESIAN_POINT('Ctrl Pts',(0.00473549444331784,-0.038345110727623,
-0.0121926237908312));
#25813=CARTESIAN_POINT('Ctrl Pts',(0.00473550006772914,-0.0383440997603812,
-0.0121754394182212));
#25814=CARTESIAN_POINT('Ctrl Pts',(0.00473550000000377,-0.0384058394797894,
-0.0121758563747875));
#25815=CARTESIAN_POINT('Ctrl Pts',(0.004735500711359,-0.0384241673526885,
-0.0124671264108875));
#25816=CARTESIAN_POINT('Ctrl Pts',(0.00484035380825948,-0.0384424952255876,
-0.0127578851096797));
#25817=CARTESIAN_POINT('Ctrl Pts',(0.00502575196577548,-0.0384608230984867,
-0.0129819556484264));
#25818=CARTESIAN_POINT('Ctrl Pts',(0.00505106886622003,-0.0384633258468406,
-0.0130125534256536));
#25819=CARTESIAN_POINT('Ctrl Pts',(0.00507781477904601,-0.0384658285951946,
-0.0130419411008095));
#25820=CARTESIAN_POINT('Ctrl Pts',(0.00510586324542223,-0.0384683313435485,
-0.013069989581601));
#25821=CARTESIAN_POINT('Ctrl Pts',(0.00530747996683213,-0.0384863214864272,
-0.0132716064066304));
#25822=CARTESIAN_POINT('Ctrl Pts',(0.00558091029438798,-0.0385043116293058,
-0.0134026257481341));
#25823=CARTESIAN_POINT('Ctrl Pts',(0.00586501629191922,-0.0385223017721845,
-0.0134331279775277));
#25824=CARTESIAN_POINT('Ctrl Pts',(0.00590987402025746,-0.0385251422505589,
-0.0134379439994764));
#25825=CARTESIAN_POINT('Ctrl Pts',(0.00595495752153627,-0.0385279827289332,
-0.0134403531534092));
#25826=CARTESIAN_POINT('Ctrl Pts',(0.00599999626189027,-0.0385308232073076,
-0.0134403532865526));
#25827=CARTESIAN_POINT('Ctrl Pts',(0.00628630384487386,-0.0385488798956495,
-0.0134403541329339));
#25828=CARTESIAN_POINT('Ctrl Pts',(0.00657323720202342,-0.0385669365839914,
-0.0133388637369163));
#25829=CARTESIAN_POINT('Ctrl Pts',(0.0067960455807007,-0.0385849932723333,
-0.0131583356952794));
#25830=CARTESIAN_POINT('Ctrl Pts',(0.00683027419908225,-0.0385877672052444,
-0.0131306023331813));
#25831=CARTESIAN_POINT('Ctrl Pts',(0.00686302916172385,-0.0385905411381556,
-0.0131010968226352));
#25832=CARTESIAN_POINT('Ctrl Pts',(0.00689413146807798,-0.0385933150710667,
-0.0130699948680723));
#25833=CARTESIAN_POINT('Ctrl Pts',(0.00709655136093038,-0.038611368368988,
-0.0128675772647462));
#25834=CARTESIAN_POINT('Ctrl Pts',(0.00722766676949683,-0.0386294216669094,
-0.0125929766257428));
#25835=CARTESIAN_POINT('Ctrl Pts',(0.00725759263530149,-0.0386474749648307,
-0.0123078419740864));
#25836=CARTESIAN_POINT('Ctrl Pts',(0.00726219643709343,-0.0386502522881624,
-0.0122639767964235));
#25837=CARTESIAN_POINT('Ctrl Pts',(0.00726449963204807,-0.0386530296114941,
-0.0122199001673678));
#25838=CARTESIAN_POINT('Ctrl Pts',(0.00726449999995587,-0.0386558069348258,
-0.0121758638510069));
#25839=CARTESIAN_POINT('Ctrl Pts',(0.00726450239144878,-0.0386738602327476,
-0.0118896167549034));
#25840=CARTESIAN_POINT('Ctrl Pts',(0.00716305422865381,-0.0386919135306694,
-0.0116027309013437));
#25841=CARTESIAN_POINT('Ctrl Pts',(0.00698258861408054,-0.0387099668285911,
-0.0113799388027853));
#25842=CARTESIAN_POINT('Ctrl Pts',(0.0069548257441594,-0.0387127441519224,
-0.011345664417239));
#25843=CARTESIAN_POINT('Ctrl Pts',(0.0069252862090245,-0.0387155214752537,
-0.0113128671345093));
#25844=CARTESIAN_POINT('Ctrl Pts',(0.00689414640842451,-0.038718298798585,
-0.0112817266454711));
#25845=CARTESIAN_POINT('Ctrl Pts',(0.00669169188390851,-0.0387363554869269,
-0.0110792676450937));
#25846=CARTESIAN_POINT('Ctrl Pts',(0.00641703196999779,-0.0387544121752688,
-0.0109481421930123));
#25847=CARTESIAN_POINT('Ctrl Pts',(0.00613183714804358,-0.0387724688636107,
-0.0109182447558953));
#25848=CARTESIAN_POINT('Ctrl Pts',(0.00608802450157561,-0.0387752427965218,
-0.0109136518048953));
#25849=CARTESIAN_POINT('Ctrl Pts',(0.00604400098357289,-0.038778016729433,
-0.0109113538915882));
#25850=CARTESIAN_POINT('Ctrl Pts',(0.00600001739078789,-0.0387807906623441,
-0.0109113532866777));
#25851=CARTESIAN_POINT('Ctrl Pts',(0.00571476495539528,-0.0387987808052228,
-0.010911349363574));
#25852=CARTESIAN_POINT('Ctrl Pts',(0.00542878155389685,-0.0388167709481014,
-0.0110121243151745));
#25853=CARTESIAN_POINT('Ctrl Pts',(0.0052063944651628,-0.0388347610909801,
-0.0111913988665488));
#25854=CARTESIAN_POINT('Ctrl Pts',(0.00517128158581817,-0.0388376015693545,
-0.0112197046721053));
#25855=CARTESIAN_POINT('Ctrl Pts',(0.00513771214689819,-0.0388404420477288,
-0.0112498691377489));
#25856=CARTESIAN_POINT('Ctrl Pts',(0.00510587818592995,-0.0388432825261032,
-0.0112817020512494));
#25857=CARTESIAN_POINT('Ctrl Pts',(0.00490047306974454,-0.0388616103990027,
-0.011487100408765));
#25858=CARTESIAN_POINT('Ctrl Pts',(0.00476860361596144,-0.0388799382719021,
-0.0117665222560225));
#25859=CARTESIAN_POINT('Ctrl Pts',(0.00474113115607628,-0.0388982661448016,
-0.0120566497471888));
#25860=CARTESIAN_POINT('Ctrl Pts',(0.00473737967579684,-0.0389007688931551,
-0.0120962678799));
#25861=CARTESIAN_POINT('Ctrl Pts',(0.00473550076196831,-0.0389032716415087,
-0.0121360549173962));
#25862=CARTESIAN_POINT('Ctrl Pts',(0.0047355000002319,-0.0389057743898623,
-0.0121758290694312));
#25863=CARTESIAN_POINT('Origin',(0.006,-0.0412787743898723,-0.0121758532865581));
#25864=CARTESIAN_POINT('',(0.0047355001992714,-0.0394057384386304,-0.0121763324065659));
#25865=CARTESIAN_POINT('',(0.0047355,-0.0393437675787716,-0.0121758532867651));
#25866=CARTESIAN_POINT('',(0.0047355,-0.0412787743898723,-0.0121758532865581));
#25867=CARTESIAN_POINT('Ctrl Pts',(0.0047355,-0.0393437675787716,-0.0121758532869721));
#25868=CARTESIAN_POINT('Ctrl Pts',(0.00473549999996698,-0.0393368792520501,
-0.0120750100100196));
#25869=CARTESIAN_POINT('Ctrl Pts',(0.00474756385553538,-0.0393299061355532,
-0.0119745079232119));
#25870=CARTESIAN_POINT('Ctrl Pts',(0.00477755184814463,-0.0393215869486887,
-0.0118514365807625));
#25871=CARTESIAN_POINT('Ctrl Pts',(0.00478442452436168,-0.0393199148525418,
-0.0118265652977435));
#25872=CARTESIAN_POINT('Ctrl Pts',(0.00479669080145859,-0.0393172643588143,
-0.0117869405525387));
#25873=CARTESIAN_POINT('Ctrl Pts',(0.00480160630587968,-0.039316271275942,
-0.0117720479732546));
#25874=CARTESIAN_POINT('Ctrl Pts',(0.00481169360095976,-0.0393143587739872,
-0.0117432947660889));
#25875=CARTESIAN_POINT('Ctrl Pts',(0.004816834068814,-0.039313438528612,
-0.0117294259356251));
#25876=CARTESIAN_POINT('Ctrl Pts',(0.0048297763937074,-0.0393112442771047,
-0.011696303067854));
#25877=CARTESIAN_POINT('Ctrl Pts',(0.00483781180765669,-0.03930997809057,
-0.0116771445738722));
#25878=CARTESIAN_POINT('Ctrl Pts',(0.00487816114598391,-0.0393040353783285,
-0.0115872201779668));
#25879=CARTESIAN_POINT('Ctrl Pts',(0.00491648806626039,-0.0392995633061622,
-0.0115193360685833));
#25880=CARTESIAN_POINT('Ctrl Pts',(0.005002685429934,-0.0392908883637259,
-0.0113950046379901));
#25881=CARTESIAN_POINT('Ctrl Pts',(0.00504973713903184,-0.0392866964812674,
-0.01133838144694));
#25882=CARTESIAN_POINT('Ctrl Pts',(0.00511182488931374,-0.0392813460311627,
-0.0112756736266181));
#25883=CARTESIAN_POINT('Ctrl Pts',(0.00512240052643995,-0.0392804399826695,
-0.011265360250361));
#25884=CARTESIAN_POINT('Ctrl Pts',(0.00513955983757548,-0.0392789734717999,
-0.0112492031928951));
#25885=CARTESIAN_POINT('Ctrl Pts',(0.00514602839708126,-0.039278421422328,
-0.0112432385959332));
#25886=CARTESIAN_POINT('Ctrl Pts',(0.00515915984202016,-0.0392773010273396,
-0.0112313813770644));
#25887=CARTESIAN_POINT('Ctrl Pts',(0.00516582368660932,-0.0392767326225019,
-0.0112254906051568));
#25888=CARTESIAN_POINT('Ctrl Pts',(0.00518407325136593,-0.0392751777541251,
-0.0112096979887208));
#25889=CARTESIAN_POINT('Ctrl Pts',(0.00519577640481568,-0.0392741825385337,
-0.0111999348061444));
#25890=CARTESIAN_POINT('Ctrl Pts',(0.00524763988364612,-0.0392697906078088,
-0.0111582348957848));
#25891=CARTESIAN_POINT('Ctrl Pts',(0.00528954407807787,-0.0392662911493851,
-0.0111285498456279));
#25892=CARTESIAN_POINT('Ctrl Pts',(0.00541659758759926,-0.0392560383961803,
-0.0110496860891085));
#25893=CARTESIAN_POINT('Ctrl Pts',(0.00550583192612201,-0.0392493004493489,
-0.0110077715321705));
#25894=CARTESIAN_POINT('Ctrl Pts',(0.00561909156203013,-0.0392415326914313,
-0.0109699028372782));
#25895=CARTESIAN_POINT('Ctrl Pts',(0.00563931952154971,-0.0392401722724608,
-0.0109636992524275));
#25896=CARTESIAN_POINT('Ctrl Pts',(0.00567385475363577,-0.0392378934814224,
-0.0109540490084974));
#25897=CARTESIAN_POINT('Ctrl Pts',(0.00568808326808116,-0.0392369670037755,
-0.0109503393548326));
#25898=CARTESIAN_POINT('Ctrl Pts',(0.00571746463897593,-0.0392350780360863,
-0.0109432239377833));
#25899=CARTESIAN_POINT('Ctrl Pts',(0.00573262205985419,-0.0392341166031605,
-0.0109398474566256));
#25900=CARTESIAN_POINT('Ctrl Pts',(0.00577230440056622,-0.039231630955099,
-0.0109317719624973));
#25901=CARTESIAN_POINT('Ctrl Pts',(0.0057969136166969,-0.0392301205700967,
-0.0109275185278807));
#25902=CARTESIAN_POINT('Ctrl Pts',(0.00592192278943934,-0.039222576195595,
-0.0109097070701317));
#25903=CARTESIAN_POINT('Ctrl Pts',(0.00602356127081529,-0.0392168917562445,
-0.0109075207281582));
#25904=CARTESIAN_POINT('Ctrl Pts',(0.00616936153422826,-0.039208410553092,
-0.0109219311893075));
#25905=CARTESIAN_POINT('Ctrl Pts',(0.00621407476665838,-0.0392057579995878,
-0.0109287866592796));
#25906=CARTESIAN_POINT('Ctrl Pts',(0.00627080030939606,-0.0392022215200484,
-0.0109406245729384));
#25907=CARTESIAN_POINT('Ctrl Pts',(0.00628323962887484,-0.0392014352169469,
-0.0109434174600005));
#25908=CARTESIAN_POINT('Ctrl Pts',(0.00630374253640136,-0.0392001181318345,
-0.010948347575428));
#25909=CARTESIAN_POINT('Ctrl Pts',(0.00631183134614074,-0.0391995930131198,
-0.0109503774574023));
#25910=CARTESIAN_POINT('Ctrl Pts',(0.00632906257756724,-0.0391984616539607,
-0.0109548832734043));
#25911=CARTESIAN_POINT('Ctrl Pts',(0.00633819810882039,-0.0391978542911164,
-0.0109573821219044));
#25912=CARTESIAN_POINT('Ctrl Pts',(0.00636476977452516,-0.0391960673334699,
-0.0109649721236327));
#25913=CARTESIAN_POINT('Ctrl Pts',(0.00638212468408195,-0.0391948744523137,
-0.0109703364557284));
#25914=CARTESIAN_POINT('Ctrl Pts',(0.00647959719340917,-0.0391880504472392,
-0.011002780986944));
#25915=CARTESIAN_POINT('Ctrl Pts',(0.00655695261414959,-0.0391821717268837,
-0.0110374705535267));
#25916=CARTESIAN_POINT('Ctrl Pts',(0.0066839928791492,-0.0391721795097203,
-0.0111105106377234));
#25917=CARTESIAN_POINT('Ctrl Pts',(0.00673538331995836,-0.0391680233874533,
-0.011145312465849));
#25918=CARTESIAN_POINT('Ctrl Pts',(0.00679993633001906,-0.039162683153921,
-0.0111963260166604));
#25919=CARTESIAN_POINT('Ctrl Pts',(0.00681554870062379,-0.0391613807886448,
-0.0112092860631907));
#25920=CARTESIAN_POINT('Ctrl Pts',(0.00684193719639083,-0.0391591591292178,
-0.0112322863392827));
#25921=CARTESIAN_POINT('Ctrl Pts',(0.00685286188420044,-0.0391582330174713,
-0.011242149124597));
#25922=CARTESIAN_POINT('Ctrl Pts',(0.00687518836630212,-0.0391563257134717,
-0.0112630243160011));
#25923=CARTESIAN_POINT('Ctrl Pts',(0.00688656032466012,-0.0391553459312388,
-0.0112740649347519));
#25924=CARTESIAN_POINT('Ctrl Pts',(0.0069165233014155,-0.0391527388785663,
-0.0113042696800743));
#25925=CARTESIAN_POINT('Ctrl Pts',(0.00693472041425494,-0.0391511282289925,
-0.0113238140629616));
#25926=CARTESIAN_POINT('Ctrl Pts',(0.00701781098827082,-0.0391436066312714,
-0.011418925165053));
#25927=CARTESIAN_POINT('Ctrl Pts',(0.00707424304872707,-0.0391380205090514,
-0.0115014043557035));
#25928=CARTESIAN_POINT('Ctrl Pts',(0.0071406571208009,-0.0391297189542401,
-0.0116283422162969));
#25929=CARTESIAN_POINT('Ctrl Pts',(0.00715888078049186,-0.0391271533430565,
-0.0116680524727002));
#25930=CARTESIAN_POINT('Ctrl Pts',(0.00717972704713311,-0.0391237103596348,
-0.0117204774694981));
#25931=CARTESIAN_POINT('Ctrl Pts',(0.00718426154651319,-0.0391229234566766,
-0.0117324036261477));
#25932=CARTESIAN_POINT('Ctrl Pts',(0.00719146070534891,-0.0391216056688344,
-0.0117522364625896));
#25933=CARTESIAN_POINT('Ctrl Pts',(0.00719422907732423,-0.039121080460829,
-0.0117601048845008));
#25934=CARTESIAN_POINT('Ctrl Pts',(0.00719997289811524,-0.0391199492872855,
-0.011776961173683));
#25935=CARTESIAN_POINT('Ctrl Pts',(0.00720292555158233,-0.0391193422055784,
-0.0117859558920852));
#25936=CARTESIAN_POINT('Ctrl Pts',(0.00721124122763924,-0.0391175569835497,
-0.0118122820161948));
#25937=CARTESIAN_POINT('Ctrl Pts',(0.00721633239518159,-0.0391163655937595,
-0.0118296960833896));
#25938=CARTESIAN_POINT('Ctrl Pts',(0.00724293803934281,-0.0391095658515815,
-0.0119285479314783));
#25939=CARTESIAN_POINT('Ctrl Pts',(0.00725664701194782,-0.039103711552185,
-0.0120118638110337));
#25940=CARTESIAN_POINT('Ctrl Pts',(0.00726591125311987,-0.0390937165145658,
-0.012158128254658));
#25941=CARTESIAN_POINT('Ctrl Pts',(0.00726524688766458,-0.039089535634441,
-0.012220547935026));
#25942=CARTESIAN_POINT('Ctrl Pts',(0.00725826586979714,-0.0390841716900076,
-0.0123028930883928));
#25943=CARTESIAN_POINT('Ctrl Pts',(0.00725606487391386,-0.0390828688201593,
-0.0123230715557001));
#25944=CARTESIAN_POINT('Ctrl Pts',(0.00725143136136867,-0.0390806465864308,
-0.0123577774646468));
#25945=CARTESIAN_POINT('Ctrl Pts',(0.00724922911943015,-0.0390797203952848,
-0.0123723310076697));
#25946=CARTESIAN_POINT('Ctrl Pts',(0.00724412936254339,-0.0390778131761194,
-0.0124024662760157));
#25947=CARTESIAN_POINT('Ctrl Pts',(0.00724119199942449,-0.0390768335537556,
-0.012418038696931));
#25948=CARTESIAN_POINT('Ctrl Pts',(0.00723252509507326,-0.039074227557888,
-0.0124596737084334));
#25949=CARTESIAN_POINT('Ctrl Pts',(0.00722626194009152,-0.0390726177801117,
-0.0124856176198209));
#25950=CARTESIAN_POINT('Ctrl Pts',(0.00719275483556149,-0.0390650961386547,
-0.0126073828479602));
#25951=CARTESIAN_POINT('Ctrl Pts',(0.00715507431207189,-0.0390595092931116,
-0.0126999575651164));
#25952=CARTESIAN_POINT('Ctrl Pts',(0.00708580441172114,-0.0390512063305857,
-0.0128253892625129));
#25953=CARTESIAN_POINT('Ctrl Pts',(0.00706272287071529,-0.0390486399708224,
-0.0128625028294435));
#25954=CARTESIAN_POINT('Ctrl Pts',(0.00703047977242015,-0.0390451961366919,
-0.0129088161085037));
#25955=CARTESIAN_POINT('Ctrl Pts',(0.00702303156639845,-0.0390444091890612,
-0.0129191765306699));
#25956=CARTESIAN_POINT('Ctrl Pts',(0.00701045724425558,-0.0390430913488836,
-0.0129361203353359));
#25957=CARTESIAN_POINT('Ctrl Pts',(0.00700542025544153,-0.0390425661342271,
-0.0129427691456154));
#25958=CARTESIAN_POINT('Ctrl Pts',(0.00699452692244313,-0.0390414349744801,
-0.0129568565314825));
#25959=CARTESIAN_POINT('Ctrl Pts',(0.0069886522989608,-0.0390408279136841,
-0.0129642798758794));
#25960=CARTESIAN_POINT('Ctrl Pts',(0.00697127893065427,-0.0390390428207079,
-0.0129857338701434));
#25961=CARTESIAN_POINT('Ctrl Pts',(0.0069595613533048,-0.0390378515417997,
-0.0129995833726727));
#25962=CARTESIAN_POINT('Ctrl Pts',(0.0068917922961739,-0.0390310535983054,
-0.0130762738437472));
#25963=CARTESIAN_POINT('Ctrl Pts',(0.00682987300420974,-0.039025201108867,
-0.0131336428391805));
#25964=CARTESIAN_POINT('Ctrl Pts',(0.00671297625450975,-0.0390152058599817,
-0.0132220433428793));
#25965=CARTESIAN_POINT('Ctrl Pts',(0.0066605195592206,-0.0390110231415432,
-0.0132559294451103));
#25966=CARTESIAN_POINT('Ctrl Pts',(0.0065879554257665,-0.0390056574379195,
-0.0132955320573579));
#25967=CARTESIAN_POINT('Ctrl Pts',(0.00656990867918295,-0.0390043545315766,
-0.0133048246350736));
#25968=CARTESIAN_POINT('Ctrl Pts',(0.0065384018589696,-0.0390021322563034,
-0.0133200998943206));
#25969=CARTESIAN_POINT('Ctrl Pts',(0.00652504701818892,-0.0390012060594077,
-0.0133262890817003));
#25970=CARTESIAN_POINT('Ctrl Pts',(0.00649709646367876,-0.0389992988463479,
-0.0133386543947277));
#25971=CARTESIAN_POINT('Ctrl Pts',(0.00648248653954957,-0.0389983192355242,
-0.0133447921580197));
#25972=CARTESIAN_POINT('Ctrl Pts',(0.00644297698056191,-0.038995713315959,
-0.0133605234847858));
#25973=CARTESIAN_POINT('Ctrl Pts',(0.00641788208130595,-0.0389941036011306,
-0.0133696065257176));
#25974=CARTESIAN_POINT('Ctrl Pts',(0.00629782994506804,-0.0389865819837905,
-0.0134088087890464));
#25975=CARTESIAN_POINT('Ctrl Pts',(0.00619982514309347,-0.0389809951097283,
-0.0134284314121707));
#25976=CARTESIAN_POINT('Ctrl Pts',(0.00605698897966107,-0.0389726920510793,
-0.0134398234525344));
#25977=CARTESIAN_POINT('Ctrl Pts',(0.00601329892582182,-0.038970125614426,
-0.0134410373652243));
#25978=CARTESIAN_POINT('Ctrl Pts',(0.0059568820447084,-0.0389666816929195,
-0.0134396823508011));
#25979=CARTESIAN_POINT('Ctrl Pts',(0.00594413188113673,-0.0389658947407048,
-0.0134391829293478));
#25980=CARTESIAN_POINT('Ctrl Pts',(0.00592306296437831,-0.0389645768951545,
-0.0134380381068915));
#25981=CARTESIAN_POINT('Ctrl Pts',(0.00591473878583227,-0.0389640516798132,
-0.0134375031391276));
#25982=CARTESIAN_POINT('Ctrl Pts',(0.00589697979758102,-0.0389629205214791,
-0.0134361852687505));
#25983=CARTESIAN_POINT('Ctrl Pts',(0.0058875476123952,-0.0389623134628286,
-0.0134353787189763));
#25984=CARTESIAN_POINT('Ctrl Pts',(0.00586007003285857,-0.0389605283830802,
-0.0134327180044229));
#25985=CARTESIAN_POINT('Ctrl Pts',(0.00584205506212158,-0.0389593371155352,
-0.0134305813989566));
#25986=CARTESIAN_POINT('Ctrl Pts',(0.00574070996510327,-0.0389525393563457,
-0.0134163446907461));
#25987=CARTESIAN_POINT('Ctrl Pts',(0.00565870828341002,-0.0389466870523613,
-0.0133963325207105));
#25988=CARTESIAN_POINT('Ctrl Pts',(0.0055204981265756,-0.0389366917816797,
-0.0133475729906142));
#25989=CARTESIAN_POINT('Ctrl Pts',(0.00546329891601119,-0.03893250887473,
-0.0133225018295304));
#25990=CARTESIAN_POINT('Ctrl Pts',(0.00539024210262064,-0.0389271429907183,
-0.0132838097122881));
#25991=CARTESIAN_POINT('Ctrl Pts',(0.00537253770468859,-0.0389258400806388,
-0.0132738802801265));
#25992=CARTESIAN_POINT('Ctrl Pts',(0.00534241952148878,-0.038923617801115,
-0.0132560221509658));
#25993=CARTESIAN_POINT('Ctrl Pts',(0.00532989150757916,-0.0389226916036335,
-0.0132482951258556));
#25994=CARTESIAN_POINT('Ctrl Pts',(0.00530416206566204,-0.0389207843912085,
-0.0132317987775011));
#25995=CARTESIAN_POINT('Ctrl Pts',(0.00529098480118406,-0.0389198047815729,
-0.0132229964445133));
#25996=CARTESIAN_POINT('Ctrl Pts',(0.00525607287374027,-0.0389171988698475,
-0.0131987142295685));
#25997=CARTESIAN_POINT('Ctrl Pts',(0.00523465638688125,-0.0389155891614845,
-0.0131827899170279));
#25998=CARTESIAN_POINT('Ctrl Pts',(0.00513574665300983,-0.0389080675468332,
-0.0131042648912665));
#25999=CARTESIAN_POINT('Ctrl Pts',(0.00506532873808064,-0.0389024806700257,
-0.0130333331341246));
#26000=CARTESIAN_POINT('Ctrl Pts',(0.00497705226703553,-0.0388941776015515,
-0.0129204647775152));
#26001=CARTESIAN_POINT('Ctrl Pts',(0.00495194474516104,-0.0388916111568294,
-0.0128846888173399));
#26002=CARTESIAN_POINT('Ctrl Pts',(0.00492196140382903,-0.0388881672261529,
-0.0128368796453873));
#26003=CARTESIAN_POINT('Ctrl Pts',(0.00491534636472717,-0.0388873802734561,
-0.0128259682954244));
#26004=CARTESIAN_POINT('Ctrl Pts',(0.00490468196062504,-0.038886062427337,
-0.0128077616824293));
#26005=CARTESIAN_POINT('Ctrl Pts',(0.00490053748232425,-0.0388855372119199,
-0.0128005227970824));
#26006=CARTESIAN_POINT('Ctrl Pts',(0.00489184284321092,-0.0388844060537095,
-0.0127849818306632));
#26007=CARTESIAN_POINT('Ctrl Pts',(0.00488731385568098,-0.0388837989952631,
-0.0127766688976815));
#26008=CARTESIAN_POINT('Ctrl Pts',(0.00487437964994546,-0.0388820139168246,
-0.012752280334548));
#26009=CARTESIAN_POINT('Ctrl Pts',(0.0048662268156162,-0.038880822650414,
-0.0127360743190182));
#26010=CARTESIAN_POINT('Ctrl Pts',(0.00482221165324144,-0.0388740249096991,
-0.0126436831839392));
#26011=CARTESIAN_POINT('Ctrl Pts',(0.00479368198600604,-0.0388681726243199,
-0.0125642427849889));
#26012=CARTESIAN_POINT('Ctrl Pts',(0.0047581339497195,-0.0388581773517096,
-0.0124220602282504));
#26013=CARTESIAN_POINT('Ctrl Pts',(0.00474750267794351,-0.038853994426094,
-0.0123605190018496));
#26014=CARTESIAN_POINT('Ctrl Pts',(0.00473948838005238,-0.0388486285242107,
-0.0122782378114584));
#26015=CARTESIAN_POINT('Ctrl Pts',(0.00473800742720685,-0.0388473256137542,
-0.0122579931495147));
#26016=CARTESIAN_POINT('Ctrl Pts',(0.00473629429393456,-0.0388451033337848,
-0.0122230205404961));
#26017=CARTESIAN_POINT('Ctrl Pts',(0.00473583088644126,-0.0388441771362282,
-0.0122083085272168));
#26018=CARTESIAN_POINT('Ctrl Pts',(0.00473554147278037,-0.0388428896926793,
-0.0121876789223812));
#26019=CARTESIAN_POINT('Ctrl Pts',(0.00473550000000128,-0.0388425219863233,
-0.0121817661174845));
#26020=CARTESIAN_POINT('Ctrl Pts',(0.0047355,-0.0388421555262979,-0.0121758532868327));
#26021=CARTESIAN_POINT('Ctrl Pts',(0.00473550000000009,-0.0389057758757622,
-0.012175852808333));
#26022=CARTESIAN_POINT('Ctrl Pts',(0.0047354998898438,-0.038924103588367,
-0.0124671228095654));
#26023=CARTESIAN_POINT('Ctrl Pts',(0.00484035214344072,-0.0389424313009718,
-0.012757881776193));
#26024=CARTESIAN_POINT('Ctrl Pts',(0.00502574963092566,-0.0389607590135766,
-0.0129819528265397));
#26025=CARTESIAN_POINT('Ctrl Pts',(0.00505106714236682,-0.0389632618094875,
-0.0130125515226587));
#26026=CARTESIAN_POINT('Ctrl Pts',(0.00507781374867609,-0.0389657646053984,
-0.01304194005383));
#26027=CARTESIAN_POINT('Ctrl Pts',(0.00510586298069669,-0.0389682674013093,
-0.0130699893168753));
#26028=CARTESIAN_POINT('Ctrl Pts',(0.00530747958806939,-0.0389862573847828,
-0.0132716061472521));
#26029=CARTESIAN_POINT('Ctrl Pts',(0.00558090980094445,-0.0390042473682563,
-0.0134026255654758));
#26030=CARTESIAN_POINT('Ctrl Pts',(0.00586501572457188,-0.0390222373517298,
-0.013433127916616));
#26031=CARTESIAN_POINT('Ctrl Pts',(0.00590987457571402,-0.039025077876772,
-0.0134379440795872));
#26032=CARTESIAN_POINT('Ctrl Pts',(0.00595495921214838,-0.0390279184018141,
-0.0134403532537739));
#26033=CARTESIAN_POINT('Ctrl Pts',(0.00599999907958751,-0.0390307589268563,
-0.0134403532865578));
#26034=CARTESIAN_POINT('Ctrl Pts',(0.0062863065904634,-0.0390488154554528,
-0.0134403534949571));
#26035=CARTESIAN_POINT('Ctrl Pts',(0.00657323966808948,-0.0390668719840494,
-0.013338862507273));
#26036=CARTESIAN_POINT('Ctrl Pts',(0.00679604762633477,-0.0390849285126459,
-0.0131583340378234));
#26037=CARTESIAN_POINT('Ctrl Pts',(0.00683027706300004,-0.039087702492565,
-0.0131305998946627));
#26038=CARTESIAN_POINT('Ctrl Pts',(0.00686303276466382,-0.0390904764724841,
-0.013101093515359));
#26039=CARTESIAN_POINT('Ctrl Pts',(0.00689413571764325,-0.0390932504524032,
-0.0130699906185349));
#26040=CARTESIAN_POINT('Ctrl Pts',(0.00709655459888521,-0.0391113035907076,
-0.0128675721027531));
#26041=CARTESIAN_POINT('Ctrl Pts',(0.00722766869842946,-0.0391293567290121,
-0.0125929709100995));
#26042=CARTESIAN_POINT('Ctrl Pts',(0.00725759324381091,-0.0391474098673166,
-0.0123078361760596));
#26043=CARTESIAN_POINT('Ctrl Pts',(0.00726219696087802,-0.0391501872375278,
-0.0122639698574641));
#26044=CARTESIAN_POINT('Ctrl Pts',(0.00726449995254541,-0.039152964607739,
-0.0122198920873515));
#26045=CARTESIAN_POINT('Ctrl Pts',(0.00726449999999927,-0.0391557419779502,
-0.012175854649158));
#26046=CARTESIAN_POINT('Ctrl Pts',(0.00726450030845333,-0.0391737951162547,
-0.011889607623441));
#26047=CARTESIAN_POINT('Ctrl Pts',(0.00716305010451997,-0.0391918482545591,
-0.0116027225601036));
#26048=CARTESIAN_POINT('Ctrl Pts',(0.00698258293554201,-0.0392099013928636,
-0.011379931792451));
#26049=CARTESIAN_POINT('Ctrl Pts',(0.00695481911238977,-0.0392126787630748,
-0.0113456567300777));
#26050=CARTESIAN_POINT('Ctrl Pts',(0.00692527854380358,-0.039215456133286,
-0.0113128588587458));
#26051=CARTESIAN_POINT('Ctrl Pts',(0.00689413764465013,-0.0392182335034972,
-0.0112817178815888));
#26052=CARTESIAN_POINT('Ctrl Pts',(0.00669168118644839,-0.0392362900320937,
-0.0110792609162627));
#26053=CARTESIAN_POINT('Ctrl Pts',(0.00641702005861165,-0.0392543465606902,
-0.0109481381604391));
#26054=CARTESIAN_POINT('Ctrl Pts',(0.00613182500527585,-0.0392724030892866,
-0.0109182434830085));
#26055=CARTESIAN_POINT('Ctrl Pts',(0.00608801119318087,-0.0392751770692058,
-0.0109136508375041));
#26056=CARTESIAN_POINT('Ctrl Pts',(0.00604398652098787,-0.039277951049125,
-0.0109113533493376));
#26057=CARTESIAN_POINT('Ctrl Pts',(0.00600000180478717,-0.0392807250290442,
-0.0109113532865594));
#26058=CARTESIAN_POINT('Ctrl Pts',(0.0057147494451515,-0.0392987150125177,
-0.0109113528794263));
#26059=CARTESIAN_POINT('Ctrl Pts',(0.00542876734207387,-0.0393167049959913,
-0.0110121313060387));
#26060=CARTESIAN_POINT('Ctrl Pts',(0.0052063824825844,-0.0393346949794648,
-0.0111914085262739));
#26061=CARTESIAN_POINT('Ctrl Pts',(0.00517126906720493,-0.039337535504507,
-0.0112197154690965));
#26062=CARTESIAN_POINT('Ctrl Pts',(0.00513769919244742,-0.0393403760295491,
-0.0112498811464967));
#26063=CARTESIAN_POINT('Ctrl Pts',(0.00510586490770486,-0.0393432165545913,
-0.0112817153292348));
#26064=CARTESIAN_POINT('Ctrl Pts',(0.00490046287355843,-0.0393615442671949,
-0.0114871167052248));
#26065=CARTESIAN_POINT('Ctrl Pts',(0.00476859756919286,-0.0393798719797985,
-0.0117665404683745));
#26066=CARTESIAN_POINT('Ctrl Pts',(0.00474112939608375,-0.039398199692402,
-0.0120566683353456));
#26067=CARTESIAN_POINT('Ctrl Pts',(0.00473737839709893,-0.0394007024883141,
-0.0120962876187305));
#26068=CARTESIAN_POINT('Ctrl Pts',(0.0047355000706813,-0.0394032052842262,
-0.0121360757886226));
#26069=CARTESIAN_POINT('Ctrl Pts',(0.004735500000002,-0.0394057080801383,
-0.0121758510395836));
#26070=CARTESIAN_POINT('Origin',(0.006,-0.0412787743898723,-0.0121758532865581));
#26071=CARTESIAN_POINT('',(0.00473550016783225,-0.0399058036708604,-0.0121753956645968));
#26072=CARTESIAN_POINT('',(0.0047355,-0.0398434635507866,-0.0121758533388321));
#26073=CARTESIAN_POINT('',(0.0047355,-0.0412787743898723,-0.0121758532865581));
#26074=CARTESIAN_POINT('Ctrl Pts',(0.0047355,-0.0398434635507866,-0.0121758533911061));
#26075=CARTESIAN_POINT('Ctrl Pts',(0.00473549999871623,-0.0398425730336631,
-0.0121603262647505));
#26076=CARTESIAN_POINT('Ctrl Pts',(0.00473578598915216,-0.0398416814807293,
-0.012144793103517));
#26077=CARTESIAN_POINT('Ctrl Pts',(0.00473771522235276,-0.0398386660407253,
-0.0120924690080894));
#26078=CARTESIAN_POINT('Ctrl Pts',(0.00474067799968203,-0.0398365301708808,
-0.0120557550046254));
#26079=CARTESIAN_POINT('Ctrl Pts',(0.00474728561309504,-0.039833359682442,
-0.0120028209337214));
#26080=CARTESIAN_POINT('Ctrl Pts',(0.00474965465898228,-0.0398323669216644,
-0.0119864594887893));
#26081=CARTESIAN_POINT('Ctrl Pts',(0.00475452352385184,-0.0398305444041562,
-0.0119569282734438));
#26082=CARTESIAN_POINT('Ctrl Pts',(0.00475691333422698,-0.0398297194916137,
-0.0119437427036166));
#26083=CARTESIAN_POINT('Ctrl Pts',(0.00476116729457608,-0.0398283514289037,
-0.0119222263852539));
#26084=CARTESIAN_POINT('Ctrl Pts',(0.00476290714918767,-0.0398278147399946,
-0.0119138717000038));
#26085=CARTESIAN_POINT('Ctrl Pts',(0.00476671193992603,-0.0398266853100518,
-0.0118964849961814));
#26086=CARTESIAN_POINT('Ctrl Pts',(0.00476879178473736,-0.0398260918779022,
-0.0118874570328898));
#26087=CARTESIAN_POINT('Ctrl Pts',(0.00477499028516025,-0.0398243897368797,
-0.0118618412498231));
#26088=CARTESIAN_POINT('Ctrl Pts',(0.00477934617361855,-0.0398232694909095,
-0.0118453135270823));
#26089=CARTESIAN_POINT('Ctrl Pts',(0.00480578068815565,-0.0398168843935129,
-0.0117526739949715));
#26090=CARTESIAN_POINT('Ctrl Pts',(0.00483464047371733,-0.0398113905697856,
-0.0116786846484056));
#26091=CARTESIAN_POINT('Ctrl Pts',(0.00489875860328867,-0.0398016296401179,
-0.0115511445764787));
#26092=CARTESIAN_POINT('Ctrl Pts',(0.00493152138538451,-0.0397973468153562,
-0.0114966266299599));
#26093=CARTESIAN_POINT('Ctrl Pts',(0.00498141345853777,-0.0397917130586943,
-0.0114262131066627));
#26094=CARTESIAN_POINT('Ctrl Pts',(0.00499508073012373,-0.03979024395799,
-0.0114079885137661));
#26095=CARTESIAN_POINT('Ctrl Pts',(0.00501863257896625,-0.0397878299586647,
-0.0113782900942377));
#26096=CARTESIAN_POINT('Ctrl Pts',(0.0050282438112329,-0.0397868749026981,
-0.0113666073400606));
#26097=CARTESIAN_POINT('Ctrl Pts',(0.00504792040127838,-0.0397849774233039,
-0.0113435460458716));
#26098=CARTESIAN_POINT('Ctrl Pts',(0.0050579857586511,-0.0397840352233526,
-0.0113321708195238));
#26099=CARTESIAN_POINT('Ctrl Pts',(0.00508388079154384,-0.0397816792831149,
-0.0113039472512419));
#26100=CARTESIAN_POINT('Ctrl Pts',(0.00509997236014619,-0.0397802765930414,
-0.011287346176422));
#26101=CARTESIAN_POINT('Ctrl Pts',(0.00516472607808981,-0.0397748485377832,
-0.0112241077160463));
#26102=CARTESIAN_POINT('Ctrl Pts',(0.00521663022018865,-0.0397709616916161,
-0.0111809487226794));
#26103=CARTESIAN_POINT('Ctrl Pts',(0.0053175467035916,-0.039763879742537,
-0.0111098520483408));
#26104=CARTESIAN_POINT('Ctrl Pts',(0.00536545503199703,-0.0397606840681993,
-0.0110806577759889));
#26105=CARTESIAN_POINT('Ctrl Pts',(0.00543353668269892,-0.0397561672907358,
-0.0110451410517151));
#26106=CARTESIAN_POINT('Ctrl Pts',(0.0054521671259105,-0.0397549333418394,
-0.0110359980736416));
#26107=CARTESIAN_POINT('Ctrl Pts',(0.00548539780306348,-0.0397527217937917,
-0.0110206928469228));
#26108=CARTESIAN_POINT('Ctrl Pts',(0.00549990494336334,-0.0397517528569151,
-0.0110143387814702));
#26109=CARTESIAN_POINT('Ctrl Pts',(0.00552285116151035,-0.039750209131006,
-0.0110047979888791));
#26110=CARTESIAN_POINT('Ctrl Pts',(0.00553121198453355,-0.0397496443658862,
-0.0110014260604236));
#26111=CARTESIAN_POINT('Ctrl Pts',(0.00554770725849822,-0.0397485243246831,
-0.0109949776997911));
#26112=CARTESIAN_POINT('Ctrl Pts',(0.00555583872891021,-0.0397479694011279,
-0.0109918952523875));
#26113=CARTESIAN_POINT('Ctrl Pts',(0.00557738388106423,-0.0397464929144523,
-0.010983981173393));
#26114=CARTESIAN_POINT('Ctrl Pts',(0.00559084833603183,-0.0397455639606821,
-0.010979292216427));
#26115=CARTESIAN_POINT('Ctrl Pts',(0.0056791097279547,-0.0397394467852465,
-0.0109502192724743));
#26116=CARTESIAN_POINT('Ctrl Pts',(0.00575595980303853,-0.0397340033639544,
-0.0109326347950351));
#26117=CARTESIAN_POINT('Ctrl Pts',(0.00590706589949332,-0.0397235632552518,
-0.0109126174506006));
#26118=CARTESIAN_POINT('Ctrl Pts',(0.00598090852293102,-0.0397185800004054,
-0.0109093463135961));
#26119=CARTESIAN_POINT('Ctrl Pts',(0.00607529272130587,-0.0397124420449962,
-0.0109134273496162));
#26120=CARTESIAN_POINT('Ctrl Pts',(0.00609593718780759,-0.0397111128179512,
-0.0109148281573623));
#26121=CARTESIAN_POINT('Ctrl Pts',(0.00613125247819444,-0.0397088604923665,
-0.010918096800554));
#26122=CARTESIAN_POINT('Ctrl Pts',(0.00614594142667959,-0.0397079300581504,
-0.0109197164626415));
#26123=CARTESIAN_POINT('Ctrl Pts',(0.00617617991867307,-0.0397060266754757,
-0.0109235882876082));
#26124=CARTESIAN_POINT('Ctrl Pts',(0.0061917226936039,-0.0397050549130296,
-0.0109258735131326));
#26125=CARTESIAN_POINT('Ctrl Pts',(0.00623281055152999,-0.0397025008524645,
-0.0109326990416615));
#26126=CARTESIAN_POINT('Ctrl Pts',(0.0062582659688675,-0.039700933933303,
-0.0109377369535174));
#26127=CARTESIAN_POINT('Ctrl Pts',(0.00638613651834869,-0.0396931087662235,
-0.010967159741422));
#26128=CARTESIAN_POINT('Ctrl Pts',(0.00648536860536396,-0.0396872264942755,
-0.0110034802865309));
#26129=CARTESIAN_POINT('Ctrl Pts',(0.00660349958051729,-0.039679502627529,
-0.0110643179275181));
#26130=CARTESIAN_POINT('Ctrl Pts',(0.00662762434558757,-0.0396778809542012,
-0.0110777594306216));
#26131=CARTESIAN_POINT('Ctrl Pts',(0.00666790371812734,-0.039675065084725,
-0.0111019628738786));
#26132=CARTESIAN_POINT('Ctrl Pts',(0.00668428623571204,-0.0396738878024674,
-0.0111123269564249));
#26133=CARTESIAN_POINT('Ctrl Pts',(0.0067084974580347,-0.0396720892137892,
-0.011128434719574));
#26134=CARTESIAN_POINT('Ctrl Pts',(0.00671650946002454,-0.0396714840729467,
-0.0111338991213237));
#26135=CARTESIAN_POINT('Ctrl Pts',(0.00673130877071756,-0.039670346048942,
-0.0111442440547512));
#26136=CARTESIAN_POINT('Ctrl Pts',(0.00673811183493579,-0.0396698146358723,
-0.011149100624618));
#26137=CARTESIAN_POINT('Ctrl Pts',(0.00675482836888941,-0.0396684888371073,
-0.0111612862015588));
#26138=CARTESIAN_POINT('Ctrl Pts',(0.00676468355633603,-0.0396676896058306,
-0.0111686932851221));
#26139=CARTESIAN_POINT('Ctrl Pts',(0.00680464683820562,-0.0396643808905084,
-0.0111996540506689));
#26140=CARTESIAN_POINT('Ctrl Pts',(0.00683378569181862,-0.0396618081250233,
-0.0112244215178391));
#26141=CARTESIAN_POINT('Ctrl Pts',(0.00692014223919626,-0.0396537749630439,
-0.0113048401799208));
#26142=CARTESIAN_POINT('Ctrl Pts',(0.00697325681895921,-0.039648246404119,
-0.0113646207921799));
#26143=CARTESIAN_POINT('Ctrl Pts',(0.00703821874619604,-0.0396408468536321,
-0.0114533756588055));
#26144=CARTESIAN_POINT('Ctrl Pts',(0.00705517603101273,-0.0396388386705201,
-0.0114783750817396));
#26145=CARTESIAN_POINT('Ctrl Pts',(0.00708425053212983,-0.0396352537588027,
-0.0115247295224242));
#26146=CARTESIAN_POINT('Ctrl Pts',(0.00709667192631941,-0.0396336676256535,
-0.011545875357773));
#26147=CARTESIAN_POINT('Ctrl Pts',(0.00711590296690817,-0.039631117287945,
-0.0115809084721999));
#26148=CARTESIAN_POINT('Ctrl Pts',(0.0071230862363398,-0.0396301403821461,
-0.011594582176817));
#26149=CARTESIAN_POINT('Ctrl Pts',(0.00713663772928902,-0.0396282471045765,
-0.0116215676697012));
#26150=CARTESIAN_POINT('Ctrl Pts',(0.00714302699238698,-0.0396273301303916,
-0.0116348660447212));
#26151=CARTESIAN_POINT('Ctrl Pts',(0.00715813635276517,-0.0396250978748872,
-0.0116677774909757));
#26152=CARTESIAN_POINT('Ctrl Pts',(0.00716659278890381,-0.0396237914863275,
-0.0116875069227721));
#26153=CARTESIAN_POINT('Ctrl Pts',(0.00721013120870794,-0.0396167166417189,
-0.0117966799196198));
#26154=CARTESIAN_POINT('Ctrl Pts',(0.0072354338234921,-0.0396112772785581,
-0.0118896807685754));
#26155=CARTESIAN_POINT('Ctrl Pts',(0.0072558130989148,-0.0396035244138168,
-0.0120229106952813));
#26156=CARTESIAN_POINT('Ctrl Pts',(0.00725990514803603,-0.0396012840645187,
-0.01206141263571));
#26157=CARTESIAN_POINT('Ctrl Pts',(0.00726324526001623,-0.039597977473665,
-0.0121170220094639));
#26158=CARTESIAN_POINT('Ctrl Pts',(0.00726392241684811,-0.0395969570287086,
-0.0121340229278381));
#26159=CARTESIAN_POINT('Ctrl Pts',(0.0072645250694901,-0.0395950893226703,
-0.0121647180974538));
#26160=CARTESIAN_POINT('Ctrl Pts',(0.00726457150264754,-0.0395942472916623,
-0.0121784074785993));
#26161=CARTESIAN_POINT('Ctrl Pts',(0.0072642854083989,-0.0395928586620499,
-0.0122006805328556));
#26162=CARTESIAN_POINT('Ctrl Pts',(0.00726408766330845,-0.0395923189253832,
-0.0122092652738219));
#26163=CARTESIAN_POINT('Ctrl Pts',(0.00726349787575642,-0.0395911924954774,
-0.0122270148535366));
#26164=CARTESIAN_POINT('Ctrl Pts',(0.00726309351885227,-0.0395906052602424,
-0.012236178559888));
#26165=CARTESIAN_POINT('Ctrl Pts',(0.00726167599879556,-0.0395889401289352,
-0.0122619364391194));
#26166=CARTESIAN_POINT('Ctrl Pts',(0.00726043524798963,-0.0395878514253083,
-0.0122785156510738));
#26167=CARTESIAN_POINT('Ctrl Pts',(0.00725134964668775,-0.0395814704873993,
-0.0123744593002325));
#26168=CARTESIAN_POINT('Ctrl Pts',(0.0072363376653185,-0.039575941740716,
-0.0124529604966164));
#26169=CARTESIAN_POINT('Ctrl Pts',(0.00719620774994823,-0.0395661299325991,
-0.0125907142888971));
#26170=CARTESIAN_POINT('Ctrl Pts',(0.00717377829703182,-0.0395618309659139,
-0.012650478373365));
#26171=CARTESIAN_POINT('Ctrl Pts',(0.00713733155497881,-0.0395561799438829,
-0.0127289873250513));
#26172=CARTESIAN_POINT('Ctrl Pts',(0.00712717055428588,-0.0395547087992434,
-0.0127494097170517));
#26173=CARTESIAN_POINT('Ctrl Pts',(0.00710935760137422,-0.0395522924220401,
-0.0127829075984756));
#26174=CARTESIAN_POINT('Ctrl Pts',(0.00710201354731257,-0.039551336989218,
-0.0127961398319851));
#26175=CARTESIAN_POINT('Ctrl Pts',(0.00708682902470908,-0.0395494394621625,
-0.0128223773809974));
#26176=CARTESIAN_POINT('Ctrl Pts',(0.00707898830310865,-0.0395484975792306,
-0.0128353796364852));
#26177=CARTESIAN_POINT('Ctrl Pts',(0.00705864079456163,-0.0395461438317747,
-0.0128677873537415));
#26178=CARTESIAN_POINT('Ctrl Pts',(0.00704583301386208,-0.0395447429720405,
-0.0128869977801207));
#26179=CARTESIAN_POINT('Ctrl Pts',(0.00698583206638948,-0.0395385094726972,
-0.0129718632616287));
#26180=CARTESIAN_POINT('Ctrl Pts',(0.00693293409140296,-0.0395338901262536,
-0.0130332517492821));
#26181=CARTESIAN_POINT('Ctrl Pts',(0.00682714716296224,-0.0395254893060913,
-0.0131345461167398));
#26182=CARTESIAN_POINT('Ctrl Pts',(0.00677630714365207,-0.0395217215608465,
-0.0131761581254128));
#26183=CARTESIAN_POINT('Ctrl Pts',(0.00671045394004568,-0.0395168546820953,
-0.0132220033762255));
#26184=CARTESIAN_POINT('Ctrl Pts',(0.00669828840301553,-0.039515955937636,
-0.0132301625750231));
#26185=CARTESIAN_POINT('Ctrl Pts',(0.00667861392344697,-0.0395144983718384,
-0.0132428679882191));
#26186=CARTESIAN_POINT('Ctrl Pts',(0.00667119423118024,-0.0395139477819667,
-0.0132475507839627));
#26187=CARTESIAN_POINT('Ctrl Pts',(0.00665613270458966,-0.0395128270377177,
-0.0132568388191417));
#26188=CARTESIAN_POINT('Ctrl Pts',(0.00664848970368741,-0.0395122567739995,
-0.0132614411184432));
#26189=CARTESIAN_POINT('Ctrl Pts',(0.00662754417199865,-0.0395106911447898,
-0.0132737535363856));
#26190=CARTESIAN_POINT('Ctrl Pts',(0.00661414908460164,-0.0395096868342676,
-0.013281302290321));
#26191=CARTESIAN_POINT('Ctrl Pts',(0.00655479806369439,-0.0395052342659157,
-0.0133133376927267));
#26192=CARTESIAN_POINT('Ctrl Pts',(0.00650749513530756,-0.0395016806859326,
-0.0133352149716183));
#26193=CARTESIAN_POINT('Ctrl Pts',(0.00639812382988118,-0.0394936316428007,
-0.0133778197987371));
#26194=CARTESIAN_POINT('Ctrl Pts',(0.0063355151022178,-0.0394891416010819,
-0.0133967778756529));
#26195=CARTESIAN_POINT('Ctrl Pts',(0.00623279140903417,-0.0394820943926213,
-0.0134193793675272));
#26196=CARTESIAN_POINT('Ctrl Pts',(0.00619347787933736,-0.0394794682015931,
-0.0134260995806315));
#26197=CARTESIAN_POINT('Ctrl Pts',(0.00613602802260432,-0.0394757355256694,
-0.0134331444884616));
#26198=CARTESIAN_POINT('Ctrl Pts',(0.00611810148456964,-0.0394745852880538,
-0.0134349549035853));
#26199=CARTESIAN_POINT('Ctrl Pts',(0.00608570790750952,-0.0394725316288873,
-0.0134375283839546));
#26200=CARTESIAN_POINT('Ctrl Pts',(0.00607125512256349,-0.039471624232183,
-0.0134384270989329));
#26201=CARTESIAN_POINT('Ctrl Pts',(0.00603970574223539,-0.0394696614215763,
-0.0134398454353331));
#26202=CARTESIAN_POINT('Ctrl Pts',(0.00602260747440094,-0.0394686091635386,
-0.0134402668435503));
#26203=CARTESIAN_POINT('Ctrl Pts',(0.00597167916045773,-0.0394655048936305,
-0.0134404885728341));
#26204=CARTESIAN_POINT('Ctrl Pts',(0.00593785901844548,-0.0394634831632167,
-0.013439278492207));
#26205=CARTESIAN_POINT('Ctrl Pts',(0.0058092500041775,-0.0394558856409178,
-0.0134294992381665));
#26206=CARTESIAN_POINT('Ctrl Pts',(0.00571549661962608,-0.039450558819576,
-0.013411600348725));
#26207=CARTESIAN_POINT('Ctrl Pts',(0.00559996511864355,-0.0394435080227075,
-0.0133756866073562));
#26208=CARTESIAN_POINT('Ctrl Pts',(0.00557553294453327,-0.0394419860402525,
-0.0133672623191858));
#26209=CARTESIAN_POINT('Ctrl Pts',(0.00553406780674108,-0.0394393232001577,
-0.0133515276482681));
#26210=CARTESIAN_POINT('Ctrl Pts',(0.00551690559551872,-0.0394381968929906,
-0.0133445802572899));
#26211=CARTESIAN_POINT('Ctrl Pts',(0.00549114348868031,-0.0394364604351813,
-0.0133334871916281));
#26212=CARTESIAN_POINT('Ctrl Pts',(0.00548242716578311,-0.0394358648299555,
-0.0133296165011747));
#26213=CARTESIAN_POINT('Ctrl Pts',(0.00546619414138775,-0.0394347388617283,
-0.0133221868815999));
#26214=CARTESIAN_POINT('Ctrl Pts',(0.00545866737347649,-0.039434209828916,
-0.0133186517717289));
#26215=CARTESIAN_POINT('Ctrl Pts',(0.00543983056793416,-0.0394328690056492,
-0.0133095768246517));
#26216=CARTESIAN_POINT('Ctrl Pts',(0.00542856759815566,-0.0394320519386242,
-0.0133039418625878));
#26217=CARTESIAN_POINT('Ctrl Pts',(0.00538083664955803,-0.0394285290246062,
-0.0132791634578248));
#26218=CARTESIAN_POINT('Ctrl Pts',(0.00534523407302543,-0.0394257497932153,
-0.0132584139485412));
#26219=CARTESIAN_POINT('Ctrl Pts',(0.00522751145313689,-0.0394161724752054,
-0.0131818702838085));
#26220=CARTESIAN_POINT('Ctrl Pts',(0.00515095620933812,-0.0394092972822839,
-0.0131181580656726));
#26221=CARTESIAN_POINT('Ctrl Pts',(0.0050630308980468,-0.0394008679125229,
-0.0130254771495794));
#26222=CARTESIAN_POINT('Ctrl Pts',(0.00504412706169264,-0.0393990143680964,
-0.013004152107354));
#26223=CARTESIAN_POINT('Ctrl Pts',(0.00501564290776988,-0.0393961533420522,
-0.0129697443686626));
#26224=CARTESIAN_POINT('Ctrl Pts',(0.00500556699254515,-0.0393951266523914,
-0.0129570862656416));
#26225=CARTESIAN_POINT('Ctrl Pts',(0.00498685784296865,-0.0393931905709259,
-0.0129326337710019));
#26226=CARTESIAN_POINT('Ctrl Pts',(0.00497818084244687,-0.0393922795941065,
-0.0129208763527132));
#26227=CARTESIAN_POINT('Ctrl Pts',(0.00495860067613465,-0.0393901914088626,
-0.0128933592580963));
#26228=CARTESIAN_POINT('Ctrl Pts',(0.00494784793025412,-0.0393890199001457,
-0.012877496680104));
#26229=CARTESIAN_POINT('Ctrl Pts',(0.00491170333890462,-0.0393849852979684,
-0.0128214751653821));
#26230=CARTESIAN_POINT('Ctrl Pts',(0.00488821600920942,-0.0393821884938485,
-0.0127801332073064));
#26231=CARTESIAN_POINT('Ctrl Pts',(0.00482209191386929,-0.0393735525985662,
-0.0126467703460761));
#26232=CARTESIAN_POINT('Ctrl Pts',(0.00478815756692421,-0.039367910615778,
-0.0125509052735547));
#26233=CARTESIAN_POINT('Ctrl Pts',(0.00476205822316223,-0.0393607301401242,
-0.0124342924930554));
#26234=CARTESIAN_POINT('Ctrl Pts',(0.00475847130345653,-0.0393596235685395,
-0.0124164714237126));
#26235=CARTESIAN_POINT('Ctrl Pts',(0.0047536012484247,-0.0393579112099727,
-0.0123892546764662));
#26236=CARTESIAN_POINT('Ctrl Pts',(0.00475203747938668,-0.0393573193617461,
-0.0123799109631057));
#26237=CARTESIAN_POINT('Ctrl Pts',(0.00474929492120454,-0.0393561956113855,
-0.01236231131214));
#26238=CARTESIAN_POINT('Ctrl Pts',(0.00474809257008097,-0.0393556649419783,
-0.0123540597978812));
#26239=CARTESIAN_POINT('Ctrl Pts',(0.0047452593922461,-0.0393543126707145,
-0.0123331702702483));
#26240=CARTESIAN_POINT('Ctrl Pts',(0.0047437378656051,-0.039353485598572,
-0.0123205185784411));
#26241=CARTESIAN_POINT('Ctrl Pts',(0.00473787898038878,-0.0393498070643418,
-0.0122646969183499));
#26242=CARTESIAN_POINT('Ctrl Pts',(0.00473557428322698,-0.0393468741467418,
-0.0122213462701389));
#26243=CARTESIAN_POINT('Ctrl Pts',(0.00473550058894212,-0.0393438638310085,
-0.0121772625009416));
#26244=CARTESIAN_POINT('Ctrl Pts',(0.00473550000000023,-0.039343815707962,
-0.0121765578855601));
#26245=CARTESIAN_POINT('Ctrl Pts',(0.0047355,-0.0393437675787716,-0.0121758532869721));
#26246=CARTESIAN_POINT('Ctrl Pts',(0.00473550043525086,-0.0394057743898623,
-0.0121769024525323));
#26247=CARTESIAN_POINT('Ctrl Pts',(0.00473574210657924,-0.0394241093002937,
-0.0124681750414799));
#26248=CARTESIAN_POINT('Ctrl Pts',(0.00484083747198399,-0.0394424442107252,
-0.0127588490205952));
#26249=CARTESIAN_POINT('Ctrl Pts',(0.00502642382811335,-0.0394607791211566,
-0.0129827669669072));
#26250=CARTESIAN_POINT('Ctrl Pts',(0.00505171291824375,-0.0394632775440585,
-0.013013279345318));
#26251=CARTESIAN_POINT('Ctrl Pts',(0.00507842401280127,-0.0394657759669604,
-0.0130425855306932));
#26252=CARTESIAN_POINT('Ctrl Pts',(0.00510643135848585,-0.0394682743898623,
-0.01307055733422));
#26253=CARTESIAN_POINT('Ctrl Pts',(0.0053081802385946,-0.0394862715977439,
-0.0132720501889767));
#26254=CARTESIAN_POINT('Ctrl Pts',(0.00558169950567516,-0.0395042688056254,
-0.0134028961466365));
#26255=CARTESIAN_POINT('Ctrl Pts',(0.00586582975456806,-0.0395222660135069,
-0.0134332150464509));
#26256=CARTESIAN_POINT('Ctrl Pts',(0.00591060497947018,-0.0395251021389587,
-0.013437992909995));
#26257=CARTESIAN_POINT('Ctrl Pts',(0.00595560356959221,-0.0395279382644105,
-0.0134403729491083));
#26258=CARTESIAN_POINT('Ctrl Pts',(0.00600055654076817,-0.0395307743898623,
-0.0134403531640837));
#26259=CARTESIAN_POINT('Ctrl Pts',(0.00628686958246528,-0.0395488381503545,
-0.0134402271499314));
#26260=CARTESIAN_POINT('Ctrl Pts',(0.00657376200210831,-0.0395669019108467,
-0.0133386059966377));
#26261=CARTESIAN_POINT('Ctrl Pts',(0.00679649174944665,-0.0395849656713389,
-0.0131579740240764));
#26262=CARTESIAN_POINT('Ctrl Pts',(0.00683064113154301,-0.03958773524418,
-0.0131302791592299));
#26263=CARTESIAN_POINT('Ctrl Pts',(0.00686332180109535,-0.0395905048170212,
-0.0131008197125847));
#26264=CARTESIAN_POINT('Ctrl Pts',(0.00689435586231493,-0.0395932743898623,
-0.0130697704200458));
#26265=CARTESIAN_POINT('Ctrl Pts',(0.00709672871535894,-0.0396113347511412,
-0.0128672982436964));
#26266=CARTESIAN_POINT('Ctrl Pts',(0.00722777549510725,-0.0396293951124201,
-0.0125926594158705));
#26267=CARTESIAN_POINT('Ctrl Pts',(0.00725762714925349,-0.039647455473699,
-0.0123075127087828));
#26268=CARTESIAN_POINT('Ctrl Pts',(0.00726221054608859,-0.0396502284457534,
-0.0122637315330931));
#26269=CARTESIAN_POINT('Ctrl Pts',(0.00726450221993153,-0.0396530014178079,
-0.0122197403218513));
#26270=CARTESIAN_POINT('Ctrl Pts',(0.00726449999838466,-0.0396557743898623,
-0.0121757893710805));
#26271=CARTESIAN_POINT('Ctrl Pts',(0.00726448552945449,-0.0396738347511412,
-0.0118895369192389));
#26272=CARTESIAN_POINT('Ctrl Pts',(0.0071630169273656,-0.0396918951124201,
-0.0116026530874273));
#26273=CARTESIAN_POINT('Ctrl Pts',(0.00698253310284427,-0.039709955473699,
-0.0113798702768053));
#26274=CARTESIAN_POINT('Ctrl Pts',(0.00695482177448543,-0.0397127284457534,
-0.0113456643991637));
#26275=CARTESIAN_POINT('Ctrl Pts',(0.00692534078294909,-0.0397155014178078,
-0.0113129300046642));
#26276=CARTESIAN_POINT('Ctrl Pts',(0.00689426548978842,-0.0397182743898623,
-0.0112818457453296));
#26277=CARTESIAN_POINT('Ctrl Pts',(0.00669183407618031,-0.0397363381503545,
-0.011079355924058));
#26278=CARTESIAN_POINT('Ctrl Pts',(0.00641718620603428,-0.0397544019108467,
-0.010948193571508));
#26279=CARTESIAN_POINT('Ctrl Pts',(0.00613199067792525,-0.0397724656713389,
-0.0109182608601572));
#26280=CARTESIAN_POINT('Ctrl Pts',(0.00608826391408728,-0.03977523524418,
-0.0109136715154051));
#26281=CARTESIAN_POINT('Ctrl Pts',(0.00604432681486676,-0.0397780048170212,
-0.0109113682422291));
#26282=CARTESIAN_POINT('Ctrl Pts',(0.00600042870982249,-0.0397807743898623,
-0.0109113533592319));
#26283=CARTESIAN_POINT('Ctrl Pts',(0.00571517052474766,-0.0397987715977441,
-0.0109112566467029));
#26284=CARTESIAN_POINT('Ctrl Pts',(0.00542915007564361,-0.0398167688056259,
-0.0110119423676297));
#26285=CARTESIAN_POINT('Ctrl Pts',(0.00520670319655887,-0.0398347660135076,
-0.0111911500664709));
#26286=CARTESIAN_POINT('Ctrl Pts',(0.00517164846698451,-0.0398376021389592,
-0.0112193908646622));
#26287=CARTESIAN_POINT('Ctrl Pts',(0.00513813070007935,-0.0398404382644107,
-0.0112494837139568));
#26288=CARTESIAN_POINT('Ctrl Pts',(0.00510634091554443,-0.0398432743898623,
-0.0112812395761948));
#26289=CARTESIAN_POINT('Ctrl Pts',(0.00490082713907305,-0.0398616093002942,
-0.0114865340526787));
#26290=CARTESIAN_POINT('Ctrl Pts',(0.00476881314118491,-0.0398799442107259,
-0.0117658908578301));
#26291=CARTESIAN_POINT('Ctrl Pts',(0.00474119222774112,-0.0398982791211577,
-0.0120560065406672));
#26292=CARTESIAN_POINT('Ctrl Pts',(0.0047374284393678,-0.0399007775440592,
-0.0120955394126051));
#26293=CARTESIAN_POINT('Ctrl Pts',(0.00473552925481075,-0.0399032759669608,
-0.0121352414295939));
#26294=CARTESIAN_POINT('Ctrl Pts',(0.00473550033564982,-0.0399057743898623,
-0.0121749319515005));
#26295=CARTESIAN_POINT('Origin',(0.006,-0.0412787743898723,-0.0121758532865581));
#26296=CARTESIAN_POINT('',(0.004735500019377,-0.0404057743898623,-0.0121756319171353));
#26297=CARTESIAN_POINT('',(0.00473550010973655,-0.0403432744616866,-0.0121763800917601));
#26298=CARTESIAN_POINT('',(0.0047355,-0.0412787743898723,-0.0121758532865581));
#26299=CARTESIAN_POINT('',(0.00510586347519225,-0.0408432743898673,-0.0112817167617504));
#26300=CARTESIAN_POINT('Ctrl Pts',(0.00473550000000687,-0.0404057879868072,
-0.0121758491190739));
#26301=CARTESIAN_POINT('Ctrl Pts',(0.00473549904534208,-0.0404240165869345,
-0.0124655139528556));
#26302=CARTESIAN_POINT('Ctrl Pts',(0.00483905593806693,-0.0404422451870618,
-0.0127544805821245));
#26303=CARTESIAN_POINT('Ctrl Pts',(0.00502252596838094,-0.0404604737871891,
-0.0129780407755595));
#26304=CARTESIAN_POINT('Ctrl Pts',(0.00520599599869494,-0.0404787023873164,
-0.0132016009689945));
#26305=CARTESIAN_POINT('Ctrl Pts',(0.00546957359064989,-0.0404969309874437,
-0.0133596172042219));
#26306=CARTESIAN_POINT('Ctrl Pts',(0.00575330522225602,-0.040515159587571,
-0.0134160556638473));
#26307=CARTESIAN_POINT('Ctrl Pts',(0.00603703685386215,-0.0405333881876983,
-0.0134724941234728));
#26308=CARTESIAN_POINT('Ctrl Pts',(0.00634094837841056,-0.0405516167878256,
-0.0134274133698865));
#26309=CARTESIAN_POINT('Ctrl Pts',(0.00659607887659464,-0.0405698453879529,
-0.0132910439531608));
#26310=CARTESIAN_POINT('Ctrl Pts',(0.00685120937477873,-0.0405880739880802,
-0.013154674536435));
#26311=CARTESIAN_POINT('Ctrl Pts',(0.00705754117506496,-0.0406063025882075,
-0.012927019531437));
#26312=CARTESIAN_POINT('Ctrl Pts',(0.00716824487144537,-0.0406245311883348,
-0.0126597584119098));
#26313=CARTESIAN_POINT('Ctrl Pts',(0.00727894856782577,-0.0406427597884621,
-0.0123924972923825));
#26314=CARTESIAN_POINT('Ctrl Pts',(0.00729402736185934,-0.0406609883885893,
-0.0120856223291149));
#26315=CARTESIAN_POINT('Ctrl Pts',(0.00721005150819125,-0.0406792169887166,
-0.0118087898076828));
#26316=CARTESIAN_POINT('Ctrl Pts',(0.00712607565452316,-0.0406974455888439,
-0.0115319572862506));
#26317=CARTESIAN_POINT('Ctrl Pts',(0.00694305547450676,-0.0407156741889712,
-0.0112851818766085));
#26318=CARTESIAN_POINT('Ctrl Pts',(0.00670251942593715,-0.0407339027890985,
-0.0111244605406344));
#26319=CARTESIAN_POINT('Ctrl Pts',(0.00646198337736753,-0.0407521313892258,
-0.0109637392046603));
#26320=CARTESIAN_POINT('Ctrl Pts',(0.00616387176926783,-0.0407703599893531,
-0.0108890950709833));
#26321=CARTESIAN_POINT('Ctrl Pts',(0.00587605784448035,-0.0407885885894804,
-0.0109174421486206));
#26322=CARTESIAN_POINT('Ctrl Pts',(0.00558824391969287,-0.0408068171896077,
-0.0109457892262579));
#26323=CARTESIAN_POINT('Ctrl Pts',(0.00531068744342894,-0.040825045789735,
-0.0110768927935084));
#26324=CARTESIAN_POINT('Ctrl Pts',(0.00510586347518962,-0.0408432743898623,
-0.0112817167617477));
#26325=CARTESIAN_POINT('',(0.00473533362745302,-0.0408432571870886,-0.0121758704359914));
#26326=CARTESIAN_POINT('Origin',(0.00600000000001,-0.0408432743898623,-0.0121758532865681));
#26327=CARTESIAN_POINT('Ctrl Pts',(0.00473550000001551,-0.0408432557077308,
-0.0121758470227837));
#26328=CARTESIAN_POINT('Ctrl Pts',(0.00473550144284202,-0.0408249249258773,
-0.011884576297668));
#26329=CARTESIAN_POINT('Ctrl Pts',(0.00484035572904346,-0.0408065941440237,
-0.0115938173109497));
#26330=CARTESIAN_POINT('Ctrl Pts',(0.00502575520119273,-0.0407882633621702,
-0.0113697470144097));
#26331=CARTESIAN_POINT('Ctrl Pts',(0.00505105839927943,-0.0407857615891126,
-0.0113391660476304));
#26332=CARTESIAN_POINT('Ctrl Pts',(0.00507778904461344,-0.0407832598160549,
-0.0113097938647511));
#26333=CARTESIAN_POINT('Ctrl Pts',(0.00510582088914852,-0.0407807580429973,
-0.0112817593498172));
#26334=CARTESIAN_POINT('Ctrl Pts',(0.00530742913308967,-0.0407627650039641,
-0.0110801319000609));
#26335=CARTESIAN_POINT('Ctrl Pts',(0.0055808547532575,-0.040744771964931,
-0.0109490995219394));
#26336=CARTESIAN_POINT('Ctrl Pts',(0.00586496058746709,-0.0407267789258978,
-0.0109185845773862));
#26337=CARTESIAN_POINT('Ctrl Pts',(0.00590979587214559,-0.0407239394100198,
-0.0109137689556662));
#26338=CARTESIAN_POINT('Ctrl Pts',(0.00595485681374009,-0.0407210998941418,
-0.0109113578041007));
#26339=CARTESIAN_POINT('Ctrl Pts',(0.00599987328184339,-0.0407182603782637,
-0.0109113532929074));
#26340=CARTESIAN_POINT('Ctrl Pts',(0.00628618228829214,-0.0407002007879828,
-0.0109113246012904));
#26341=CARTESIAN_POINT('Ctrl Pts',(0.00657312656936524,-0.0406821411977019,
-0.0110127880335355));
#26342=CARTESIAN_POINT('Ctrl Pts',(0.00679595286337989,-0.0406640816074211,
-0.0111932957618923));
#26343=CARTESIAN_POINT('Ctrl Pts',(0.00683016678642004,-0.0406613086427908,
-0.0112210118694256));
#26344=CARTESIAN_POINT('Ctrl Pts',(0.00686290871373913,-0.0406585356781604,
-0.0112504984712462));
#26345=CARTESIAN_POINT('Ctrl Pts',(0.00689399989489287,-0.0406557627135301,
-0.0112815801527049));
#26346=CARTESIAN_POINT('Ctrl Pts',(0.00709645054913169,-0.0406377065161534,
-0.011483968949549));
#26347=CARTESIAN_POINT('Ctrl Pts',(0.00722760643875915,-0.0406196503187767,
-0.0117585516667657));
#26348=CARTESIAN_POINT('Ctrl Pts',(0.00725757357256424,-0.0406015941214,
-0.0120436830948051));
#26349=CARTESIAN_POINT('Ctrl Pts',(0.00726218137984443,-0.0405988177638655,
-0.0120875254815505));
#26350=CARTESIAN_POINT('Ctrl Pts',(0.00726449093380774,-0.040596041406331,
-0.0121315794393803));
#26351=CARTESIAN_POINT('Ctrl Pts',(0.0072644999733317,-0.0405932650487966,
-0.0121755935864718));
#26352=CARTESIAN_POINT('Ctrl Pts',(0.00726455876238414,-0.0405752088514199,
-0.0124618420675824));
#26353=CARTESIAN_POINT('Ctrl Pts',(0.00716316620513801,-0.0405571526540431,
-0.0127487489303258));
#26354=CARTESIAN_POINT('Ctrl Pts',(0.00698274316807724,-0.0405390964566663,
-0.0129715769292868));
#26355=CARTESIAN_POINT('Ctrl Pts',(0.00695500095592264,-0.0405363200991319,
-0.0130058394143989));
#26356=CARTESIAN_POINT('Ctrl Pts',(0.00692548358500305,-0.0405335437415975,
-0.0130386266339102));
#26357=CARTESIAN_POINT('Ctrl Pts',(0.00689436714696436,-0.040530767384063,
-0.0130697591297154));
#26358=CARTESIAN_POINT('Ctrl Pts',(0.00669196161561386,-0.0405127077937821,
-0.0132722691132774));
#26359=CARTESIAN_POINT('Ctrl Pts',(0.00641733267734601,-0.0404946482035013,
-0.0134034624598366));
#26360=CARTESIAN_POINT('Ctrl Pts',(0.00613214402769639,-0.0404765886132204,
-0.0134334296086731));
#26361=CARTESIAN_POINT('Ctrl Pts',(0.00608835466004441,-0.0404738156485901,
-0.0134380309225735));
#26362=CARTESIAN_POINT('Ctrl Pts',(0.00604435407325099,-0.0404710426839597,
-0.0134403395736692));
#26363=CARTESIAN_POINT('Ctrl Pts',(0.00600039268201306,-0.0404682697193294,
-0.0134403532255857));
#26364=CARTESIAN_POINT('Ctrl Pts',(0.00571513876285686,-0.0404502766802965,
-0.0134404418092857));
#26365=CARTESIAN_POINT('Ctrl Pts',(0.00542912435281271,-0.0404322836412635,
-0.0133397507523118));
#26366=CARTESIAN_POINT('Ctrl Pts',(0.0052066836807388,-0.0404142906022307,
-0.0131605407839875));
#26367=CARTESIAN_POINT('Ctrl Pts',(0.0051715798931479,-0.0404114510863525,
-0.0131322593163783));
#26368=CARTESIAN_POINT('Ctrl Pts',(0.00513801746798488,-0.0404086115704742,
-0.0131021205785883));
#26369=CARTESIAN_POINT('Ctrl Pts',(0.00510618821846458,-0.0404057720545959,
-0.0130703144367421));
#26370=CARTESIAN_POINT('Ctrl Pts',(0.00490071127995417,-0.0403874412727424,
-0.0128649866721582));
#26371=CARTESIAN_POINT('Ctrl Pts',(0.00476874496696427,-0.0403691104908888,
-0.012585609720854));
#26372=CARTESIAN_POINT('Ctrl Pts',(0.00474117235696595,-0.0403507797090353,
-0.0122954911364775));
#26373=CARTESIAN_POINT('Ctrl Pts',(0.00473740930129016,-0.040348277959919,
-0.0122558963217082));
#26374=CARTESIAN_POINT('Ctrl Pts',(0.00473551667089936,-0.0403457762108028,
-0.0122161321452331));
#26375=CARTESIAN_POINT('Ctrl Pts',(0.00473550010973655,-0.0403432744616866,
-0.0121763800917601));
#26376=CARTESIAN_POINT('Origin',(-0.0125,-0.0412787743898723,-0.0121758532865581));
#26377=CARTESIAN_POINT('',(-0.0137644998890966,-0.0306412974549308,-0.0121754725361131));
#26378=CARTESIAN_POINT('',(-0.013764499947573,-0.0305787585919128,-0.0121761158277784));
#26379=CARTESIAN_POINT('',(-0.0137645,-0.0412787743898723,-0.0121758532865581));
#26380=CARTESIAN_POINT('',(-0.0123336368679221,-0.0302142743898643,-0.0134293617860556));
#26381=CARTESIAN_POINT('Ctrl Pts',(-0.0137644999999586,-0.0305787427939633,
-0.0121758635184457));
#26382=CARTESIAN_POINT('Ctrl Pts',(-0.013764502313608,-0.0305607502112303,
-0.0118899329282279));
#26383=CARTESIAN_POINT('Ctrl Pts',(-0.0136631184159084,-0.0305427576284972,
-0.0116030220978715));
#26384=CARTESIAN_POINT('Ctrl Pts',(-0.0134829588914643,-0.0305247650457642,
-0.0113803961427148));
#26385=CARTESIAN_POINT('Ctrl Pts',(-0.0133590002535709,-0.0305123852614888,
-0.0112272185061392));
#26386=CARTESIAN_POINT('Ctrl Pts',(-0.0131991673647667,-0.0305000054772134,
-0.0111044564592225));
#26387=CARTESIAN_POINT('Ctrl Pts',(-0.0130221765475669,-0.0304876256929381,
-0.0110242058130789));
#26388=CARTESIAN_POINT('Ctrl Pts',(-0.0127747915104563,-0.0304703221206916,
-0.0109120372306151));
#26389=CARTESIAN_POINT('Ctrl Pts',(-0.0124846583937566,-0.0304530185484451,
-0.0108815539625805));
#26390=CARTESIAN_POINT('Ctrl Pts',(-0.0122152033504749,-0.0304357149761986,
-0.0109438422807553));
#26391=CARTESIAN_POINT('Ctrl Pts',(-0.0120116931961525,-0.0304226461814367,
-0.0109908865115473));
#26392=CARTESIAN_POINT('Ctrl Pts',(-0.0118210695107719,-0.0304095773866747,
-0.0110895293206415));
#26393=CARTESIAN_POINT('Ctrl Pts',(-0.0116667589653249,-0.0303965085919128,
-0.0112247120624838));
#26394=CARTESIAN_POINT('Ctrl Pts',(-0.011462446041281,-0.0303792050196663,
-0.0114036990603331));
#26395=CARTESIAN_POINT('Ctrl Pts',(-0.0113148742128925,-0.0303619014474198,
-0.0116553505295554));
#26396=CARTESIAN_POINT('Ctrl Pts',(-0.0112603333855932,-0.0303445978751733,
-0.0119264802023544));
#26397=CARTESIAN_POINT('Ctrl Pts',(-0.0112191405689906,-0.0303315290804114,
-0.0121312551469266));
#26398=CARTESIAN_POINT('Ctrl Pts',(-0.011230262856726,-0.0303184602856495,
-0.0123456017572798));
#26399=CARTESIAN_POINT('Ctrl Pts',(-0.011289660285933,-0.0303053914908876,
-0.0125419653275403));
#26400=CARTESIAN_POINT('Ctrl Pts',(-0.0113714362399216,-0.0302873989081545,
-0.0128123106690992));
#26401=CARTESIAN_POINT('Ctrl Pts',(-0.0115490474424576,-0.0302694063254215,
-0.0130573513611474));
#26402=CARTESIAN_POINT('Ctrl Pts',(-0.0117859367401441,-0.0302514137426883,
-0.0132194403269739));
#26403=CARTESIAN_POINT('Ctrl Pts',(-0.0119489282598164,-0.030239033958413,
-0.0133309655293373));
#26404=CARTESIAN_POINT('Ctrl Pts',(-0.0121386126078993,-0.0302266541741377,
-0.0134034785576961));
#26405=CARTESIAN_POINT('Ctrl Pts',(-0.0123336368679193,-0.0302142743898623,
-0.0134293617860444));
#26406=CARTESIAN_POINT('',(-0.0132689117770196,-0.0302142793348334,-0.0131800804819545));
#26407=CARTESIAN_POINT('Origin',(-0.01249999999999,-0.0302142743898623,
-0.0121758532865681));
#26408=CARTESIAN_POINT('Ctrl Pts',(-0.0132687256619633,-0.0302142800428447,
-0.0131798558297018));
#26409=CARTESIAN_POINT('Ctrl Pts',(-0.0130442789756256,-0.0302320714739704,
-0.0133517059198322));
#26410=CARTESIAN_POINT('Ctrl Pts',(-0.0127604773556288,-0.0302498629050961,
-0.0134450228840146));
#26411=CARTESIAN_POINT('Ctrl Pts',(-0.01247824326561,-0.0302676543362219,
-0.0134401661016908));
#26412=CARTESIAN_POINT('Ctrl Pts',(-0.0121960091755913,-0.0302854457673476,
-0.0134353093193669));
#26413=CARTESIAN_POINT('Ctrl Pts',(-0.0119153315214627,-0.0303032371984734,
-0.0133320736205398));
#26414=CARTESIAN_POINT('Ctrl Pts',(-0.0116971852644419,-0.0303210286295991,
-0.0131528122162838));
#26415=CARTESIAN_POINT('Ctrl Pts',(-0.0114790390074211,-0.0303388200607248,
-0.0129735508120277));
#26416=CARTESIAN_POINT('Ctrl Pts',(-0.0113233711528139,-0.0303566114918506,
-0.0127182793274862));
#26417=CARTESIAN_POINT('Ctrl Pts',(-0.0112638836495351,-0.0303744029229763,
-0.0124422676595061));
#26418=CARTESIAN_POINT('Ctrl Pts',(-0.0112043961462563,-0.030392194354102,
-0.0121662559915259));
#26419=CARTESIAN_POINT('Ctrl Pts',(-0.0112410972350849,-0.0304099857852278,
-0.0118695173223329));
#26420=CARTESIAN_POINT('Ctrl Pts',(-0.0113660322898324,-0.0304277772163535,
-0.0116163200147169));
#26421=CARTESIAN_POINT('Ctrl Pts',(-0.01149096734458,-0.0304455686474792,
-0.0113631227071009));
#26422=CARTESIAN_POINT('Ctrl Pts',(-0.0117041396255603,-0.030463360078605,
-0.0111534601536076));
#26423=CARTESIAN_POINT('Ctrl Pts',(-0.011959383315386,-0.0304811515097307,
-0.011032746182951));
#26424=CARTESIAN_POINT('Ctrl Pts',(-0.0122146270052117,-0.0304989429408564,
-0.0109120322122944));
#26425=CARTESIAN_POINT('Ctrl Pts',(-0.0125119266283734,-0.0305167343719822,
-0.0108802683043807));
#26426=CARTESIAN_POINT('Ctrl Pts',(-0.0127869140293121,-0.0305345258031079,
-0.0109443336603304));
#26427=CARTESIAN_POINT('Ctrl Pts',(-0.0130619014302509,-0.0305523172342336,
-0.0110083990162802));
#26428=CARTESIAN_POINT('Ctrl Pts',(-0.013314596450261,-0.0305701086653594,
-0.0111683452006722));
#26429=CARTESIAN_POINT('Ctrl Pts',(-0.0134901617902954,-0.0305879000964851,
-0.0113893802234218));
#26430=CARTESIAN_POINT('Ctrl Pts',(-0.0136657271303297,-0.0306056915276108,
-0.0116104152461713));
#26431=CARTESIAN_POINT('Ctrl Pts',(-0.0137643323694026,-0.0306234829587366,
-0.0118924230867439));
#26432=CARTESIAN_POINT('Ctrl Pts',(-0.0137644997782563,-0.0306412743898623,
-0.0121751044275857));
#26433=CARTESIAN_POINT('Origin',(-0.0125,-0.0412787743898723,-0.0121758532865581));
#26434=CARTESIAN_POINT('',(-0.0137647273224036,-0.0311411440628488,-0.012176494611068));
#26435=CARTESIAN_POINT('',(-0.01376449983248,-0.0310787450976138,-0.0121763100166715));
#26436=CARTESIAN_POINT('',(-0.0137645,-0.0412787743898723,-0.0121758532865581));
#26437=CARTESIAN_POINT('Ctrl Pts',(-0.0137644999999806,-0.0310787158053654,
-0.0121758462757411));
#26438=CARTESIAN_POINT('Ctrl Pts',(-0.0137644983850769,-0.0310603865105392,
-0.0118845755643713));
#26439=CARTESIAN_POINT('Ctrl Pts',(-0.0136596439362594,-0.0310420572157129,
-0.0115938166505956));
#26440=CARTESIAN_POINT('Ctrl Pts',(-0.0134742443467336,-0.0310237279208867,
-0.0113697464680424));
#26441=CARTESIAN_POINT('Ctrl Pts',(-0.0134489408557085,-0.0310212263234003,
-0.0113391651821412));
#26442=CARTESIAN_POINT('Ctrl Pts',(-0.0134222098869974,-0.0310187247259139,
-0.0113097927073432));
#26443=CARTESIAN_POINT('Ctrl Pts',(-0.0133941776929318,-0.0310162231284275,
-0.0112817579317647));
#26444=CARTESIAN_POINT('Ctrl Pts',(-0.013192569150655,-0.0309982315498371,
-0.0110801308231549));
#26445=CARTESIAN_POINT('Ctrl Pts',(-0.0129191433525998,-0.0309802399712467,
-0.0109490988803221));
#26446=CARTESIAN_POINT('Ctrl Pts',(-0.0126350374955696,-0.0309622483926564,
-0.0109185843714925));
#26447=CARTESIAN_POINT('Ctrl Pts',(-0.0125902017600955,-0.0309594090789341,
-0.0109137687705038));
#26448=CARTESIAN_POINT('Ctrl Pts',(-0.0125451403669309,-0.0309565697652119,
-0.0109113576876354));
#26449=CARTESIAN_POINT('Ctrl Pts',(-0.0125001234545288,-0.0309537304514896,
-0.0109113532925846));
#26450=CARTESIAN_POINT('Ctrl Pts',(-0.0122138144764302,-0.030935672326955,
-0.0109113253399233));
#26451=CARTESIAN_POINT('Ctrl Pts',(-0.0119268704782712,-0.0309176142024204,
-0.0110127894939568));
#26452=CARTESIAN_POINT('Ctrl Pts',(-0.011704044657302,-0.0308995560778858,
-0.0111932977703503));
#26453=CARTESIAN_POINT('Ctrl Pts',(-0.01166983045885,-0.0308967833101078,
-0.0112210142439792));
#26454=CARTESIAN_POINT('Ctrl Pts',(-0.0116370882903576,-0.0308940105423297,
-0.0112505012439437));
#26455=CARTESIAN_POINT('Ctrl Pts',(-0.0116059969071438,-0.0308912377745517,
-0.0112815833497026));
#26456=CARTESIAN_POINT('Ctrl Pts',(-0.0114035469962073,-0.0308731830426072,
-0.0114839728509779));
#26457=CARTESIAN_POINT('Ctrl Pts',(-0.0112723920900571,-0.0308551283106627,
-0.0117585560098165));
#26458=CARTESIAN_POINT('Ctrl Pts',(-0.0112424259622087,-0.0308370735787181,
-0.0120436875214248));
#26459=CARTESIAN_POINT('Ctrl Pts',(-0.0112378182628657,-0.03083429741835,
-0.012087530365764));
#26460=CARTESIAN_POINT('Ctrl Pts',(-0.0112355088639121,-0.0308315212579819,
-0.0121315847773326));
#26461=CARTESIAN_POINT('Ctrl Pts',(-0.0112355000254944,-0.0308287450976138,
-0.0121755993666846));
#26462=CARTESIAN_POINT('Ctrl Pts',(-0.0112354425449309,-0.0308106903656693,
-0.0124618478203132));
#26463=CARTESIAN_POINT('Ctrl Pts',(-0.011336836395326,-0.0307926356337248,
-0.0127487541990847));
#26464=CARTESIAN_POINT('Ctrl Pts',(-0.0115172604246094,-0.0307745809017803,
-0.0129715813663448));
#26465=CARTESIAN_POINT('Ctrl Pts',(-0.0115450030707529,-0.0307718047414122,
-0.0130058440711354));
#26466=CARTESIAN_POINT('Ctrl Pts',(-0.0115745209047644,-0.030769028581044,
-0.0130386314725521));
#26467=CARTESIAN_POINT('Ctrl Pts',(-0.0116056378287405,-0.0307662524206759,
-0.0130697641079603));
#26468=CARTESIAN_POINT('Ctrl Pts',(-0.0118080444673294,-0.0307481942961413,
-0.0132722729448952));
#26469=CARTESIAN_POINT('Ctrl Pts',(-0.0120826741077508,-0.0307301361716068,
-0.0134034647611449));
#26470=CARTESIAN_POINT('Ctrl Pts',(-0.0123678628998988,-0.0307120780470722,
-0.0134334303365939));
#26471=CARTESIAN_POINT('Ctrl Pts',(-0.0124116527348847,-0.0307093052792942,
-0.0134380314557133));
#26472=CARTESIAN_POINT('Ctrl Pts',(-0.0124556537806187,-0.0307065325115161,
-0.0134403398645289));
#26473=CARTESIAN_POINT('Ctrl Pts',(-0.0124996156147847,-0.0307037597437381,
-0.013440353228135));
#26474=CARTESIAN_POINT('Ctrl Pts',(-0.0127848695046488,-0.0306857681651477,
-0.0134404399401816));
#26475=CARTESIAN_POINT('Ctrl Pts',(-0.0130708832318396,-0.0306677765865574,
-0.013339747026259));
#26476=CARTESIAN_POINT('Ctrl Pts',(-0.0132933227203511,-0.030649785007967,
-0.0131605356268967));
#26477=CARTESIAN_POINT('Ctrl Pts',(-0.0133284266712874,-0.0306469456942447,
-0.0131322536513692));
#26478=CARTESIAN_POINT('Ctrl Pts',(-0.0133619892171701,-0.0306441063805225,
-0.0131021143789215));
#26479=CARTESIAN_POINT('Ctrl Pts',(-0.0133938185404324,-0.0306412670668002,
-0.013070307682701));
#26480=CARTESIAN_POINT('Ctrl Pts',(-0.0135992939148588,-0.0306229377719739,
-0.0128649783779801));
#26481=CARTESIAN_POINT('Ctrl Pts',(-0.0137312581167778,-0.0306046084771476,
-0.0125856004461779));
#26482=CARTESIAN_POINT('Ctrl Pts',(-0.0137588285430525,-0.0305862791823214,
-0.012295481666119));
#26483=CARTESIAN_POINT('Ctrl Pts',(-0.0137625913778871,-0.030583777584835,
-0.0122558860123952));
#26484=CARTESIAN_POINT('Ctrl Pts',(-0.0137644837095114,-0.0305812759873487,
-0.0122161210040892));
#26485=CARTESIAN_POINT('Ctrl Pts',(-0.0137644998951874,-0.0305787743898623,
-0.0121763681371112));
#26486=CARTESIAN_POINT('Ctrl Pts',(-0.0137644999999368,-0.0306413205199993,
-0.0121758406446405));
#26487=CARTESIAN_POINT('Ctrl Pts',(-0.0137645029300491,-0.0306597087123115,
-0.0124689233200942));
#26488=CARTESIAN_POINT('Ctrl Pts',(-0.0136584023059271,-0.0306781182315215,
-0.0127613134836949));
#26489=CARTESIAN_POINT('Ctrl Pts',(-0.0134708289910776,-0.0306965228322482,
-0.0129860701217839));
#26490=CARTESIAN_POINT('Ctrl Pts',(-0.0134465321684366,-0.0306989068244488,
-0.0130151833897208));
#26491=CARTESIAN_POINT('Ctrl Pts',(-0.0134209340716843,-0.0307012907341239,
-0.0130431918626772));
#26492=CARTESIAN_POINT('Ctrl Pts',(-0.0133941432291651,-0.0307036745042324,
-0.0130699831069635));
#26493=CARTESIAN_POINT('Ctrl Pts',(-0.0131934054241877,-0.0307215355617486,
-0.0132707239222924));
#26494=CARTESIAN_POINT('Ctrl Pts',(-0.0129214992936078,-0.030739388783757,
-0.0134014108571587));
#26495=CARTESIAN_POINT('Ctrl Pts',(-0.0126391600155025,-0.0307573061545645,
-0.0134326725814789));
#26496=CARTESIAN_POINT('Ctrl Pts',(-0.0125929135130964,-0.0307602409772988,
-0.0134377931775883));
#26497=CARTESIAN_POINT('Ctrl Pts',(-0.0125464294253273,-0.0307631775211235,
-0.013440353054484));
#26498=CARTESIAN_POINT('Ctrl Pts',(-0.0125000063209412,-0.0307661161023836,
-0.0134403532865423));
#26499=CARTESIAN_POINT('Ctrl Pts',(-0.012224309899828,-0.030783567678431,
-0.0134403546646845));
#26500=CARTESIAN_POINT('Ctrl Pts',(-0.0119465654693464,-0.0308010911129074,
-0.0133458957658519));
#26501=CARTESIAN_POINT('Ctrl Pts',(-0.0117277890330815,-0.0308184434524664,
-0.0131771776458797));
#26502=CARTESIAN_POINT('Ctrl Pts',(-0.0116848234390513,-0.0308218512855479,
-0.0131440430251133));
#26503=CARTESIAN_POINT('Ctrl Pts',(-0.0116440699024505,-0.0308252525196365,
-0.0131081960476507));
#26504=CARTESIAN_POINT('Ctrl Pts',(-0.0116058657099795,-0.030828645314453,
-0.0130699920461528));
#26505=CARTESIAN_POINT('Ctrl Pts',(-0.011489497681923,-0.0308389795949825,
-0.0129536245997907));
#26506=CARTESIAN_POINT('Ctrl Pts',(-0.0113964889249869,-0.0308492355775799,
-0.0128160390688021));
#26507=CARTESIAN_POINT('Ctrl Pts',(-0.011331754935869,-0.030859942775707,
-0.0126597579467274));
#26508=CARTESIAN_POINT('Ctrl Pts',(-0.0112670209467511,-0.0308706499738341,
-0.0125034768246526));
#26509=CARTESIAN_POINT('Ctrl Pts',(-0.0112355,-0.030881808387491,-0.0123257398452038));
#26510=CARTESIAN_POINT('Ctrl Pts',(-0.0112355,-0.0308912621404406,-0.0121758532865581));
#26511=CARTESIAN_POINT('Ctrl Pts',(-0.0112355,-0.0309007158933902,-0.0120259667279124));
#26512=CARTESIAN_POINT('Ctrl Pts',(-0.0112576964300095,-0.0309084649856326,
-0.0119036839263425));
#26513=CARTESIAN_POINT('Ctrl Pts',(-0.0113007457940289,-0.0309169920427827,
-0.0117749173821287));
#26514=CARTESIAN_POINT('Ctrl Pts',(-0.0113437951580483,-0.0309255190999327,
-0.0116461508379148));
#26515=CARTESIAN_POINT('Ctrl Pts',(-0.0114125317794308,-0.0309348241219903,
-0.0115133602798955));
#26516=CARTESIAN_POINT('Ctrl Pts',(-0.0115051746667562,-0.0309442973412607,
-0.0113952875901965));
#26517=CARTESIAN_POINT('Ctrl Pts',(-0.011680968239998,-0.0309622731526125,
-0.0111712399528259));
#26518=CARTESIAN_POINT('Ctrl Pts',(-0.0119429575015307,-0.0309808545845356,
-0.0109986148069392));
#26519=CARTESIAN_POINT('Ctrl Pts',(-0.0122485416715191,-0.0310004508145921,
-0.0109366079682141));
#26520=CARTESIAN_POINT('Ctrl Pts',(-0.012265042084108,-0.0310015089383854,
-0.0109332598287396));
#26521=CARTESIAN_POINT('Ctrl Pts',(-0.0122816566882631,-0.0310025700209238,
-0.0109302316696991));
#26522=CARTESIAN_POINT('Ctrl Pts',(-0.012298374142954,-0.0310036341266249,
-0.0109275315076203));
#26523=CARTESIAN_POINT('Ctrl Pts',(-0.0125577285204244,-0.0310201426488116,
-0.0108856412277915));
#26524=CARTESIAN_POINT('Ctrl Pts',(-0.0128442652884611,-0.0310373787972624,
-0.0109263878319273));
#26525=CARTESIAN_POINT('Ctrl Pts',(-0.0130949673908159,-0.0310552769721772,
-0.0110600692331384));
#26526=CARTESIAN_POINT('Ctrl Pts',(-0.0131597001439185,-0.0310598983859064,
-0.0110945865549228));
#26527=CARTESIAN_POINT('Ctrl Pts',(-0.0132219563480234,-0.0310645639371177,
-0.011135041042932));
#26528=CARTESIAN_POINT('Ctrl Pts',(-0.013280570940992,-0.0310692724965332,
-0.0111810320684094));
#26529=CARTESIAN_POINT('Ctrl Pts',(-0.0134918342552102,-0.0310862434557593,
-0.011346796530373));
#26530=CARTESIAN_POINT('Ctrl Pts',(-0.0136575068172827,-0.0311037731269602,
-0.0115906304950738));
#26531=CARTESIAN_POINT('Ctrl Pts',(-0.0137271531481506,-0.0311218791353568,
-0.0118708034529504));
#26532=CARTESIAN_POINT('Ctrl Pts',(-0.0137516666134372,-0.0311282519191458,
-0.0119694161148319));
#26533=CARTESIAN_POINT('Ctrl Pts',(-0.0137645010939262,-0.0311346961015161,
-0.0120721097217937));
#26534=CARTESIAN_POINT('Ctrl Pts',(-0.0137644999999297,-0.0311412124509856,
-0.012175866619248));
#26535=CARTESIAN_POINT('Origin',(-0.0125,-0.0412787743898723,-0.0121758532865581));
#26536=CARTESIAN_POINT('',(-0.013764499973714,-0.0316412626404869,-0.0121760322553932));
#26537=CARTESIAN_POINT('',(-0.0137644998147527,-0.0315788051416157,-0.0121753723444795));
#26538=CARTESIAN_POINT('',(-0.0137645,-0.0412787743898723,-0.0121758532865581));
#26539=CARTESIAN_POINT('Ctrl Pts',(-0.0137644996295201,-0.0315787743898623,
-0.0121748853280777));
#26540=CARTESIAN_POINT('Ctrl Pts',(-0.0137642766641099,-0.0315604396759252,
-0.0118836128362491));
#26541=CARTESIAN_POINT('Ctrl Pts',(-0.0136592000410348,-0.0315421049619881,
-0.0115929321979826));
#26542=CARTESIAN_POINT('Ctrl Pts',(-0.0134736281878384,-0.0315237702480509,
-0.0113690023698167));
#26543=CARTESIAN_POINT('Ctrl Pts',(-0.0134483388141738,-0.0315212716286547,
-0.0113384856454234));
#26544=CARTESIAN_POINT('Ctrl Pts',(-0.0134216271051845,-0.0315187730092585,
-0.0113091752375175));
#26545=CARTESIAN_POINT('Ctrl Pts',(-0.0133936188401708,-0.0315162743898623,
-0.0112811993766623));
#26546=CARTESIAN_POINT('Ctrl Pts',(-0.0131918814404613,-0.0314982773814931,
-0.0110796953770112));
#26547=CARTESIAN_POINT('Ctrl Pts',(-0.0129183697591856,-0.031480280373124,
-0.0109488340864079));
#26548=CARTESIAN_POINT('Ctrl Pts',(-0.0126342414202779,-0.0314622833647548,
-0.0109184991236104));
#26549=CARTESIAN_POINT('Ctrl Pts',(-0.0125894628501879,-0.0314594470397906,
-0.0109137183394654));
#26550=CARTESIAN_POINT('Ctrl Pts',(-0.0125444607432362,-0.0314566107148265,
-0.0109113357548491));
#26551=CARTESIAN_POINT('Ctrl Pts',(-0.0124995041488628,-0.0314537743898623,
-0.0109113533837777));
#26552=CARTESIAN_POINT('Ctrl Pts',(-0.0122131913331388,-0.0314357108288182,
-0.0109114656562539));
#26553=CARTESIAN_POINT('Ctrl Pts',(-0.0119262942079631,-0.0314176472677742,
-0.0110130728866724));
#26554=CARTESIAN_POINT('Ctrl Pts',(-0.0117035558497281,-0.0313995837067301,
-0.0111936939484171));
#26555=CARTESIAN_POINT('Ctrl Pts',(-0.0116694023109608,-0.0313968139344408,
-0.0112213894404884));
#26556=CARTESIAN_POINT('Ctrl Pts',(-0.0116367176417391,-0.0313940441621516,
-0.0112508498765764));
#26557=CARTESIAN_POINT('Ctrl Pts',(-0.0116056797895326,-0.0313912743898623,
-0.0112819004851476));
#26558=CARTESIAN_POINT('Ctrl Pts',(-0.011403299020959,-0.0313732142276789,
-0.011484364430962));
#26559=CARTESIAN_POINT('Ctrl Pts',(-0.0112722413007821,-0.0313551540654955,
-0.0117589978088282));
#26560=CARTESIAN_POINT('Ctrl Pts',(-0.0112423781627974,-0.0313370939033121,
-0.0120441431328445));
#26561=CARTESIAN_POINT('Ctrl Pts',(-0.0112377926229853,-0.0313343207321622,
-0.0120879277222667));
#26562=CARTESIAN_POINT('Ctrl Pts',(-0.011235499174881,-0.0313315475610122,
-0.0121319224740286));
#26563=CARTESIAN_POINT('Ctrl Pts',(-0.0112355000002229,-0.0313287743898623,
-0.012175877030283));
#26564=CARTESIAN_POINT('Ctrl Pts',(-0.0112355053752281,-0.0313107142276789,
-0.0124621292562503));
#26565=CARTESIAN_POINT('Ctrl Pts',(-0.0113369647137236,-0.0312926540654955,
-0.0127490161444656));
#26566=CARTESIAN_POINT('Ctrl Pts',(-0.0115174412457287,-0.031274593903312,
-0.0129718046320591));
#26567=CARTESIAN_POINT('Ctrl Pts',(-0.0115451537494544,-0.0312718207321621,
-0.0130060142144567));
#26568=CARTESIAN_POINT('Ctrl Pts',(-0.0115746362548937,-0.0312690475610122,
-0.0130387521283998));
#26569=CARTESIAN_POINT('Ctrl Pts',(-0.0116057133619614,-0.0312662743898623,
-0.0130698396729341));
#26570=CARTESIAN_POINT('Ctrl Pts',(-0.0118081398225887,-0.0312482108288182,
-0.0132723341199225));
#26571=CARTESIAN_POINT('Ctrl Pts',(-0.0120827843608681,-0.0312301472677741,
-0.0134035029559604));
#26572=CARTESIAN_POINT('Ctrl Pts',(-0.0123679789827087,-0.0312120837067301,
-0.0134334425283192));
#26573=CARTESIAN_POINT('Ctrl Pts',(-0.0124117092393669,-0.0312093139344408,
-0.0134380333062765));
#26574=CARTESIAN_POINT('Ctrl Pts',(-0.0124556499210143,-0.0312065441621516,
-0.0134403376404914));
#26575=CARTESIAN_POINT('Ctrl Pts',(-0.0124995516363092,-0.0312037743898623,
-0.0134403532070682));
#26576=CARTESIAN_POINT('Ctrl Pts',(-0.012784809576339,-0.0311857773814931,
-0.0134404543532215));
#26577=CARTESIAN_POINT('Ctrl Pts',(-0.0130708314094809,-0.031167780373124,
-0.0133397732383392));
#26578=CARTESIAN_POINT('Ctrl Pts',(-0.0132932810111053,-0.0311497833647548,
-0.0131605692290612));
#26579=CARTESIAN_POINT('Ctrl Pts',(-0.0133283390243824,-0.0311469470397906,
-0.0131323267125959));
#26580=CARTESIAN_POINT('Ctrl Pts',(-0.0133618598559568,-0.0311441107148265,
-0.0131022318210814));
#26581=CARTESIAN_POINT('Ctrl Pts',(-0.0133936524376684,-0.0311412743898623,
-0.0130704736365666));
#26582=CARTESIAN_POINT('Ctrl Pts',(-0.0135991676372248,-0.0311229396759248,
-0.0128651807890925));
#26583=CARTESIAN_POINT('Ctrl Pts',(-0.0137311837108138,-0.0311046049619872,
-0.0125858251007971));
#26584=CARTESIAN_POINT('Ctrl Pts',(-0.013758806849294,-0.0310862702480498,
-0.0122957097263953));
#26585=CARTESIAN_POINT('Ctrl Pts',(-0.0137625712772429,-0.0310837716286539,
-0.0122561733636258));
#26586=CARTESIAN_POINT('Ctrl Pts',(-0.0137644707703676,-0.0310812730092581,
-0.012216467811213));
#26587=CARTESIAN_POINT('Ctrl Pts',(-0.0137644996649794,-0.0310787743898623,
-0.0121767737576019));
#26588=CARTESIAN_POINT('Ctrl Pts',(-0.0137644996042272,-0.0311412743898623,
-0.0121768537410499));
#26589=CARTESIAN_POINT('Ctrl Pts',(-0.0137642691544413,-0.0311596061323621,
-0.0124681250237667));
#26590=CARTESIAN_POINT('Ctrl Pts',(-0.0136591858638433,-0.031177937874862,
-0.0127588019995018));
#26591=CARTESIAN_POINT('Ctrl Pts',(-0.0134736095695228,-0.0311962696173618,
-0.0129827266695208));
#26592=CARTESIAN_POINT('Ctrl Pts',(-0.0134482953225914,-0.0311987702290807,
-0.0130132719738746));
#26593=CARTESIAN_POINT('Ctrl Pts',(-0.0134215560483623,-0.0312012708407996,
-0.013042608617474));
#26594=CARTESIAN_POINT('Ctrl Pts',(-0.0133935178974578,-0.0312037714525185,
-0.0130706080110064));
#26595=CARTESIAN_POINT('Ctrl Pts',(-0.0131917596414352,-0.0312217654729198,
-0.0132720873748926));
#26596=CARTESIAN_POINT('Ctrl Pts',(-0.0129182358167704,-0.031239759493321,
-0.0134029176620471));
#26597=CARTESIAN_POINT('Ctrl Pts',(-0.0126341062951139,-0.0312577535137223,
-0.0134332218688007));
#26598=CARTESIAN_POINT('Ctrl Pts',(-0.0125892883827257,-0.0312605918475397,
-0.0134380019820229));
#26599=CARTESIAN_POINT('Ctrl Pts',(-0.0125442468058514,-0.0312634301813572,
-0.0134403797057756));
#26600=CARTESIAN_POINT('Ctrl Pts',(-0.0124992513169962,-0.0312662685151747,
-0.0134403530649186));
#26601=CARTESIAN_POINT('Ctrl Pts',(-0.0122129410176822,-0.0312843290858119,
-0.0134401835467751));
#26602=CARTESIAN_POINT('Ctrl Pts',(-0.0119260660550254,-0.0313023896564492,
-0.013338520601838));
#26603=CARTESIAN_POINT('Ctrl Pts',(-0.0117033644410345,-0.0313204502270865,
-0.0131578573782969));
#26604=CARTESIAN_POINT('Ctrl Pts',(-0.011669186081468,-0.0313232220106679,
-0.0131301307152342));
#26605=CARTESIAN_POINT('Ctrl Pts',(-0.0116364795416869,-0.0313259937942494,
-0.0131006362680639));
#26606=CARTESIAN_POINT('Ctrl Pts',(-0.0116054231994823,-0.0313287655778308,
-0.0130695493187611));
#26607=CARTESIAN_POINT('Ctrl Pts',(-0.0114031022707209,-0.0313468227535544,
-0.0128670289957348));
#26608=CARTESIAN_POINT('Ctrl Pts',(-0.0112721235294321,-0.031364879929278,
-0.0125923604050326));
#26609=CARTESIAN_POINT('Ctrl Pts',(-0.0112423410495547,-0.0313829371050016,
-0.0123072085847569));
#26610=CARTESIAN_POINT('Ctrl Pts',(-0.0112377638277925,-0.0313857122834967,
-0.0122633840569576));
#26611=CARTESIAN_POINT('Ctrl Pts',(-0.0112354828095669,-0.0313884874619919,
-0.0122193496457451));
#26612=CARTESIAN_POINT('Ctrl Pts',(-0.0112355000976358,-0.031391262640487,
-0.0121753563750721));
#26613=CARTESIAN_POINT('Ctrl Pts',(-0.011235612585427,-0.0314093198162106,
-0.0118891066002938));
#26614=CARTESIAN_POINT('Ctrl Pts',(-0.0113371776611666,-0.0314273769919342,
-0.0116022594903848));
#26615=CARTESIAN_POINT('Ctrl Pts',(-0.0115177352388894,-0.0314454341676578,
-0.0113795391594196));
#26616=CARTESIAN_POINT('Ctrl Pts',(-0.011545484844614,-0.0314482093461529,
-0.0113453096274937));
#26617=CARTESIAN_POINT('Ctrl Pts',(-0.0115750070352552,-0.031450984524648,
-0.0113125550224318));
#26618=CARTESIAN_POINT('Ctrl Pts',(-0.0116061258684813,-0.0314537597031431,
-0.0112814544454353));
#26619=CARTESIAN_POINT('Ctrl Pts',(-0.0118086439719538,-0.0314718202737804,
-0.0110790551515912));
#26620=CARTESIAN_POINT('Ctrl Pts',(-0.0120833465317326,-0.0314898808444177,
-0.0109480131716259));
#26621=CARTESIAN_POINT('Ctrl Pts',(-0.0123685528079687,-0.031507941415055,
-0.0109182039372929));
#26622=CARTESIAN_POINT('Ctrl Pts',(-0.0124123238542812,-0.0315107131986364,
-0.0109136290682061));
#26623=CARTESIAN_POINT('Ctrl Pts',(-0.0124563046506386,-0.0315134849822179,
-0.0109113447918782));
#26624=CARTESIAN_POINT('Ctrl Pts',(-0.0125002451399487,-0.0315162567657993,
-0.0109113533103199));
#26625=CARTESIAN_POINT('Ctrl Pts',(-0.0127855004774802,-0.0315342507862006,
-0.0109114086108182));
#26626=CARTESIAN_POINT('Ctrl Pts',(-0.0130714651086127,-0.0315522448066019,
-0.0110122448522433));
#26627=CARTESIAN_POINT('Ctrl Pts',(-0.0132938157207033,-0.0315702388270031,
-0.0111915683422639));
#26628=CARTESIAN_POINT('Ctrl Pts',(-0.0133288887753934,-0.0315730771608206,
-0.0112198544014457));
#26629=CARTESIAN_POINT('Ctrl Pts',(-0.0133624209683958,-0.031575915494638,
-0.0112499952146683));
#26630=CARTESIAN_POINT('Ctrl Pts',(-0.0133942208462703,-0.0315787538284555,
-0.0112818010911603));
#26631=CARTESIAN_POINT('Ctrl Pts',(-0.0135996044305191,-0.0315970855709553,
-0.0114872234182486));
#26632=CARTESIAN_POINT('Ctrl Pts',(-0.013731442931389,-0.0316154173134552,
-0.0117666614940349));
#26633=CARTESIAN_POINT('Ctrl Pts',(-0.0137588824248632,-0.031633749055955,
-0.0120567932581251));
#26634=CARTESIAN_POINT('Ctrl Pts',(-0.0137626254143222,-0.0316362496676739,
-0.0120963697953423));
#26635=CARTESIAN_POINT('Ctrl Pts',(-0.0137644997916104,-0.0316387502793927,
-0.012136114664894));
#26636=CARTESIAN_POINT('Ctrl Pts',(-0.0137644999999826,-0.0316412508911116,
-0.0121758466549596));
#26637=CARTESIAN_POINT('Origin',(-0.0125,-0.0412787743898723,-0.0121758532865581));
#26638=CARTESIAN_POINT('',(-0.0137644997244071,-0.0321413104439873,-0.0121752554129869));
#26639=CARTESIAN_POINT('',(-0.0137644999999678,-0.0320788036733635,-0.0121758442670768));
#26640=CARTESIAN_POINT('',(-0.0137645,-0.0412787743898723,-0.0121758532865581));
#26641=CARTESIAN_POINT('Ctrl Pts',(-0.0137644999101415,-0.0320787743898623,
-0.0121753765769045));
#26642=CARTESIAN_POINT('Ctrl Pts',(-0.0137643901026805,-0.0320604452955693,
-0.011884105939584));
#26643=CARTESIAN_POINT('Ctrl Pts',(-0.0136594276941949,-0.0320421162012764,
-0.0115933860367519));
#26644=CARTESIAN_POINT('Ctrl Pts',(-0.0134739449447686,-0.0320237871069834,
-0.0113693847536569));
#26645=CARTESIAN_POINT('Ctrl Pts',(-0.0134486290285339,-0.0320212854305892,
-0.0113388115723943));
#26646=CARTESIAN_POINT('Ctrl Pts',(-0.0134218859628255,-0.0320187837541949,
-0.0113094478347642));
#26647=CARTESIAN_POINT('Ctrl Pts',(-0.0133938420641875,-0.0320162820778007,
-0.0112814223980658));
#26648=CARTESIAN_POINT('Ctrl Pts',(-0.0131921579459829,-0.0319982906992082,
-0.0110798710531277));
#26649=CARTESIAN_POINT('Ctrl Pts',(-0.0129186831052984,-0.0319802993206158,
-0.01094894174627));
#26650=CARTESIAN_POINT('Ctrl Pts',(-0.0126345659150311,-0.0319623079420234,
-0.0109185338106444));
#26651=CARTESIAN_POINT('Ctrl Pts',(-0.012589726654944,-0.0319594685499286,
-0.0109137348425392));
#26652=CARTESIAN_POINT('Ctrl Pts',(-0.0125446626218893,-0.0319566291578338,
-0.0109113406619024));
#26653=CARTESIAN_POINT('Ctrl Pts',(-0.0124996439863367,-0.031953789765739,
-0.010911353336675));
#26654=CARTESIAN_POINT('Ctrl Pts',(-0.0122133351285606,-0.0319357318415605,
-0.010911433945508));
#26655=CARTESIAN_POINT('Ctrl Pts',(-0.0119264297054606,-0.0319176739173819,
-0.0110130068215275));
#26656=CARTESIAN_POINT('Ctrl Pts',(-0.0117036723726936,-0.0318996159932033,
-0.0111935994700785));
#26657=CARTESIAN_POINT('Ctrl Pts',(-0.0116694673396937,-0.0318968431466947,
-0.0112213299938127));
#26658=CARTESIAN_POINT('Ctrl Pts',(-0.0116367351231188,-0.031894070300186,
-0.0112508306247152));
#26659=CARTESIAN_POINT('Ctrl Pts',(-0.0116056544324338,-0.0318912974536774,
-0.0112819258533877));
#26660=CARTESIAN_POINT('Ctrl Pts',(-0.0114032821352834,-0.0318732429219011,
-0.0114843928101436));
#26661=CARTESIAN_POINT('Ctrl Pts',(-0.0112722324208137,-0.0318551883901249,
-0.0117590260799309));
#26662=CARTESIAN_POINT('Ctrl Pts',(-0.0112423754584874,-0.0318371338583486,
-0.0120441689572507));
#26663=CARTESIAN_POINT('Ctrl Pts',(-0.0112377843640408,-0.0318343576194376,
-0.0120880152757821));
#26664=CARTESIAN_POINT('Ctrl Pts',(-0.0112354918306623,-0.0318315813805267,
-0.01213207229806));
#26665=CARTESIAN_POINT('Ctrl Pts',(-0.0112355000218958,-0.0318288051416157,
-0.0121760886042277));
#26666=CARTESIAN_POINT('Ctrl Pts',(-0.0112355532914055,-0.0318107506098395,
-0.0124623369509536));
#26667=CARTESIAN_POINT('Ctrl Pts',(-0.0113370580676153,-0.0317926960780632,
-0.012749203999261));
#26668=CARTESIAN_POINT('Ctrl Pts',(-0.0115175681933444,-0.031774641546287,
-0.0129719613164581));
#26669=CARTESIAN_POINT('Ctrl Pts',(-0.0115453251709876,-0.031771865307376,
-0.0130062146296634));
#26670=CARTESIAN_POINT('Ctrl Pts',(-0.0115748569046832,-0.0317690890684651,
-0.01303899183759));
#26671=CARTESIAN_POINT('Ctrl Pts',(-0.0116059872059909,-0.0317663128295541,
-0.0130701135250502));
#26672=CARTESIAN_POINT('Ctrl Pts',(-0.011808472884889,-0.0317482549053755,
-0.0132725431755552));
#26673=CARTESIAN_POINT('Ctrl Pts',(-0.0120831536604284,-0.031730196981197,
-0.0134036276597726));
#26674=CARTESIAN_POINT('Ctrl Pts',(-0.0123683540459796,-0.0317121390570185,
-0.0134334818457082));
#26675=CARTESIAN_POINT('Ctrl Pts',(-0.012412147390415,-0.0317093662105098,
-0.0134380660423424));
#26676=CARTESIAN_POINT('Ctrl Pts',(-0.012456151066559,-0.0317065933640011,
-0.0134403572664768));
#26677=CARTESIAN_POINT('Ctrl Pts',(-0.0125001146216738,-0.0317038205174925,
-0.0134403532813631));
#26678=CARTESIAN_POINT('Ctrl Pts',(-0.0127853684075842,-0.0316858291389,
-0.0134403274242919));
#26679=CARTESIAN_POINT('Ctrl Pts',(-0.0130713422901893,-0.0316678377603076,
-0.0133395217256917));
#26680=CARTESIAN_POINT('Ctrl Pts',(-0.0132937110097133,-0.0316498463817151,
-0.0131602226700011));
#26681=CARTESIAN_POINT('Ctrl Pts',(-0.0133288051511152,-0.0316470069896203,
-0.0131319257655304));
#26682=CARTESIAN_POINT('Ctrl Pts',(-0.0133623570364164,-0.0316441675975256,
-0.0131017720295453));
#26683=CARTESIAN_POINT('Ctrl Pts',(-0.0133941749012707,-0.0316413282054308,
-0.013069951433261));
#26684=CARTESIAN_POINT('Ctrl Pts',(-0.0135995683889091,-0.0316229991111379,
-0.012864540313455));
#26685=CARTESIAN_POINT('Ctrl Pts',(-0.0137314212509396,-0.0316046700168449,
-0.0125851098820988));
#26686=CARTESIAN_POINT('Ctrl Pts',(-0.0137588760985249,-0.0315863409225519,
-0.012294980187646));
#26687=CARTESIAN_POINT('Ctrl Pts',(-0.0137626233182736,-0.0315838392461577,
-0.0122553813620694));
#26688=CARTESIAN_POINT('Ctrl Pts',(-0.0137644998090151,-0.0315813375697634,
-0.0122156139127346));
#26689=CARTESIAN_POINT('Ctrl Pts',(-0.0137644999999854,-0.0315788358933692,
-0.0121758593608812));
#26690=CARTESIAN_POINT('Ctrl Pts',(-0.0137644999474453,-0.0316412743898623,
-0.0121762178558267));
#26691=CARTESIAN_POINT('Ctrl Pts',(-0.0137644159704943,-0.0316596082582658,
-0.012467489938709));
#26692=CARTESIAN_POINT('Ctrl Pts',(-0.0136594783866661,-0.0316779421266695,
-0.0127582202982457));
#26693=CARTESIAN_POINT('Ctrl Pts',(-0.0134740139348575,-0.031696275995073,
-0.0129822384951919));
#26694=CARTESIAN_POINT('Ctrl Pts',(-0.0134487294786364,-0.0316987754600028,
-0.0130127790016781));
#26695=CARTESIAN_POINT('Ctrl Pts',(-0.0134220210203026,-0.0317012749249325,
-0.0130421129465654));
#26696=CARTESIAN_POINT('Ctrl Pts',(-0.0133940144252717,-0.0317037743898623,
-0.0130701118942361));
#26697=CARTESIAN_POINT('Ctrl Pts',(-0.0131923669146546,-0.0317217705397123,
-0.0132717043438519));
#26698=CARTESIAN_POINT('Ctrl Pts',(-0.0129189141847026,-0.0317397666895621,
-0.0134026865273691));
#26699=CARTESIAN_POINT('Ctrl Pts',(-0.0126348001866975,-0.031757762839412,
-0.0134331476672289));
#26700=CARTESIAN_POINT('Ctrl Pts',(-0.0125900081867821,-0.0317606000228954,
-0.013437950019044));
#26701=CARTESIAN_POINT('Ctrl Pts',(-0.0125449914289418,-0.0317634372063788,
-0.0134403526020235));
#26702=CARTESIAN_POINT('Ctrl Pts',(-0.012500019243202,-0.0317662743898623,
-0.0134403532864117));
#26703=CARTESIAN_POINT('Ctrl Pts',(-0.0122137074025703,-0.0317843370926638,
-0.0134403576435145));
#26704=CARTESIAN_POINT('Ctrl Pts',(-0.0119267696495195,-0.0318023997954653,
-0.0133388679488294));
#26705=CARTESIAN_POINT('Ctrl Pts',(-0.0117039579848907,-0.0318204624982669,
-0.01315833858425));
#26706=CARTESIAN_POINT('Ctrl Pts',(-0.0116697809955634,-0.0318232331287987,
-0.0131306472594858));
#26707=CARTESIAN_POINT('Ctrl Pts',(-0.0116370731965135,-0.0318260037593305,
-0.0131011891364016));
#26708=CARTESIAN_POINT('Ctrl Pts',(-0.0116060127928554,-0.0318287743898623,
-0.0130701391041029));
#26709=CARTESIAN_POINT('Ctrl Pts',(-0.0114035573189597,-0.0318468336953203,
-0.0128677512319839));
#26710=CARTESIAN_POINT('Ctrl Pts',(-0.0112723973787259,-0.0318648930007784,
-0.0125931676450612));
#26711=CARTESIAN_POINT('Ctrl Pts',(-0.0112424275638582,-0.0318829523062364,
-0.0123080342907011));
#26712=CARTESIAN_POINT('Ctrl Pts',(-0.0112378240035466,-0.0318857263341117,
-0.0122642359356089));
#26713=CARTESIAN_POINT('Ctrl Pts',(-0.0112355140795679,-0.031888500361987,
-0.0122202264115989));
#26714=CARTESIAN_POINT('Ctrl Pts',(-0.0112355000642364,-0.0318912743898623,
-0.012176256342229));
#26715=CARTESIAN_POINT('Ctrl Pts',(-0.0112354088224881,-0.031909333695321,
-0.0118900051041403));
#26716=CARTESIAN_POINT('Ctrl Pts',(-0.0113367706805386,-0.0319273930007799,
-0.011603084706141));
#26717=CARTESIAN_POINT('Ctrl Pts',(-0.0115171710811969,-0.0319454523062386,
-0.0113802355602822));
#26718=CARTESIAN_POINT('Ctrl Pts',(-0.0115448817670342,-0.0319482263341132,
-0.0113460044685137));
#26719=CARTESIAN_POINT('Ctrl Pts',(-0.0115743642075006,-0.0319510003619877,
-0.0113132454868955));
#26720=CARTESIAN_POINT('Ctrl Pts',(-0.0116054428725726,-0.0319537743898623,
-0.0112821375623097));
#26721=CARTESIAN_POINT('Ctrl Pts',(-0.0118078073461992,-0.0319718370926638,
-0.0110795825693637));
#26722=CARTESIAN_POINT('Ctrl Pts',(-0.0120824111931275,-0.0319898997954653,
-0.010948330687204));
#26723=CARTESIAN_POINT('Ctrl Pts',(-0.0123675958891875,-0.0320079624982668,
-0.0109183043207361));
#26724=CARTESIAN_POINT('Ctrl Pts',(-0.0124113402520771,-0.0320107331287986,
-0.0109136985887695));
#26725=CARTESIAN_POINT('Ctrl Pts',(-0.0124552958852648,-0.0320135037593305,
-0.0109113808600401));
#26726=CARTESIAN_POINT('Ctrl Pts',(-0.0124992131318974,-0.0320162743898623,
-0.0109113535313827));
#26727=CARTESIAN_POINT('Ctrl Pts',(-0.0127844699867276,-0.0320342705397125,
-0.0109111760228311));
#26728=CARTESIAN_POINT('Ctrl Pts',(-0.0130705179832772,-0.0320522666895627,
-0.0110117798761921));
#26729=CARTESIAN_POINT('Ctrl Pts',(-0.0132930152789238,-0.0320702628394128,
-0.0111909233309809));
#26730=CARTESIAN_POINT('Ctrl Pts',(-0.0133280930959852,-0.032073100022896,
-0.011219166197109));
#26731=CARTESIAN_POINT('Ctrl Pts',(-0.0133616331609475,-0.0320759372063791,
-0.0112492631415283));
#26732=CARTESIAN_POINT('Ctrl Pts',(-0.0133934441590142,-0.0320787743898623,
-0.0112810249316635));
#26733=CARTESIAN_POINT('Ctrl Pts',(-0.0135990067022201,-0.0320971082582658,
-0.0114862694934108));
#26734=CARTESIAN_POINT('Ctrl Pts',(-0.0137310878026323,-0.0321154421266692,
-0.0117655938573517));
#26735=CARTESIAN_POINT('Ctrl Pts',(-0.0137587787741663,-0.0321337759950726,
-0.012055702349365));
#26736=CARTESIAN_POINT('Ctrl Pts',(-0.0137625538973809,-0.0321362754600025,
-0.0120952529769626));
#26737=CARTESIAN_POINT('Ctrl Pts',(-0.0137644626950543,-0.0321387749249324,
-0.012134973360974));
#26738=CARTESIAN_POINT('Ctrl Pts',(-0.013764499458089,-0.0321412743898623,
-0.0121746826060963));
#26739=CARTESIAN_POINT('Origin',(-0.0125,-0.0412787743898723,-0.0121758532865581));
#26740=CARTESIAN_POINT('',(-0.0137644999963171,-0.0326412702050577,-0.012175922879839));
#26741=CARTESIAN_POINT('',(-0.013764499952579,-0.0325787109363731,-0.0121759694420946));
#26742=CARTESIAN_POINT('',(-0.0137645,-0.0412787743898723,-0.0121758532865581));
#26743=CARTESIAN_POINT('Ctrl Pts',(-0.0137644999999542,-0.0325787043142338,
-0.012175864048403));
#26744=CARTESIAN_POINT('Ctrl Pts',(-0.0137645024788849,-0.0325603935516432,
-0.0118845935557882));
#26745=CARTESIAN_POINT('Ctrl Pts',(-0.0136596522608517,-0.0325420806179084,
-0.0115938333359118));
#26746=CARTESIAN_POINT('Ctrl Pts',(-0.013448947159338,-0.0325212608798433,
-0.0113391718965068));
#26747=CARTESIAN_POINT('Ctrl Pts',(-0.0134222101122967,-0.0325187599996857,
-0.0113097925285742));
#26748=CARTESIAN_POINT('Ctrl Pts',(-0.0131925610498707,-0.0324982758277494,
-0.0110801256275606));
#26749=CARTESIAN_POINT('Ctrl Pts',(-0.0129191339088165,-0.0324802863335813,
-0.0109490955450475));
#26750=CARTESIAN_POINT('Ctrl Pts',(-0.012590183010145,-0.0324594626929304,
-0.0109137671230538));
#26751=CARTESIAN_POINT('Ctrl Pts',(-0.0125451129513083,-0.0324566240194546,
-0.0109113564037182));
#26752=CARTESIAN_POINT('Ctrl Pts',(-0.0122137837892425,-0.0324357362376009,
-0.0109113334877237));
#26753=CARTESIAN_POINT('Ctrl Pts',(-0.0119268474756361,-0.0324176933911951,
-0.0110128022239468));
#26754=CARTESIAN_POINT('Ctrl Pts',(-0.0116698041003138,-0.0323968396734784,
-0.0112210365037981));
#26755=CARTESIAN_POINT('Ctrl Pts',(-0.0116370522931408,-0.0323940622327908,
-0.011250534140304));
#26756=CARTESIAN_POINT('Ctrl Pts',(-0.0114035049818775,-0.0323731976062524,
-0.0114840349847706));
#26757=CARTESIAN_POINT('Ctrl Pts',(-0.0112723614861413,-0.0323550709023229,
-0.0117586372462776));
#26758=CARTESIAN_POINT('Ctrl Pts',(-0.01123781175723,-0.0323342853331126,
-0.0120876245901732));
#26759=CARTESIAN_POINT('Ctrl Pts',(-0.0112355057241986,-0.0323315180760419,
-0.012131676815311));
#26760=CARTESIAN_POINT('Ctrl Pts',(-0.0112354628440165,-0.032310773620894,
-0.012461989545241));
#26761=CARTESIAN_POINT('Ctrl Pts',(-0.0113369123537346,-0.0322929275911575,
-0.0127489399162024));
#26762=CARTESIAN_POINT('Ctrl Pts',(-0.0115451460559283,-0.0322722716324522,
-0.013006006497036));
#26763=CARTESIAN_POINT('Ctrl Pts',(-0.0115746430676899,-0.0322695200073974,
-0.0130387605517719));
#26764=CARTESIAN_POINT('Ctrl Pts',(-0.0118081008913406,-0.0322488442021525,
-0.0132722847039332));
#26765=CARTESIAN_POINT('Ctrl Pts',(-0.0120826511136037,-0.0322308326812266,
-0.0134034390928158));
#26766=CARTESIAN_POINT('Ctrl Pts',(-0.0124116737763742,-0.0322100048075982,
-0.013438037243111));
#26767=CARTESIAN_POINT('Ctrl Pts',(-0.0124557985794072,-0.0322072241920666,
-0.0134403492115628));
#26768=CARTESIAN_POINT('Ctrl Pts',(-0.0127851468318433,-0.0321864457028237,
-0.013440379614818));
#26769=CARTESIAN_POINT('Ctrl Pts',(-0.0130711473210704,-0.0321684202301248,
-0.013339619647662));
#26770=CARTESIAN_POINT('Ctrl Pts',(-0.0133286756983239,-0.0321474987910244,
-0.0131320394832236));
#26771=CARTESIAN_POINT('Ctrl Pts',(-0.0133622552364703,-0.0321446443052363,
-0.0131018683857812));
#26772=CARTESIAN_POINT('Ctrl Pts',(-0.0135995104230382,-0.0321233679731723,
-0.0128646334078737));
#26773=CARTESIAN_POINT('Ctrl Pts',(-0.0137313874371309,-0.0321049007542866,
-0.012585212686444));
#26774=CARTESIAN_POINT('Ctrl Pts',(-0.0137626205171119,-0.0320838633766418,
-0.0122554456853946));
#26775=CARTESIAN_POINT('Ctrl Pts',(-0.0137645002838139,-0.0320813339055445,
-0.0122156385036423));
#26776=CARTESIAN_POINT('Ctrl Pts',(-0.0137644999999678,-0.0320788036733635,
-0.0121758442670768));
#26777=CARTESIAN_POINT('Ctrl Pts',(-0.0137644999999896,-0.0321413477523234,
-0.012175848146052));
#26778=CARTESIAN_POINT('Ctrl Pts',(-0.0137645011763883,-0.0321595625621079,
-0.012465227487546));
#26779=CARTESIAN_POINT('Ctrl Pts',(-0.013663043056052,-0.0321767871020658,
-0.0127350696305296));
#26780=CARTESIAN_POINT('Ctrl Pts',(-0.0135072112013381,-0.0321930214076091,
-0.012940370026662));
#26781=CARTESIAN_POINT('Ctrl Pts',(-0.013496896303629,-0.0321940959966356,
-0.012953959370058));
#26782=CARTESIAN_POINT('Ctrl Pts',(-0.0134863491201398,-0.0321951662470044,
-0.0129672835872208));
#26783=CARTESIAN_POINT('Ctrl Pts',(-0.0134755850392324,-0.0321962321587258,
-0.0129803370223949));
#26784=CARTESIAN_POINT('Ctrl Pts',(-0.0133022030885797,-0.0322134012839923,
-0.0131905946442644));
#26785=CARTESIAN_POINT('Ctrl Pts',(-0.0130732963736853,-0.0322294447466978,
-0.0133276013131048));
#26786=CARTESIAN_POINT('Ctrl Pts',(-0.0128451691284769,-0.0322443624180834,
-0.0133923312036394));
#26787=CARTESIAN_POINT('Ctrl Pts',(-0.0126170418832684,-0.0322592800894691,
-0.013457061094174));
#26788=CARTESIAN_POINT('Ctrl Pts',(-0.0123906040206081,-0.0322730719695349,
-0.0134516000849701));
#26789=CARTESIAN_POINT('Ctrl Pts',(-0.0121952022194095,-0.0322857385303962,
-0.0134030690634071));
#26790=CARTESIAN_POINT('Ctrl Pts',(-0.0119998004182109,-0.0322984050912574,
-0.0133545380418441));
#26791=CARTESIAN_POINT('Ctrl Pts',(-0.0118352558919743,-0.0323099463329141,
-0.0132641994845881));
#26792=CARTESIAN_POINT('Ctrl Pts',(-0.0117063400195007,-0.0323203604956642,
-0.0131602638133983));
#26793=CARTESIAN_POINT('Ctrl Pts',(-0.0115774241470271,-0.0323307746584143,
-0.0130563281422085));
#26794=CARTESIAN_POINT('Ctrl Pts',(-0.011483731425446,-0.032340061742258,
-0.0129394138527007));
#26795=CARTESIAN_POINT('Ctrl Pts',(-0.0114167366022701,-0.0323482283138874,
-0.0128281574036222));
#26796=CARTESIAN_POINT('Ctrl Pts',(-0.0113497417790943,-0.0323563948855168,
-0.0127169009545437));
#26797=CARTESIAN_POINT('Ctrl Pts',(-0.0113092033223697,-0.032363440944932,
-0.01261149502709));
#26798=CARTESIAN_POINT('Ctrl Pts',(-0.0112835578380688,-0.0323693419850658,
-0.0125211484018958));
#26799=CARTESIAN_POINT('Ctrl Pts',(-0.0112707350959183,-0.0323722925051327,
-0.0124759750892987));
#26800=CARTESIAN_POINT('Ctrl Pts',(-0.0112616568978935,-0.0323749567703793,
-0.0124345685527524));
#26801=CARTESIAN_POINT('Ctrl Pts',(-0.0112549627958923,-0.0323773660155132,
-0.0123968569299392));
#26802=CARTESIAN_POINT('Ctrl Pts',(-0.0112482686938912,-0.0323797752606472,
-0.012359145307126));
#26803=CARTESIAN_POINT('Ctrl Pts',(-0.0112440228544091,-0.0323819294856686,
-0.0123251081982629));
#26804=CARTESIAN_POINT('Ctrl Pts',(-0.0112413201089934,-0.0323837015091994,
-0.0122970357191774));
#26805=CARTESIAN_POINT('Ctrl Pts',(-0.0112386173635777,-0.0323854735327302,
-0.012268963240092));
#26806=CARTESIAN_POINT('Ctrl Pts',(-0.0112372750835179,-0.0323868633547704,
-0.0122468834046135));
#26807=CARTESIAN_POINT('Ctrl Pts',(-0.0112363886520364,-0.0323883484661244,
-0.0122232517179404));
#26808=CARTESIAN_POINT('Ctrl Pts',(-0.0112359454362956,-0.0323890910218015,
-0.0122114358746039));
#26809=CARTESIAN_POINT('Ctrl Pts',(-0.0112357127140258,-0.0323898573998069,
-0.0121992251218495));
#26810=CARTESIAN_POINT('Ctrl Pts',(-0.0112356659453741,-0.0323900387433015,
-0.0121963386060175));
#26811=CARTESIAN_POINT('Ctrl Pts',(-0.0112356542532112,-0.0323900840791751,
-0.0121956169770595));
#26812=CARTESIAN_POINT('Ctrl Pts',(-0.0112356522835067,-0.0323900928503918,
-0.0121954780672));
#26813=CARTESIAN_POINT('Ctrl Pts',(-0.0112356496095871,-0.0323901037947021,
-0.0121953042572958));
#26814=CARTESIAN_POINT('Ctrl Pts',(-0.0112356415878281,-0.0323901366276331,
-0.0121947828275831));
#26815=CARTESIAN_POINT('Ctrl Pts',(-0.0112355037950207,-0.0323901890184068,
-0.0121939554867409));
#26816=CARTESIAN_POINT('Ctrl Pts',(-0.0112355000282024,-0.0323913068862882,
-0.0121761203516306));
#26817=CARTESIAN_POINT('Ctrl Pts',(-0.0112354950057779,-0.0323927973767968,
-0.0121523401714834));
#26818=CARTESIAN_POINT('Ctrl Pts',(-0.0112370398539334,-0.0323961820488304,
-0.0120982736572059));
#26819=CARTESIAN_POINT('Ctrl Pts',(-0.0112415429565992,-0.0323990751630377,
-0.0120523781072101));
#26820=CARTESIAN_POINT('Ctrl Pts',(-0.0112460460592651,-0.0324019682772451,
-0.0120064825572144));
#26821=CARTESIAN_POINT('Ctrl Pts',(-0.0112519691979474,-0.0324043698336261,
-0.0119685882970341));
#26822=CARTESIAN_POINT('Ctrl Pts',(-0.0112597084231613,-0.0324068590142232,
-0.0119296073639056));
#26823=CARTESIAN_POINT('Ctrl Pts',(-0.0112751868735891,-0.0324118373754174,
-0.0118516454976486));
#26824=CARTESIAN_POINT('Ctrl Pts',(-0.0112995326251591,-0.0324171662334758,
-0.011769813820212));
#26825=CARTESIAN_POINT('Ctrl Pts',(-0.0113315921296918,-0.0324224324680165,
-0.0116923418610448));
#26826=CARTESIAN_POINT('Ctrl Pts',(-0.0113957111387573,-0.0324329649370979,
-0.0115373979427105));
#26827=CARTESIAN_POINT('Ctrl Pts',(-0.0114889334793173,-0.0324432469121083,
-0.0113987138484009));
#26828=CARTESIAN_POINT('Ctrl Pts',(-0.0116056067900746,-0.0324536023812925,
-0.011281973520572));
#26829=CARTESIAN_POINT('Ctrl Pts',(-0.0117222801008318,-0.0324639578504768,
-0.0111652331927431));
#26830=CARTESIAN_POINT('Ctrl Pts',(-0.0118627766610855,-0.0324743868138348,
-0.0110711577771328));
#26831=CARTESIAN_POINT('Ctrl Pts',(-0.012015817714252,-0.0324848029688212,
-0.0110077232577651));
#26832=CARTESIAN_POINT('Ctrl Pts',(-0.0121688587674185,-0.0324952191238075,
-0.0109442887383975));
#26833=CARTESIAN_POINT('Ctrl Pts',(-0.0123343565668412,-0.0325056224704221,
-0.010911384850466));
#26834=CARTESIAN_POINT('Ctrl Pts',(-0.0124997588698091,-0.0325160342306024,
-0.0109113533095489));
#26835=CARTESIAN_POINT('Ctrl Pts',(-0.0127867621774742,-0.0325341005425989,
-0.0109112985802775));
#26836=CARTESIAN_POINT('Ctrl Pts',(-0.0130739461331377,-0.0325521921866719,
-0.0110131918049057));
#26837=CARTESIAN_POINT('Ctrl Pts',(-0.0132966463397878,-0.0325702980756418,
-0.0111938579406919));
#26838=CARTESIAN_POINT('Ctrl Pts',(-0.0133306339556649,-0.0325730613240854,
-0.0112214304845951));
#26839=CARTESIAN_POINT('Ctrl Pts',(-0.0133631604934758,-0.0325758249043161,
-0.0112507465619568));
#26840=CARTESIAN_POINT('Ctrl Pts',(-0.0133940522332139,-0.0325785887769225,
-0.0112816324780967));
#26841=CARTESIAN_POINT('Ctrl Pts',(-0.0135978692208023,-0.032596824207931,
-0.0114854110428495));
#26842=CARTESIAN_POINT('Ctrl Pts',(-0.0137295669170478,-0.0326150723662705,
-0.0117624467162534));
#26843=CARTESIAN_POINT('Ctrl Pts',(-0.0137582680854385,-0.0326333370250046,
-0.0120504671821971));
#26844=CARTESIAN_POINT('Ctrl Pts',(-0.013762420756471,-0.0326359796741892,
-0.012092139849644));
#26845=CARTESIAN_POINT('Ctrl Pts',(-0.0137645000903062,-0.0326386226687959,
-0.0121340072957658));
#26846=CARTESIAN_POINT('Ctrl Pts',(-0.0137644999999971,-0.032641266020253,
-0.0121758560153365));
#26847=CARTESIAN_POINT('Origin',(-0.0125,-0.0412787743898723,-0.0121758532865581));
#26848=CARTESIAN_POINT('',(-0.0137644997766436,-0.0331412349785624,-0.012176354624468));
#26849=CARTESIAN_POINT('',(-0.0137644999997312,-0.0330787743898623,-0.0121758793595363));
#26850=CARTESIAN_POINT('',(-0.0137645,-0.0412787743898723,-0.0121758532865581));
#26851=CARTESIAN_POINT('Ctrl Pts',(-0.0137644999999999,-0.0330787727022437,
-0.0121758527106564));
#26852=CARTESIAN_POINT('Ctrl Pts',(-0.0137644998673437,-0.0330604398739191,
-0.0118845811735839));
#26853=CARTESIAN_POINT('Ctrl Pts',(-0.0136596463479785,-0.0330421070455945,
-0.0115938210656056));
#26854=CARTESIAN_POINT('Ctrl Pts',(-0.0134742469976217,-0.0330237742172699,
-0.0113697496718626));
#26855=CARTESIAN_POINT('Ctrl Pts',(-0.0134489601755792,-0.0330212737825786,
-0.0113391883271358));
#26856=CARTESIAN_POINT('Ctrl Pts',(-0.0134222477406572,-0.0330187733478873,
-0.0113098342031574));
#26857=CARTESIAN_POINT('Ctrl Pts',(-0.0133942356918425,-0.033016272913196,
-0.0112818159397795));
#26858=CARTESIAN_POINT('Ctrl Pts',(-0.0131926389430079,-0.032998277817308,
-0.0110801744660571));
#26859=CARTESIAN_POINT('Ctrl Pts',(-0.0129192198486113,-0.03298028272142,
-0.010949124685627));
#26860=CARTESIAN_POINT('Ctrl Pts',(-0.0126351144353285,-0.032962287625532,
-0.0109185926376209));
#26861=CARTESIAN_POINT('Ctrl Pts',(-0.012590305635762,-0.0329594494584041,
-0.0109137771559177));
#26862=CARTESIAN_POINT('Ctrl Pts',(-0.0125452712982326,-0.0329566112912762,
-0.0109113633184062));
#26863=CARTESIAN_POINT('Ctrl Pts',(-0.0125002810781795,-0.0329537731241484,
-0.0109113533177977));
#26864=CARTESIAN_POINT('Ctrl Pts',(-0.0122139703982751,-0.0329357114752144,
-0.010911289675499));
#26865=CARTESIAN_POINT('Ctrl Pts',(-0.0119270124904289,-0.0329176498262805,
-0.0110127191898094));
#26866=CARTESIAN_POINT('Ctrl Pts',(-0.0117041637398992,-0.0328995881773465,
-0.01119320131505));
#26867=CARTESIAN_POINT('Ctrl Pts',(-0.0116699669322119,-0.0328968165632646,
-0.0112208968372963));
#26868=CARTESIAN_POINT('Ctrl Pts',(-0.0116372401521535,-0.0328940449491827,
-0.0112503609161892));
#26869=CARTESIAN_POINT('Ctrl Pts',(-0.0116061618569985,-0.0328912733351008,
-0.0112814184794784));
#26870=CARTESIAN_POINT('Ctrl Pts',(-0.0114036734472617,-0.0328732150817423,
-0.0114837718122265));
#26871=CARTESIAN_POINT('Ctrl Pts',(-0.0112724678069508,-0.0328551568283838,
-0.0117583324226996));
#26872=CARTESIAN_POINT('Ctrl Pts',(-0.0112424499134969,-0.0328370985750254,
-0.0120434598201938));
#26873=CARTESIAN_POINT('Ctrl Pts',(-0.0112378370673606,-0.0328343235653679,
-0.0120872753136389));
#26874=CARTESIAN_POINT('Ctrl Pts',(-0.0112355197009196,-0.0328315485557105,
-0.0121313025356128));
#26875=CARTESIAN_POINT('Ctrl Pts',(-0.0112355001252145,-0.032828773546053,
-0.0121752905543113));
#26876=CARTESIAN_POINT('Ctrl Pts',(-0.0112353727371744,-0.0328107152926946,
-0.0124615406523085));
#26877=CARTESIAN_POINT('Ctrl Pts',(-0.0113366976187793,-0.0327926570393361,
-0.0127484730157758));
#26878=CARTESIAN_POINT('Ctrl Pts',(-0.0115170688076744,-0.0327745987859777,
-0.0129713446574436));
#26879=CARTESIAN_POINT('Ctrl Pts',(-0.0115447864269355,-0.0327718237763202,
-0.0130055933162549));
#26880=CARTESIAN_POINT('Ctrl Pts',(-0.0115742774409676,-0.0327690487666628,
-0.0130383688860161));
#26881=CARTESIAN_POINT('Ctrl Pts',(-0.0116053661220587,-0.0327662737570053,
-0.0130694921814366));
#26882=CARTESIAN_POINT('Ctrl Pts',(-0.0118077123885585,-0.0327482121080714,
-0.0132720637415188));
#26883=CARTESIAN_POINT('Ctrl Pts',(-0.0120823038219357,-0.0327301504591375,
-0.0134033391389739));
#26884=CARTESIAN_POINT('Ctrl Pts',(-0.0123674849516029,-0.0327120888102036,
-0.0134333905670982));
#26885=CARTESIAN_POINT('Ctrl Pts',(-0.0124112468494109,-0.0327093171961216,
-0.0134380020486787));
#26886=CARTESIAN_POINT('Ctrl Pts',(-0.0124552203917516,-0.0327065455820396,
-0.0134403236663119));
#26887=CARTESIAN_POINT('Ctrl Pts',(-0.0124991556137138,-0.0327037739679577,
-0.0134403530046331));
#26888=CARTESIAN_POINT('Ctrl Pts',(-0.0127844112476858,-0.0326857788720697,
-0.0134405434878273));
#26889=CARTESIAN_POINT('Ctrl Pts',(-0.0130704629193013,-0.0326677837761816,
-0.0133399534447622));
#26890=CARTESIAN_POINT('Ctrl Pts',(-0.0132929680502495,-0.0326497886802936,
-0.0131608212663846));
#26891=CARTESIAN_POINT('Ctrl Pts',(-0.0133280613196807,-0.0326469505131657,
-0.0131325687322843));
#26892=CARTESIAN_POINT('Ctrl Pts',(-0.0133616156871987,-0.0326441123460379,
-0.0131024605546831));
#26893=CARTESIAN_POINT('Ctrl Pts',(-0.0133934396024196,-0.03264127417891,
-0.0130706861909757));
#26894=CARTESIAN_POINT('Ctrl Pts',(-0.0135990026817153,-0.0326229413505854,
-0.0128654431842294));
#26895=CARTESIAN_POINT('Ctrl Pts',(-0.0137310852050748,-0.0326046085222609,
-0.0125861201701978));
#26896=CARTESIAN_POINT('Ctrl Pts',(-0.0137587780000869,-0.0325862756939363,
-0.0122960123332303));
#26897=CARTESIAN_POINT('Ctrl Pts',(-0.0137625550509665,-0.032583775259245,
-0.0122564442051196));
#26898=CARTESIAN_POINT('Ctrl Pts',(-0.013764464121777,-0.0325812748245536,
-0.0122167061575427));
#26899=CARTESIAN_POINT('Ctrl Pts',(-0.0137644994986291,-0.0325787743898623,
-0.0121769793268418));
#26900=CARTESIAN_POINT('Ctrl Pts',(-0.0137644999926371,-0.0326412743898623,
-0.0121759897443414));
#26901=CARTESIAN_POINT('Ctrl Pts',(-0.0137644685603842,-0.0326596023068526,
-0.0124672599279237));
#26902=CARTESIAN_POINT('Ctrl Pts',(-0.0136595846977029,-0.032677930223843,
-0.0127580076853526));
#26903=CARTESIAN_POINT('Ctrl Pts',(-0.0134741627452126,-0.0326962581408333,
-0.0129820587168547));
#26904=CARTESIAN_POINT('Ctrl Pts',(-0.0134488456013029,-0.0326987605980978,
-0.0130126501982381));
#26905=CARTESIAN_POINT('Ctrl Pts',(-0.0134220999108933,-0.0327012630553624,
-0.0130420317130972));
#26906=CARTESIAN_POINT('Ctrl Pts',(-0.0133940521006994,-0.0327037655126269,
-0.0130700742275089));
#26907=CARTESIAN_POINT('Ctrl Pts',(-0.0131924160601591,-0.0327217557076172,
-0.0132716721966082));
#26908=CARTESIAN_POINT('Ctrl Pts',(-0.0129189730052593,-0.0327397459026075,
-0.0134026656693521));
#26909=CARTESIAN_POINT('Ctrl Pts',(-0.0126348638437601,-0.0327577360975978,
-0.0134331408406388));
#26910=CARTESIAN_POINT('Ctrl Pts',(-0.0125900104694752,-0.0327605762768623,
-0.0134379520697344));
#26911=CARTESIAN_POINT('Ctrl Pts',(-0.0125449315998565,-0.0327634164561269,
-0.0134403569263869));
#26912=CARTESIAN_POINT('Ctrl Pts',(-0.0124998976816101,-0.0327662566353914,
-0.0134403532824185));
#26913=CARTESIAN_POINT('Ctrl Pts',(-0.0122135897910585,-0.0327843133749709,
-0.0134403301155047));
#26914=CARTESIAN_POINT('Ctrl Pts',(-0.0119266647188268,-0.0328023701145505,
-0.0133388154499535));
#26915=CARTESIAN_POINT('Ctrl Pts',(-0.0117038714045645,-0.03282042685413,
-0.0131582684276924));
#26916=CARTESIAN_POINT('Ctrl Pts',(-0.0116696488773386,-0.0328232004888053,
-0.0131305352104486));
#26917=CARTESIAN_POINT('Ctrl Pts',(-0.0116368998322642,-0.0328259741234807,
-0.0131010303575405));
#26918=CARTESIAN_POINT('Ctrl Pts',(-0.0116058031972925,-0.032828747758156,
-0.0130699295294075));
#26919=CARTESIAN_POINT('Ctrl Pts',(-0.0114033978839815,-0.032846801106886,
-0.0128674969231715));
#26920=CARTESIAN_POINT('Ctrl Pts',(-0.0112723025246776,-0.0328648544556159,
-0.0125928864066233));
#26921=CARTESIAN_POINT('Ctrl Pts',(-0.0112423976430418,-0.0328829078043458,
-0.012307749312932));
#26922=CARTESIAN_POINT('Ctrl Pts',(-0.0112377975757155,-0.0328856848298707,
-0.0122638885866408));
#26923=CARTESIAN_POINT('Ctrl Pts',(-0.0112354976277577,-0.0328884618553957,
-0.012219816624342));
#26924=CARTESIAN_POINT('Ctrl Pts',(-0.011235500001838,-0.0328912388809206,
-0.0121757851075616));
#26925=CARTESIAN_POINT('Ctrl Pts',(-0.011235515435654,-0.0329092922296505,
-0.0118895377106938));
#26926=CARTESIAN_POINT('Ctrl Pts',(-0.0113369816624679,-0.0329273455783804,
-0.011602657952783));
#26927=CARTESIAN_POINT('Ctrl Pts',(-0.0115174614365488,-0.0329453989271104,
-0.0113798770172314));
#26928=CARTESIAN_POINT('Ctrl Pts',(-0.011545223429454,-0.0329481759526353,
-0.0113456081204329));
#26929=CARTESIAN_POINT('Ctrl Pts',(-0.0115747616064416,-0.0329509529781602,
-0.0113128161149497));
#26930=CARTESIAN_POINT('Ctrl Pts',(-0.0116058996156524,-0.0329537300036851,
-0.0112816806227456));
#26931=CARTESIAN_POINT('Ctrl Pts',(-0.0118083647778547,-0.0329717867432646,
-0.0110792318265923));
#26932=CARTESIAN_POINT('Ctrl Pts',(-0.0120830317457008,-0.0329898434828442,
-0.0109481204941999));
#26933=CARTESIAN_POINT('Ctrl Pts',(-0.0123682283698876,-0.0330079002224237,
-0.0109182378892694));
#26934=CARTESIAN_POINT('Ctrl Pts',(-0.0124120364584216,-0.033010673857099,
-0.010913647723428));
#26935=CARTESIAN_POINT('Ctrl Pts',(-0.0124560552530744,-0.0330134474917744,
-0.010911352103133));
#26936=CARTESIAN_POINT('Ctrl Pts',(-0.012500034039603,-0.0330162211264497,
-0.0109113532870163));
#26937=CARTESIAN_POINT('Ctrl Pts',(-0.0127852867991391,-0.03303421132144,
-0.0109113609658543));
#26938=CARTESIAN_POINT('Ctrl Pts',(-0.0130712663423404,-0.0330522015164303,
-0.0110121477627849));
#26939=CARTESIAN_POINT('Ctrl Pts',(-0.0132936462228542,-0.0330701917114207,
-0.0111914316680687));
#26940=CARTESIAN_POINT('Ctrl Pts',(-0.013328754165032,-0.0330730318906852,
-0.0112197358877021));
#26941=CARTESIAN_POINT('Ctrl Pts',(-0.0133623189218372,-0.0330758720699498,
-0.0112498983046016));
#26942=CARTESIAN_POINT('Ctrl Pts',(-0.0133941485242657,-0.0330787122492143,
-0.011281728761364));
#26943=CARTESIAN_POINT('Ctrl Pts',(-0.0135995476405913,-0.0330970401662046,
-0.0114871333907787));
#26944=CARTESIAN_POINT('Ctrl Pts',(-0.0137314087469587,-0.0331153680831949,
-0.0117665593582989));
#26945=CARTESIAN_POINT('Ctrl Pts',(-0.0137588724472994,-0.0331336960001852,
-0.0120566878073691));
#26946=CARTESIAN_POINT('Ctrl Pts',(-0.0137626222862181,-0.0331361984574497,
-0.0120963013676778));
#26947=CARTESIAN_POINT('Ctrl Pts',(-0.0137644999968615,-0.0331387009147143,
-0.0121360837360722));
#26948=CARTESIAN_POINT('Ctrl Pts',(-0.0137645,-0.0331412033719788,-0.0121758531867676));
#26949=CARTESIAN_POINT('Origin',(-0.0125,-0.0412787743898723,-0.0121758532865581));
#26950=CARTESIAN_POINT('',(-0.0137644017347287,-0.0336414716603326,-0.012175630710863));
#26951=CARTESIAN_POINT('',(-0.0137644996589709,-0.0335787980895467,-0.0121750921833385));
#26952=CARTESIAN_POINT('',(-0.0137645,-0.0412787743898723,-0.0121758532865581));
#26953=CARTESIAN_POINT('Ctrl Pts',(-0.0137644994877345,-0.0335787743898623,
-0.0121747150778228));
#26954=CARTESIAN_POINT('Ctrl Pts',(-0.0137642373067409,-0.0335604414094987,
-0.0118834436073164));
#26955=CARTESIAN_POINT('Ctrl Pts',(-0.0136591222073282,-0.033542108429135,
-0.0115927779094656));
#26956=CARTESIAN_POINT('Ctrl Pts',(-0.013473521285526,-0.0335237754487713,
-0.0113688733880304));
#26957=CARTESIAN_POINT('Ctrl Pts',(-0.0134482080082087,-0.0335212750958016,
-0.0113383360545481));
#26958=CARTESIAN_POINT('Ctrl Pts',(-0.0134214703210877,-0.033518774742832,
-0.0113090071252378));
#26959=CARTESIAN_POINT('Ctrl Pts',(-0.0133934343230916,-0.0335162743898623,
-0.0112810151110639));
#26960=CARTESIAN_POINT('Ctrl Pts',(-0.0131916569149418,-0.0334982791416907,
-0.0110795542581383));
#26961=CARTESIAN_POINT('Ctrl Pts',(-0.0129181204047335,-0.0334802838935192,
-0.0109487494930919));
#26962=CARTESIAN_POINT('Ctrl Pts',(-0.0126339876547543,-0.0334622886453476,
-0.0109184720562332));
#26963=CARTESIAN_POINT('Ctrl Pts',(-0.0125891762170904,-0.0334594505601858,
-0.0109136969098464));
#26964=CARTESIAN_POINT('Ctrl Pts',(-0.0125441414103058,-0.0334566124750241,
-0.0109113234307162));
#26965=CARTESIAN_POINT('Ctrl Pts',(-0.0124991528616412,-0.0334537743898623,
-0.0109113535703238));
#26966=CARTESIAN_POINT('Ctrl Pts',(-0.0122128421325712,-0.0334357125884496,
-0.0109115453812021));
#26967=CARTESIAN_POINT('Ctrl Pts',(-0.0119259747580602,-0.0334176507870369,
-0.0110132309561064));
#26968=CARTESIAN_POINT('Ctrl Pts',(-0.011703287099886,-0.0333995889856242,
-0.0111939119416744));
#26969=CARTESIAN_POINT('Ctrl Pts',(-0.0116691163137691,-0.0333968174537036,
-0.0112216369236687));
#26970=CARTESIAN_POINT('Ctrl Pts',(-0.0116364170215967,-0.0333940459217829,
-0.0112511290160514));
#26971=CARTESIAN_POINT('Ctrl Pts',(-0.0116053675044745,-0.0333912743898623,
-0.0112822130077267));
#26972=CARTESIAN_POINT('Ctrl Pts',(-0.0114030588925162,-0.0333732159841984,
-0.0114847462447237));
#26973=CARTESIAN_POINT('Ctrl Pts',(-0.0112720972453575,-0.0333551575785346,
-0.0117594234255462));
#26974=CARTESIAN_POINT('Ctrl Pts',(-0.011242332750728,-0.0333370991728707,
-0.0120445774696354));
#26975=CARTESIAN_POINT('Ctrl Pts',(-0.0112377590180712,-0.0333343242452012,
-0.0120883953936389));
#26976=CARTESIAN_POINT('Ctrl Pts',(-0.0112354807791195,-0.0333315493175318,
-0.0121324229903591));
#26977=CARTESIAN_POINT('Ctrl Pts',(-0.0112355001222663,-0.0333287743898623,
-0.0121764093544956));
#26978=CARTESIAN_POINT('Ctrl Pts',(-0.0112356260017247,-0.0333107159841984,
-0.0124626595569768));
#26979=CARTESIAN_POINT('Ctrl Pts',(-0.0113372047834033,-0.0332926575785346,
-0.0127495022348612));
#26980=CARTESIAN_POINT('Ctrl Pts',(-0.0115177731919476,-0.0332745991728708,
-0.0129722142270512));
#26981=CARTESIAN_POINT('Ctrl Pts',(-0.0115455200640928,-0.0332718242452013,
-0.0130064370527511));
#26982=CARTESIAN_POINT('Ctrl Pts',(-0.0115750388929873,-0.0332690493175318,
-0.0130391853319111));
#26983=CARTESIAN_POINT('Ctrl Pts',(-0.011606153812779,-0.0332662743898623,
-0.0130702800547121));
#26984=CARTESIAN_POINT('Ctrl Pts',(-0.0118086785518679,-0.0332482125884496,
-0.0132726733330642));
#26985=CARTESIAN_POINT('Ctrl Pts',(-0.0120833856444131,-0.0332301507870369,
-0.0134037067560259));
#26986=CARTESIAN_POINT('Ctrl Pts',(-0.0123685932311997,-0.0332120889856242,
-0.0134335068601281));
#26987=CARTESIAN_POINT('Ctrl Pts',(-0.0124123575220764,-0.0332093174537036,
-0.0134380796011228));
#26988=CARTESIAN_POINT('Ctrl Pts',(-0.012456331423678,-0.0332065459217829,
-0.0134403624658187));
#26989=CARTESIAN_POINT('Ctrl Pts',(-0.0125002649974867,-0.0332037743898623,
-0.0134403532587907));
#26990=CARTESIAN_POINT('Ctrl Pts',(-0.0127855208005565,-0.0331857791416907,
-0.0134402934785831));
#26991=CARTESIAN_POINT('Ctrl Pts',(-0.0130714841943955,-0.0331677838935192,
-0.0133394524388388));
#26992=CARTESIAN_POINT('Ctrl Pts',(-0.0132938321104615,-0.0331497886453476,
-0.0131601250124551));
#26993=CARTESIAN_POINT('Ctrl Pts',(-0.0133288992745993,-0.0331469505601858,
-0.0131318427402095));
#26994=CARTESIAN_POINT('Ctrl Pts',(-0.0133624260233035,-0.0331441124750241,
-0.0131017063130526));
#26995=CARTESIAN_POINT('Ctrl Pts',(-0.0133942209933907,-0.0331412743898623,
-0.0130699053348077));
#26996=CARTESIAN_POINT('Ctrl Pts',(-0.0135996047394909,-0.0331229414094986,
-0.0128644827782311));
#26997=CARTESIAN_POINT('Ctrl Pts',(-0.0137314431939203,-0.0331046084291349,
-0.0125850444201865));
#26998=CARTESIAN_POINT('Ctrl Pts',(-0.0137588825062962,-0.0330862754487713,
-0.0122949124539553));
#26999=CARTESIAN_POINT('Ctrl Pts',(-0.0137626248310478,-0.0330837750958016,
-0.0122553426563026));
#27000=CARTESIAN_POINT('Ctrl Pts',(-0.0137644991806288,-0.033081274742832,
-0.0122156045851513));
#27001=CARTESIAN_POINT('Ctrl Pts',(-0.0137644999997312,-0.0330787743898623,
-0.0121758793595363));
#27002=CARTESIAN_POINT('Ctrl Pts',(-0.013764499498133,-0.0331412743898623,
-0.0121769798838072));
#27003=CARTESIAN_POINT('Ctrl Pts',(-0.0137642399910612,-0.0331596088050655,
-0.012468252175019));
#27004=CARTESIAN_POINT('Ctrl Pts',(-0.0136591270148841,-0.0331779432202687,
-0.012758919492331));
#27005=CARTESIAN_POINT('Ctrl Pts',(-0.0134735272558264,-0.0331962776354719,
-0.0129828259826037));
#27006=CARTESIAN_POINT('Ctrl Pts',(-0.0134482306429966,-0.033198776553602,
-0.0130133436719761));
#27007=CARTESIAN_POINT('Ctrl Pts',(-0.0134215114608746,-0.0332012754717322,
-0.0130426545398078));
#27008=CARTESIAN_POINT('Ctrl Pts',(-0.0133934955569117,-0.0332037743898623,
-0.0130706303201139));
#27009=CARTESIAN_POINT('Ctrl Pts',(-0.0131917306594618,-0.0332217710949099,
-0.0132721062550693));
#27010=CARTESIAN_POINT('Ctrl Pts',(-0.0129182013201166,-0.0332397677999575,
-0.0134029298366984));
#27011=CARTESIAN_POINT('Ctrl Pts',(-0.0126340691208629,-0.0332577645050051,
-0.0134332258331134));
#27012=CARTESIAN_POINT('Ctrl Pts',(-0.0125892843988171,-0.0332606011332908,
-0.0134380010672548));
#27013=CARTESIAN_POINT('Ctrl Pts',(-0.012544276414023,-0.0332634377615766,
-0.0134403774816797));
#27014=CARTESIAN_POINT('Ctrl Pts',(-0.0124993143156266,-0.0332662743898624,
-0.0134403531006494));
#27015=CARTESIAN_POINT('Ctrl Pts',(-0.0122130018722459,-0.0332843376476823,
-0.0134401978456101));
#27016=CARTESIAN_POINT('Ctrl Pts',(-0.0119261202647265,-0.0333024009055021,
-0.0133385477790772));
#27017=CARTESIAN_POINT('Ctrl Pts',(-0.0117034091133121,-0.033320464163322,
-0.0131578936163031));
#27018=CARTESIAN_POINT('Ctrl Pts',(-0.0116692554344324,-0.0333232342388354,
-0.0131301895510847));
#27019=CARTESIAN_POINT('Ctrl Pts',(-0.0116365712576102,-0.0333260043143489,
-0.0131007203188604));
#27020=CARTESIAN_POINT('Ctrl Pts',(-0.0116055345699018,-0.0333287743898623,
-0.0130696607850493));
#27021=CARTESIAN_POINT('Ctrl Pts',(-0.0114031869384003,-0.033346834249358,
-0.0128671642054773));
#27022=CARTESIAN_POINT('Ctrl Pts',(-0.0112721738559381,-0.0333648941088535,
-0.0125925098791858));
#27023=CARTESIAN_POINT('Ctrl Pts',(-0.011242356873197,-0.0333829539683491,
-0.0123073599997148));
#27024=CARTESIAN_POINT('Ctrl Pts',(-0.0112377778441314,-0.0333857274421868,
-0.0122635691977578));
#27025=CARTESIAN_POINT('Ctrl Pts',(-0.0112354915142712,-0.0333885009160246,
-0.0122195685521193));
#27026=CARTESIAN_POINT('Ctrl Pts',(-0.0112355000236904,-0.0333912743898623,
-0.0121756085151439));
#27027=CARTESIAN_POINT('Ctrl Pts',(-0.0112355554339538,-0.0334093342493578,
-0.0118893566383836));
#27028=CARTESIAN_POINT('Ctrl Pts',(-0.0113370646897218,-0.0334273941088534,
-0.0116024877429456));
#27029=CARTESIAN_POINT('Ctrl Pts',(-0.0115175798344913,-0.0334454539683489,
-0.011379730891193));
#27030=CARTESIAN_POINT('Ctrl Pts',(-0.0115453017573263,-0.0334482274421867,
-0.0113455218597949));
#27031=CARTESIAN_POINT('Ctrl Pts',(-0.0115747938682146,-0.0334510009160245,
-0.0113127851735476));
#27032=CARTESIAN_POINT('Ctrl Pts',(-0.0116058806685998,-0.0334537743898623,
-0.0112816995686681));
#27033=CARTESIAN_POINT('Ctrl Pts',(-0.0118083447706616,-0.0334718376476825,
-0.0110792432527729));
#27034=CARTESIAN_POINT('Ctrl Pts',(-0.012083013501435,-0.0334899009055026,
-0.0109481258335134));
#27035=CARTESIAN_POINT('Ctrl Pts',(-0.0123682134196918,-0.0335079641633228,
-0.0109182394558252));
#27036=CARTESIAN_POINT('Ctrl Pts',(-0.0124119500101667,-0.033510734238836,
-0.0109136562558379));
#27037=CARTESIAN_POINT('Ctrl Pts',(-0.0124558966516803,-0.0335135043143491,
-0.0109113601123901));
#27038=CARTESIAN_POINT('Ctrl Pts',(-0.0124998038584254,-0.0335162743898623,
-0.0109113533017702));
#27039=CARTESIAN_POINT('Ctrl Pts',(-0.0127850614427392,-0.0335342710949099,
-0.0109113090543425));
#27040=CARTESIAN_POINT('Ctrl Pts',(-0.0130710629130146,-0.0335522677999575,
-0.0110120469742265));
#27041=CARTESIAN_POINT('Ctrl Pts',(-0.0132934766700397,-0.0335702645050051,
-0.0111912949977287));
#27042=CARTESIAN_POINT('Ctrl Pts',(-0.0133285333736225,-0.0335731011332908,
-0.0112195479480487));
#27043=CARTESIAN_POINT('Ctrl Pts',(-0.0133620521491485,-0.0335759377615766,
-0.0112496534229335));
#27044=CARTESIAN_POINT('Ctrl Pts',(-0.0133938418969691,-0.0335787743898624,
-0.0112814222309576));
#27045=CARTESIAN_POINT('Ctrl Pts',(-0.0135993134558177,-0.0335971088050655,
-0.0114867584464037));
#27046=CARTESIAN_POINT('Ctrl Pts',(-0.0137312703595708,-0.0336154432202687,
-0.0117661418824352));
#27047=CARTESIAN_POINT('Ctrl Pts',(-0.0137588321571824,-0.033633777635472,
-0.0120562629439565));
#27048=CARTESIAN_POINT('Ctrl Pts',(-0.0137625887359981,-0.0336362765536021,
-0.0120958054530865));
#27049=CARTESIAN_POINT('Ctrl Pts',(-0.0137644798389691,-0.0336387754717322,
-0.0121355168034981));
#27050=CARTESIAN_POINT('Ctrl Pts',(-0.0137644998395261,-0.0336412743898623,
-0.0121752162320185));
#27051=CARTESIAN_POINT('Origin',(-0.0125,-0.0412787743898723,-0.0121758532865581));
#27052=CARTESIAN_POINT('',(-0.0137644998637729,-0.0341412999856959,-0.0121754316468409));
#27053=CARTESIAN_POINT('',(-0.013764499925554,-0.0340787743898623,-0.0121762871919379));
#27054=CARTESIAN_POINT('',(-0.0137645,-0.0412787743898723,-0.0121758532865581));
#27055=CARTESIAN_POINT('Ctrl Pts',(-0.0137644999999728,-0.0340787477436506,
-0.0121758615870606));
#27056=CARTESIAN_POINT('Ctrl Pts',(-0.0137645018988856,-0.0340606084504782,
-0.0118865808727149));
#27057=CARTESIAN_POINT('Ctrl Pts',(-0.0136610153723787,-0.0340424568279764,
-0.0115976083349243));
#27058=CARTESIAN_POINT('Ctrl Pts',(-0.0134779938396196,-0.0340242900869158,
-0.011374299607965));
#27059=CARTESIAN_POINT('Ctrl Pts',(-0.0134515698526924,-0.0340216672385489,
-0.0113420591016543));
#27060=CARTESIAN_POINT('Ctrl Pts',(-0.0134235693534653,-0.0340190440750426,
-0.0113111498801886));
#27061=CARTESIAN_POINT('Ctrl Pts',(-0.0133941409267945,-0.0340164205880029,
-0.0112817211637535));
#27062=CARTESIAN_POINT('Ctrl Pts',(-0.013191714932659,-0.0339983747040669,
-0.011079293176449));
#27063=CARTESIAN_POINT('Ctrl Pts',(-0.0129168426251142,-0.0339803135121575,
-0.0109479341169463));
#27064=CARTESIAN_POINT('Ctrl Pts',(-0.0126310167083062,-0.0339622452080805,
-0.0109181590184052));
#27065=CARTESIAN_POINT('Ctrl Pts',(-0.0125874794070605,-0.033959493025191,
-0.0109136236443941));
#27066=CARTESIAN_POINT('Ctrl Pts',(-0.0125437266583471,-0.0339567406772872,
-0.0109113534300671));
#27067=CARTESIAN_POINT('Ctrl Pts',(-0.01250000415023,-0.0339539881933339,
-0.0109113532865649));
#27068=CARTESIAN_POINT('Ctrl Pts',(-0.0123346219886952,-0.0339435768110642,
-0.0109113527437622));
#27069=CARTESIAN_POINT('Ctrl Pts',(-0.0121691218361513,-0.0339331634822505,
-0.0109442230135551));
#27070=CARTESIAN_POINT('Ctrl Pts',(-0.0120160996755066,-0.0339227325313663,
-0.0110076064265344));
#27071=CARTESIAN_POINT('Ctrl Pts',(-0.0118630775148619,-0.033912301580482,
-0.0110709898395137));
#27072=CARTESIAN_POINT('Ctrl Pts',(-0.0117226409181171,-0.033901853007527,
-0.0111649397020928));
#27073=CARTESIAN_POINT('Ctrl Pts',(-0.011605864942515,-0.0338914505596433,
-0.0112817152944248));
#27074=CARTESIAN_POINT('Ctrl Pts',(-0.0114890889669128,-0.0338810481117596,
-0.0113984908867567));
#27075=CARTESIAN_POINT('Ctrl Pts',(-0.0113956972487478,-0.0338706917889472,
-0.0115375785856883));
#27076=CARTESIAN_POINT('Ctrl Pts',(-0.0113317547281944,-0.0338601422781651,
-0.0116919491277582));
#27077=CARTESIAN_POINT('Ctrl Pts',(-0.0112997834679177,-0.033854867522774,
-0.0117691343987931));
#27078=CARTESIAN_POINT('Ctrl Pts',(-0.011275473578601,-0.0338495444703905,
-0.011850350325652));
#27079=CARTESIAN_POINT('Ctrl Pts',(-0.0112597971141385,-0.0338444782712676,
-0.0119291610655605));
#27080=CARTESIAN_POINT('Ctrl Pts',(-0.0112519588819072,-0.0338419451717062,
-0.0119685664355147));
#27081=CARTESIAN_POINT('Ctrl Pts',(-0.0112459846027741,-0.0338394762854599,
-0.0120072805204668));
#27082=CARTESIAN_POINT('Ctrl Pts',(-0.0112415889385475,-0.0338366438012794,
-0.0120519103544722));
#27083=CARTESIAN_POINT('Ctrl Pts',(-0.011237193274321,-0.0338338113170988,
-0.0120965401884777));
#27084=CARTESIAN_POINT('Ctrl Pts',(-0.0112355,-0.0338306152349841,-0.0121472179637786));
#27085=CARTESIAN_POINT('Ctrl Pts',(-0.0112355,-0.0338288076869315,-0.0121758532865581));
#27086=CARTESIAN_POINT('Ctrl Pts',(-0.0112355,-0.0338270001388788,-0.0122044886093376));
#27087=CARTESIAN_POINT('Ctrl Pts',(-0.0112359205269678,-0.0338265811248883,
-0.0122111179060965));
#27088=CARTESIAN_POINT('Ctrl Pts',(-0.0112364374006413,-0.0338257345815302,
-0.0122245339552262));
#27089=CARTESIAN_POINT('Ctrl Pts',(-0.0112369542743149,-0.033824888038172,
-0.0122379500043559));
#27090=CARTESIAN_POINT('Ctrl Pts',(-0.0112380215535703,-0.0338236139654462,
-0.0122581221936209));
#27091=CARTESIAN_POINT('Ctrl Pts',(-0.0112396320697024,-0.0338223557845349,
-0.0122779950031942));
#27092=CARTESIAN_POINT('Ctrl Pts',(-0.0112428531019667,-0.0338198394227122,
-0.0123177406223408));
#27093=CARTESIAN_POINT('Ctrl Pts',(-0.0112477128926463,-0.0338173866281474,
-0.0123563628814054));
#27094=CARTESIAN_POINT('Ctrl Pts',(-0.0112552843905968,-0.0338146811157623,
-0.0123986610550672));
#27095=CARTESIAN_POINT('Ctrl Pts',(-0.0112704273864978,-0.0338092700909921,
-0.0124832574023907));
#27096=CARTESIAN_POINT('Ctrl Pts',(-0.0112971842349235,-0.0338028481949406,
-0.012582311247989));
#27097=CARTESIAN_POINT('Ctrl Pts',(-0.0113432673161325,-0.033795663479089,
-0.0126866661173217));
#27098=CARTESIAN_POINT('Ctrl Pts',(-0.0113893503973415,-0.0337884787632373,
-0.0127910209866544));
#27099=CARTESIAN_POINT('Ctrl Pts',(-0.0114546927022284,-0.0337805312275854,
-0.0129009041684455));
#27100=CARTESIAN_POINT('Ctrl Pts',(-0.0115461452173229,-0.0337717547769112,
-0.0130059865912531));
#27101=CARTESIAN_POINT('Ctrl Pts',(-0.0116375977324173,-0.033762978326237,
-0.0131110690140608));
#27102=CARTESIAN_POINT('Ctrl Pts',(-0.0117547887102928,-0.0337533729605404,
-0.0132109764039506));
#27103=CARTESIAN_POINT('Ctrl Pts',(-0.0119018449572601,-0.0337429550092292,
-0.0132899317374963));
#27104=CARTESIAN_POINT('Ctrl Pts',(-0.0120983071384933,-0.0337290369779943,
-0.0133954133975296));
#27105=CARTESIAN_POINT('Ctrl Pts',(-0.012346185450533,-0.0337136686392474,
-0.0134590161788762));
#27106=CARTESIAN_POINT('Ctrl Pts',(-0.0126119809515327,-0.0336968458212211,
-0.0134353851505829));
#27107=CARTESIAN_POINT('Ctrl Pts',(-0.0127440929622223,-0.0336884841435156,
-0.0134236394940509));
#27108=CARTESIAN_POINT('Ctrl Pts',(-0.0128798762734508,-0.0336797631329847,
-0.0133904081463402));
#27109=CARTESIAN_POINT('Ctrl Pts',(-0.0130108174784532,-0.0336706822773521,
-0.013332583917996));
#27110=CARTESIAN_POINT('Ctrl Pts',(-0.0132080080623682,-0.0336570069852651,
-0.0132455036642943));
#27111=CARTESIAN_POINT('Ctrl Pts',(-0.0133984744886159,-0.0336425156084047,
-0.0130983842065243));
#27112=CARTESIAN_POINT('Ctrl Pts',(-0.0135377000870961,-0.0336272093131572,
-0.012898444996475));
#27113=CARTESIAN_POINT('Ctrl Pts',(-0.0136769256855764,-0.0336119030179097,
-0.0126985057864257));
#27114=CARTESIAN_POINT('Ctrl Pts',(-0.013764502164571,-0.033595781804275,
-0.0124452108403644));
#27115=CARTESIAN_POINT('Ctrl Pts',(-0.0137644999999592,-0.0335788452834579,
-0.0121758431251633));
#27116=CARTESIAN_POINT('Ctrl Pts',(-0.0137644999999694,-0.0336413152440371,
-0.0121758620877456));
#27117=CARTESIAN_POINT('Ctrl Pts',(-0.0137644979726606,-0.033659645947366,
-0.0124671332318196));
#27118=CARTESIAN_POINT('Ctrl Pts',(-0.0136596428238356,-0.0336779766506949,
-0.0127578923433247));
#27119=CARTESIAN_POINT('Ctrl Pts',(-0.013474242444834,-0.0336963073540238,
-0.0129819624036657));
#27120=CARTESIAN_POINT('Ctrl Pts',(-0.0134489475642251,-0.033698808281771,
-0.0130125331363409));
#27121=CARTESIAN_POINT('Ctrl Pts',(-0.0134222261882464,-0.0337013092095181,
-0.0130418958856302));
#27122=CARTESIAN_POINT('Ctrl Pts',(-0.0133942044369489,-0.0337038101372653,
-0.0130699218940714));
#27123=CARTESIAN_POINT('Ctrl Pts',(-0.0131926012515593,-0.0337218031240314,
-0.0132715557075881));
#27124=CARTESIAN_POINT('Ctrl Pts',(-0.0129191784313342,-0.0337397961107975,
-0.0134025958817728));
#27125=CARTESIAN_POINT('Ctrl Pts',(-0.0126350726820894,-0.0337577890975637,
-0.0134331184219027));
#27126=CARTESIAN_POINT('Ctrl Pts',(-0.0125902510424699,-0.0337606277418736,
-0.0134379337777961));
#27127=CARTESIAN_POINT('Ctrl Pts',(-0.0125452038176885,-0.0337634663861835,
-0.0134403461209176));
#27128=CARTESIAN_POINT('Ctrl Pts',(-0.0125002008930168,-0.0337663050304934,
-0.0134403532706));
#27129=CARTESIAN_POINT('Ctrl Pts',(-0.0122138910223444,-0.0337843645653168,
-0.0134403987570803));
#27130=CARTESIAN_POINT('Ctrl Pts',(-0.011926940148603,-0.03380242410014,
-0.0133389515838582));
#27131=CARTESIAN_POINT('Ctrl Pts',(-0.0117041030481573,-0.0338204836349634,
-0.0131584561015589));
#27132=CARTESIAN_POINT('Ctrl Pts',(-0.0116698980757059,-0.0338232557312161,
-0.0131307504682182));
#27133=CARTESIAN_POINT('Ctrl Pts',(-0.0116371640909388,-0.0338260278274689,
-0.0131012753468492));
#27134=CARTESIAN_POINT('Ctrl Pts',(-0.0116060796922359,-0.0338287999237216,
-0.0130702059761426));
#27135=CARTESIAN_POINT('Ctrl Pts',(-0.0114036104318054,-0.0338468560644724,
-0.0128678346010635));
#27136=CARTESIAN_POINT('Ctrl Pts',(-0.0112724300594571,-0.0338649122052232,
-0.0125932627217097));
#27137=CARTESIAN_POINT('Ctrl Pts',(-0.0112424379684191,-0.0338829683459741,
-0.012308133242432));
#27138=CARTESIAN_POINT('Ctrl Pts',(-0.0112378277496764,-0.0338857438362993,
-0.012264304712178));
#27139=CARTESIAN_POINT('Ctrl Pts',(-0.0112355143538179,-0.0338885193266245,
-0.012220264539437));
#27140=CARTESIAN_POINT('Ctrl Pts',(-0.0112355000666595,-0.0338912948169497,
-0.0121762638737737));
#27141=CARTESIAN_POINT('Ctrl Pts',(-0.0112354071205807,-0.0339093509577008,
-0.0118900145559006));
#27142=CARTESIAN_POINT('Ctrl Pts',(-0.0113367660008467,-0.0339274070984519,
-0.0116030949718573));
#27143=CARTESIAN_POINT('Ctrl Pts',(-0.0115171632508829,-0.033945463239203,
-0.0113802452331895));
#27144=CARTESIAN_POINT('Ctrl Pts',(-0.0115448929207517,-0.033948238729528,
-0.0113459900010152));
#27145=CARTESIAN_POINT('Ctrl Pts',(-0.0115743968327725,-0.0339510142198529,
-0.0113132089188103));
#27146=CARTESIAN_POINT('Ctrl Pts',(-0.0116054990823748,-0.0339537897101779,
-0.0112820813031262));
#27147=CARTESIAN_POINT('Ctrl Pts',(-0.0118078749129517,-0.0339718492450012,
-0.0110795404207626));
#27148=CARTESIAN_POINT('Ctrl Pts',(-0.0120824850703501,-0.0339899087798247,
-0.0109483059244207));
#27149=CARTESIAN_POINT('Ctrl Pts',(-0.0123676699728074,-0.034007968314648,
-0.0109182965228678));
#27150=CARTESIAN_POINT('Ctrl Pts',(-0.012411445186685,-0.0340107404109007,
-0.01091369015009));
#27151=CARTESIAN_POINT('Ctrl Pts',(-0.0124554318294686,-0.0340135125071533,
-0.0109113749966697));
#27152=CARTESIAN_POINT('Ctrl Pts',(-0.0124993797185969,-0.034016284603406,
-0.0109113534386929));
#27153=CARTESIAN_POINT('Ctrl Pts',(-0.0127846345277401,-0.0340342775901722,
-0.0109112135112319));
#27154=CARTESIAN_POINT('Ctrl Pts',(-0.0130706677330489,-0.0340522705769383,
-0.0110118536863371));
#27155=CARTESIAN_POINT('Ctrl Pts',(-0.013293140892811,-0.0340702635637044,
-0.0111910244820692));
#27156=CARTESIAN_POINT('Ctrl Pts',(-0.0133282391328796,-0.0340731022080143,
-0.0112192911709975));
#27157=CARTESIAN_POINT('Ctrl Pts',(-0.013361797272371,-0.0340759408523243,
-0.0112494142841308));
#27158=CARTESIAN_POINT('Ctrl Pts',(-0.0133936236345209,-0.0340787794966342,
-0.0112812041654912));
#27159=CARTESIAN_POINT('Ctrl Pts',(-0.0135991441361798,-0.034097110199963,
-0.0114864890904258));
#27160=CARTESIAN_POINT('Ctrl Pts',(-0.0137311692055575,-0.0341154409032919,
-0.0117658387884295));
#27161=CARTESIAN_POINT('Ctrl Pts',(-0.0137588025739744,-0.0341337716066208,
-0.0120559519531405));
#27162=CARTESIAN_POINT('Ctrl Pts',(-0.0137625726997891,-0.034136272534368,
-0.0120955331983566));
#27163=CARTESIAN_POINT('Ctrl Pts',(-0.0137644736441105,-0.0341387734621151,
-0.012135284086788));
#27164=CARTESIAN_POINT('Ctrl Pts',(-0.0137644997276158,-0.0341412743898623,
-0.0121750233109846));
#27165=CARTESIAN_POINT('Origin',(-0.0125,-0.0412787743898723,-0.0121758532865581));
#27166=CARTESIAN_POINT('',(-0.0137644998286153,-0.0346412456228672,-0.0121763255635047));
#27167=CARTESIAN_POINT('',(-0.0137644998230799,-0.0345787397706929,-0.0121762999529358));
#27168=CARTESIAN_POINT('',(-0.0137645,-0.0412787743898723,-0.0121758532865581));
#27169=CARTESIAN_POINT('Ctrl Pts',(-0.0137644999999884,-0.0345787112306013,
-0.0121758478627298));
#27170=CARTESIAN_POINT('Ctrl Pts',(-0.0137644987506394,-0.0345603823010006,
-0.0118845772640469));
#27171=CARTESIAN_POINT('Ctrl Pts',(-0.0136596447418225,-0.0345420533713999,
-0.0115938183088325));
#27172=CARTESIAN_POINT('Ctrl Pts',(-0.0134742455564904,-0.0345237244417992,
-0.0113697479301321));
#27173=CARTESIAN_POINT('Ctrl Pts',(-0.0134489398502257,-0.0345212226697025,
-0.0113391638734878));
#27174=CARTESIAN_POINT('Ctrl Pts',(-0.0134222064093296,-0.0345187208976057,
-0.0113097888422845));
#27175=CARTESIAN_POINT('Ctrl Pts',(-0.0133941715204833,-0.034516219125509,
-0.0112817517587904));
#27176=CARTESIAN_POINT('Ctrl Pts',(-0.0131925617618852,-0.0344982279120871,
-0.0110801262176284));
#27177=CARTESIAN_POINT('Ctrl Pts',(-0.0129191353045024,-0.0344802366986654,
-0.0109490961761));
#27178=CARTESIAN_POINT('Ctrl Pts',(-0.0126350294464768,-0.0344622454852435,
-0.0109185835070023));
#27179=CARTESIAN_POINT('Ctrl Pts',(-0.012590190044376,-0.0344594059969679,
-0.0109137678025732));
#27180=CARTESIAN_POINT('Ctrl Pts',(-0.012545124963572,-0.0344565665086922,
-0.0109113570081699));
#27181=CARTESIAN_POINT('Ctrl Pts',(-0.0125001044084758,-0.0344537270204166,
-0.0109113532908685));
#27182=CARTESIAN_POINT('Ctrl Pts',(-0.0122137956630281,-0.0344356692615957,
-0.0109113296506473));
#27183=CARTESIAN_POINT('Ctrl Pts',(-0.011926853365667,-0.0344176115027748,
-0.0110127979724812));
#27184=CARTESIAN_POINT('Ctrl Pts',(-0.0117040303222684,-0.0343995537439538,
-0.0111933093831462));
#27185=CARTESIAN_POINT('Ctrl Pts',(-0.0116698136967697,-0.0343967808010773,
-0.011221028649712));
#27186=CARTESIAN_POINT('Ctrl Pts',(-0.0116370693711646,-0.0343940078582007,
-0.0112505187143577));
#27187=CARTESIAN_POINT('Ctrl Pts',(-0.0116059761418116,-0.0343912349153242,
-0.0112816041093206));
#27188=CARTESIAN_POINT('Ctrl Pts',(-0.0114035310908213,-0.0343731805487076,
-0.0114839981513443));
#27189=CARTESIAN_POINT('Ctrl Pts',(-0.0112723825734531,-0.034355126182091,
-0.0117585841309941));
#27190=CARTESIAN_POINT('Ctrl Pts',(-0.011242422954328,-0.0343370718154744,
-0.0120437161449255));
#27191=CARTESIAN_POINT('Ctrl Pts',(-0.0112378158726534,-0.0343342954803935,
-0.0120875627128921));
#27192=CARTESIAN_POINT('Ctrl Pts',(-0.0112355074760351,-0.0343315191453126,
-0.0121316208304898));
#27193=CARTESIAN_POINT('Ctrl Pts',(-0.0112355000181491,-0.0343287428102318,
-0.0121756390457791));
#27194=CARTESIAN_POINT('Ctrl Pts',(-0.0112354515198935,-0.0343106884436152,
-0.0124618872735694));
#27195=CARTESIAN_POINT('Ctrl Pts',(-0.0113368542227572,-0.0342926340769986,
-0.0127487903025532));
#27196=CARTESIAN_POINT('Ctrl Pts',(-0.0115172850280278,-0.0342745797103819,
-0.0129716117510821));
#27197=CARTESIAN_POINT('Ctrl Pts',(-0.0115450310234966,-0.0342718033753011,
-0.0130058764260746));
#27198=CARTESIAN_POINT('Ctrl Pts',(-0.0115745524544448,-0.0342690270402203,
-0.0130386654988026));
#27199=CARTESIAN_POINT('Ctrl Pts',(-0.0116056731727549,-0.0342662507051395,
-0.0130697994684224));
#27200=CARTESIAN_POINT('Ctrl Pts',(-0.0118080876541539,-0.0342481929463185,
-0.0132723001386087));
#27201=CARTESIAN_POINT('Ctrl Pts',(-0.0120827222510488,-0.0342301351874976,
-0.0134034810829045));
#27202=CARTESIAN_POINT('Ctrl Pts',(-0.0123679120285065,-0.0342120774286767,
-0.0134334354977024));
#27203=CARTESIAN_POINT('Ctrl Pts',(-0.012411705667003,-0.0342093044858002,
-0.0134380352867437));
#27204=CARTESIAN_POINT('Ctrl Pts',(-0.0124557104613993,-0.0342065315429236,
-0.0134403419773165));
#27205=CARTESIAN_POINT('Ctrl Pts',(-0.0124996759269194,-0.0342037586000471,
-0.0134403532450305));
#27206=CARTESIAN_POINT('Ctrl Pts',(-0.0127849295756885,-0.0341857673866254,
-0.0134404263514217));
#27207=CARTESIAN_POINT('Ctrl Pts',(-0.0130709383179884,-0.0341677761732036,
-0.0133397199571894));
#27208=CARTESIAN_POINT('Ctrl Pts',(-0.0132933691953534,-0.0341497849597818,
-0.0131604981818703));
#27209=CARTESIAN_POINT('Ctrl Pts',(-0.0133284746578713,-0.0341469454715061,
-0.0131322122559665));
#27210=CARTESIAN_POINT('Ctrl Pts',(-0.0133620383771549,-0.0341441059832304,
-0.0131020688045103));
#27211=CARTESIAN_POINT('Ctrl Pts',(-0.0133938684987958,-0.0341412664949547,
-0.0130702577570638));
#27212=CARTESIAN_POINT('Ctrl Pts',(-0.0135993323014577,-0.034122937565354,
-0.0128649170785468));
#27213=CARTESIAN_POINT('Ctrl Pts',(-0.0137312808987023,-0.0341046086357533,
-0.0125855319131322));
#27214=CARTESIAN_POINT('Ctrl Pts',(-0.0137588351903264,-0.0340862797061526,
-0.0122954116973699));
#27215=CARTESIAN_POINT('Ctrl Pts',(-0.0137625961605212,-0.0340837779340558,
-0.0122558122948785));
#27216=CARTESIAN_POINT('Ctrl Pts',(-0.013764486283383,-0.034081276161959,
-0.0122160436113997));
#27217=CARTESIAN_POINT('Ctrl Pts',(-0.013764499925554,-0.0340787743898623,
-0.0121762871919379));
#27218=CARTESIAN_POINT('Ctrl Pts',(-0.01376449999993,-0.0341413255815296,
-0.0121758399826972));
#27219=CARTESIAN_POINT('Ctrl Pts',(-0.0137645030485197,-0.0341595105759365,
-0.0124656011047135));
#27220=CARTESIAN_POINT('Ctrl Pts',(-0.0136606891579716,-0.0341776961989851,
-0.012755005442436));
#27221=CARTESIAN_POINT('Ctrl Pts',(-0.0134770965549167,-0.0341959072895615,
-0.0129785005144048));
#27222=CARTESIAN_POINT('Ctrl Pts',(-0.0134509381871666,-0.0341985020150379,
-0.0130103442062835));
#27223=CARTESIAN_POINT('Ctrl Pts',(-0.0134232395263884,-0.0342010972575229,
-0.0130408863505521));
#27224=CARTESIAN_POINT('Ctrl Pts',(-0.0133941435802119,-0.0342036930888617,
-0.0130699827559113));
#27225=CARTESIAN_POINT('Ctrl Pts',(-0.0131915881066192,-0.0342217643295428,
-0.0132725414261682));
#27226=CARTESIAN_POINT('Ctrl Pts',(-0.0129165508093684,-0.0342398641086831,
-0.0134038931150264));
#27227=CARTESIAN_POINT('Ctrl Pts',(-0.0126306236596915,-0.0342579197062186,
-0.0134335884373465));
#27228=CARTESIAN_POINT('Ctrl Pts',(-0.0125872163046045,-0.0342606607741249,
-0.0134380965625869));
#27229=CARTESIAN_POINT('Ctrl Pts',(-0.0125435961840299,-0.0342634008237744,
-0.0134403530572374));
#27230=CARTESIAN_POINT('Ctrl Pts',(-0.0125000066519147,-0.0342661396007313,
-0.0134403532865406));
#27231=CARTESIAN_POINT('Ctrl Pts',(-0.0122040785829089,-0.0342847330780403,
-0.0134403548432731));
#27232=CARTESIAN_POINT('Ctrl Pts',(-0.0119088287462426,-0.0343032678967875,
-0.0133322605654254));
#27233=CARTESIAN_POINT('Ctrl Pts',(-0.0116827236707415,-0.0343220359752789,
-0.0131407468825747));
#27234=CARTESIAN_POINT('Ctrl Pts',(-0.0116561432766619,-0.0343242423075397,
-0.0131182329732759));
#27235=CARTESIAN_POINT('Ctrl Pts',(-0.0116304947029669,-0.0343264518634068,
-0.0130946209095796));
#27236=CARTESIAN_POINT('Ctrl Pts',(-0.0116058658269969,-0.0343286651171383,
-0.0130699921631696));
#27237=CARTESIAN_POINT('Ctrl Pts',(-0.0114333146555468,-0.0343441712865858,
-0.0128974418994232));
#27238=CARTESIAN_POINT('Ctrl Pts',(-0.011310324410609,-0.0343598589648035,
-0.0126683334263073));
#27239=CARTESIAN_POINT('Ctrl Pts',(-0.0112614280346616,-0.0343751202607046,
-0.0124306075537998));
#27240=CARTESIAN_POINT('Ctrl Pts',(-0.0112439772708908,-0.0343805669070961,
-0.0123457649051789));
#27241=CARTESIAN_POINT('Ctrl Pts',(-0.0112355,-0.0343859592441231,-0.0122600429339026));
#27242=CARTESIAN_POINT('Ctrl Pts',(-0.0112355,-0.034391269638083,-0.0121758532865581));
#27243=CARTESIAN_POINT('Ctrl Pts',(-0.0112355,-0.0344114595538166,-0.0118557674514308));
#27244=CARTESIAN_POINT('Ctrl Pts',(-0.0113533279721126,-0.0344304649895133,
-0.0115562112741644));
#27245=CARTESIAN_POINT('Ctrl Pts',(-0.0115664721147305,-0.0344502780039842,
-0.0113229254247642));
#27246=CARTESIAN_POINT('Ctrl Pts',(-0.0117451590437316,-0.0344668880157188,
-0.0111273529286274));
#27247=CARTESIAN_POINT('Ctrl Pts',(-0.0119943711986191,-0.03448406560298,
-0.0109844551616016));
#27248=CARTESIAN_POINT('Ctrl Pts',(-0.012265501352359,-0.0345014958683265,
-0.0109332871377135));
#27249=CARTESIAN_POINT('Ctrl Pts',(-0.0123177849171256,-0.0345048570452173,
-0.0109234201175608));
#27250=CARTESIAN_POINT('Ctrl Pts',(-0.0123707825304687,-0.0345082276180931,
-0.0109168422232236));
#27251=CARTESIAN_POINT('Ctrl Pts',(-0.0124240318569026,-0.034511605328916,
-0.010913637341787));
#27252=CARTESIAN_POINT('Ctrl Pts',(-0.0127003824135621,-0.0345291347950834,
-0.0108970048164887));
#27253=CARTESIAN_POINT('Ctrl Pts',(-0.012989029181726,-0.0345468565109965,
-0.0109750528015166));
#27254=CARTESIAN_POINT('Ctrl Pts',(-0.0132239667471111,-0.0345648565559082,
-0.0111391120463842));
#27255=CARTESIAN_POINT('Ctrl Pts',(-0.013269055909737,-0.0345683111203197,
-0.011170598258306));
#27256=CARTESIAN_POINT('Ctrl Pts',(-0.0133121818315644,-0.0345717759364779,
-0.0112050969475248));
#27257=CARTESIAN_POINT('Ctrl Pts',(-0.0133529328811715,-0.0345752516128787,
-0.0112423299873221));
#27258=CARTESIAN_POINT('Ctrl Pts',(-0.0135629921327208,-0.0345931676663403,
-0.0114342549695773));
#27259=CARTESIAN_POINT('Ctrl Pts',(-0.0137095012841564,-0.0346113722860647,
-0.0117040258019251));
#27260=CARTESIAN_POINT('Ctrl Pts',(-0.0137515302674899,-0.0346298376912104,
-0.0119952093285727));
#27261=CARTESIAN_POINT('Ctrl Pts',(-0.0137601388925848,-0.034633619884771,
-0.0120548512617315));
#27262=CARTESIAN_POINT('Ctrl Pts',(-0.0137645006514589,-0.0346374130192336,
-0.0121152795154768));
#27263=CARTESIAN_POINT('Ctrl Pts',(-0.0137644999999269,-0.0346412168558721,
-0.0121758668844777));
#27264=CARTESIAN_POINT('Origin',(-0.0125,-0.0412787743898723,-0.0121758532865581));
#27265=CARTESIAN_POINT('',(-0.0137644999524637,-0.0351412586228095,-0.0121760944261459));
#27266=CARTESIAN_POINT('',(-0.0137644998439392,-0.0350788026914135,-0.0121754128237017));
#27267=CARTESIAN_POINT('',(-0.0137645,-0.0412787743898723,-0.0121758532865581));
#27268=CARTESIAN_POINT('Ctrl Pts',(-0.0137644996879007,-0.0350787743898623,
-0.0121749648615133));
#27269=CARTESIAN_POINT('Ctrl Pts',(-0.0137642950427078,-0.0350604396877818,
-0.011883692363005));
#27270=CARTESIAN_POINT('Ctrl Pts',(-0.013659236707341,-0.0350421049857011,
-0.0115930051217057));
#27271=CARTESIAN_POINT('Ctrl Pts',(-0.0134736789464501,-0.0350237702836206,
-0.0113690636242298));
#27272=CARTESIAN_POINT('Ctrl Pts',(-0.0134483913569099,-0.0350212716523678,
-0.0113385451450134));
#27273=CARTESIAN_POINT('Ctrl Pts',(-0.0134216813408798,-0.0350187730211151,
-0.0113092329057806));
#27274=CARTESIAN_POINT('Ctrl Pts',(-0.0133936746716602,-0.0350162743898623,
-0.0112812551470379));
#27275=CARTESIAN_POINT('Ctrl Pts',(-0.0131919498582662,-0.0349982773935308,
-0.0110797385683511));
#27276=CARTESIAN_POINT('Ctrl Pts',(-0.0129184463589703,-0.0349802803971992,
-0.0109488602095992));
#27277=CARTESIAN_POINT('Ctrl Pts',(-0.0126343199263155,-0.0349622834008676,
-0.0109185075077866));
#27278=CARTESIAN_POINT('Ctrl Pts',(-0.0125895414366565,-0.0349594470638658,
-0.0109137239044747));
#27279=CARTESIAN_POINT('Ctrl Pts',(-0.0125445392582302,-0.0349566107268641,
-0.0109113385101257));
#27280=CARTESIAN_POINT('Ctrl Pts',(-0.0124995824442955,-0.0349537743898623,
-0.0109113533554995));
#27281=CARTESIAN_POINT('Ctrl Pts',(-0.0122132696361486,-0.0349357108408525,
-0.0109114479000252));
#27282=CARTESIAN_POINT('Ctrl Pts',(-0.0119263662305414,-0.0349176472918427,
-0.0110130373568707));
#27283=CARTESIAN_POINT('Ctrl Pts',(-0.0117036166925373,-0.0348995837428329,
-0.0111936446134164));
#27284=CARTESIAN_POINT('Ctrl Pts',(-0.0116694612683676,-0.0348968139585094,
-0.0112213381274444));
#27285=CARTESIAN_POINT('Ctrl Pts',(-0.0116367746190418,-0.0348940441741858,
-0.0112507966940394));
#27286=CARTESIAN_POINT('Ctrl Pts',(-0.0116057347054632,-0.0348912743898623,
-0.0112818455500216));
#27287=CARTESIAN_POINT('Ctrl Pts',(-0.0114033415098123,-0.0348732142396919,
-0.011484297053878));
#27288=CARTESIAN_POINT('Ctrl Pts',(-0.0112722669203073,-0.0348551540895215,
-0.0117589223670615));
#27289=CARTESIAN_POINT('Ctrl Pts',(-0.0112423862595724,-0.034837093939351,
-0.0120440658444863));
#27290=CARTESIAN_POINT('Ctrl Pts',(-0.0112377980061822,-0.0348343207561881,
-0.0120878503691525));
#27291=CARTESIAN_POINT('Ctrl Pts',(-0.0112355018543397,-0.0348315475730252,
-0.0121318451990947));
#27292=CARTESIAN_POINT('Ctrl Pts',(-0.0112355000011239,-0.0348287743898623,
-0.0121757999728644));
#27293=CARTESIAN_POINT('Ctrl Pts',(-0.0112354879321933,-0.0348107142396919,
-0.0124620521849796));
#27294=CARTESIAN_POINT('Ctrl Pts',(-0.0113369297788642,-0.0347926540895215,
-0.0127489452454201));
#27295=CARTESIAN_POINT('Ctrl Pts',(-0.0115173927210527,-0.0347745939393511,
-0.0129717447272457));
#27296=CARTESIAN_POINT('Ctrl Pts',(-0.011545103276507,-0.0347718207561882,
-0.0130059561687829));
#27297=CARTESIAN_POINT('Ctrl Pts',(-0.0115745839409616,-0.0347690475730252,
-0.0130386960351572));
#27298=CARTESIAN_POINT('Ctrl Pts',(-0.0116056593225539,-0.0347662743898623,
-0.0130697856121092));
#27299=CARTESIAN_POINT('Ctrl Pts',(-0.0118080735322945,-0.0347482108408525,
-0.013272292285478));
#27300=CARTESIAN_POINT('Ctrl Pts',(-0.0120827101271603,-0.0347301472918427,
-0.0134034777225892));
#27301=CARTESIAN_POINT('Ctrl Pts',(-0.0123679029266934,-0.0347120837428329,
-0.013433434541676));
#27302=CARTESIAN_POINT('Ctrl Pts',(-0.0124116331230631,-0.0347093139585094,
-0.0134380279871747));
#27303=CARTESIAN_POINT('Ctrl Pts',(-0.0124555738847812,-0.0347065441741858,
-0.013440334978898));
#27304=CARTESIAN_POINT('Ctrl Pts',(-0.0124994758169154,-0.0347037743898623,
-0.0134403531779112));
#27305=CARTESIAN_POINT('Ctrl Pts',(-0.012784733735675,-0.0346857773935313,
-0.0134404714281197));
#27306=CARTESIAN_POINT('Ctrl Pts',(-0.0130707615942272,-0.0346677803972003,
-0.0133398074729649));
#27307=CARTESIAN_POINT('Ctrl Pts',(-0.0132932219367298,-0.0346497834008692,
-0.0131606168160872));
#27308=CARTESIAN_POINT('Ctrl Pts',(-0.0133282818150218,-0.0346469470638669,
-0.0131323762652073));
#27309=CARTESIAN_POINT('Ctrl Pts',(-0.0133618046077298,-0.0346441107268646,
-0.0131022832290055));
#27310=CARTESIAN_POINT('Ctrl Pts',(-0.0133935992326092,-0.0346412743898623,
-0.0130705267809012));
#27311=CARTESIAN_POINT('Ctrl Pts',(-0.0135991266344828,-0.0346229396877819,
-0.0128652461620435));
#27312=CARTESIAN_POINT('Ctrl Pts',(-0.0137311593212538,-0.0346046049857014,
-0.0125858983335253));
#27313=CARTESIAN_POINT('Ctrl Pts',(-0.0137587997171842,-0.034586270283621,
-0.0122957846086425));
#27314=CARTESIAN_POINT('Ctrl Pts',(-0.0137625665172561,-0.0345837716523681,
-0.0122562482574811));
#27315=CARTESIAN_POINT('Ctrl Pts',(-0.0137644683725183,-0.0345812730211152,
-0.0122165426039117));
#27316=CARTESIAN_POINT('Ctrl Pts',(-0.0137644996084897,-0.0345787743898623,
-0.0121768483389608));
#27317=CARTESIAN_POINT('Ctrl Pts',(-0.0137644996573036,-0.0346412743898623,
-0.0121767842425317));
#27318=CARTESIAN_POINT('Ctrl Pts',(-0.013764285216229,-0.0346596056746789,
-0.0124680554444549));
#27319=CARTESIAN_POINT('Ctrl Pts',(-0.0136592179638055,-0.0346779369594955,
-0.0127587381208865));
#27320=CARTESIAN_POINT('Ctrl Pts',(-0.0134736540784892,-0.0346962682443121,
-0.0129826729599929));
#27321=CARTESIAN_POINT('Ctrl Pts',(-0.013448339648412,-0.0346987689789078,
-0.0130132219152314));
#27322=CARTESIAN_POINT('Ctrl Pts',(-0.0134215999140004,-0.0347012697135035,
-0.0130425621095678));
#27323=CARTESIAN_POINT('Ctrl Pts',(-0.0133935610472872,-0.0347037704480992,
-0.0130705649187452));
#27324=CARTESIAN_POINT('Ctrl Pts',(-0.0131918126532027,-0.0347217640137402,
-0.0132720538676103));
#27325=CARTESIAN_POINT('Ctrl Pts',(-0.0129182953407975,-0.0347397575793813,
-0.0134028973345348));
#27326=CARTESIAN_POINT('Ctrl Pts',(-0.0126341674539392,-0.0347577511450224,
-0.0134332153443217));
#27327=CARTESIAN_POINT('Ctrl Pts',(-0.0125893467725896,-0.0347605895987936,
-0.0134379979577808));
#27328=CARTESIAN_POINT('Ctrl Pts',(-0.0125443022800829,-0.0347634280525648,
-0.0134403778704686));
#27329=CARTESIAN_POINT('Ctrl Pts',(-0.0124993037832106,-0.034766266506336,
-0.0134403530948943));
#27330=CARTESIAN_POINT('Ctrl Pts',(-0.0122129936694684,-0.0347843266211966,
-0.0134401954563507));
#27331=CARTESIAN_POINT('Ctrl Pts',(-0.0119261146312032,-0.0348023867360572,
-0.0133385445417751));
#27332=CARTESIAN_POINT('Ctrl Pts',(-0.0117034055697304,-0.0348204468509179,
-0.0131578907418842));
#27333=CARTESIAN_POINT('Ctrl Pts',(-0.0116692237128628,-0.0348232187554695,
-0.0131301636153379));
#27334=CARTESIAN_POINT('Ctrl Pts',(-0.0116365138032983,-0.0348259906600211,
-0.0131006684012419));
#27335=CARTESIAN_POINT('Ctrl Pts',(-0.0116054542621016,-0.0348287625645727,
-0.0130695804109131));
#27336=CARTESIAN_POINT('Ctrl Pts',(-0.0114031264267015,-0.0348468192848671,
-0.0128670672523849));
#27337=CARTESIAN_POINT('Ctrl Pts',(-0.011272138149275,-0.0348648760051615,
-0.0125924033996814));
#27338=CARTESIAN_POINT('Ctrl Pts',(-0.0112423456656896,-0.0348829327254559,
-0.0123072527743432));
#27339=CARTESIAN_POINT('Ctrl Pts',(-0.0112377665919671,-0.0348857080245738,
-0.0122634254199813));
#27340=CARTESIAN_POINT('Ctrl Pts',(-0.0112354840278291,-0.0348884833236916,
-0.0122193880730684));
#27341=CARTESIAN_POINT('Ctrl Pts',(-0.0112355000842078,-0.0348912586228095,
-0.0121753918089769));
#27342=CARTESIAN_POINT('Ctrl Pts',(-0.0112356045506192,-0.0349093153431039,
-0.0118891422189465));
#27343=CARTESIAN_POINT('Ctrl Pts',(-0.0113371614640519,-0.0349273720633983,
-0.0116022924016807));
#27344=CARTESIAN_POINT('Ctrl Pts',(-0.0115177126222287,-0.0349454287836927,
-0.0113795670582009));
#27345=CARTESIAN_POINT('Ctrl Pts',(-0.0115454631473433,-0.0349482040828106,
-0.0113453344046954));
#27346=CARTESIAN_POINT('Ctrl Pts',(-0.0115749865410915,-0.0349509793819284,
-0.0113125768291603));
#27347=CARTESIAN_POINT('Ctrl Pts',(-0.0116061068293765,-0.0349537546810463,
-0.0112814734737757));
#27348=CARTESIAN_POINT('Ctrl Pts',(-0.0118086204890069,-0.0349718147959071,
-0.011079070004115));
#27349=CARTESIAN_POINT('Ctrl Pts',(-0.0120833200690478,-0.0349898749107678,
-0.0109480221876352));
#27350=CARTESIAN_POINT('Ctrl Pts',(-0.0123685255462422,-0.0350079350256286,
-0.010918206786937));
#27351=CARTESIAN_POINT('Ctrl Pts',(-0.0124122994849158,-0.0350107069301801,
-0.0109136306563012));
#27352=CARTESIAN_POINT('Ctrl Pts',(-0.0124562832517799,-0.0350134788347316,
-0.0109113454273497));
#27353=CARTESIAN_POINT('Ctrl Pts',(-0.0125002267383571,-0.0350162507392831,
-0.0109113533068864));
#27354=CARTESIAN_POINT('Ctrl Pts',(-0.0127854818745024,-0.0350342443049242,
-0.0109114044561802));
#27355=CARTESIAN_POINT('Ctrl Pts',(-0.0130714478229443,-0.0350522378705653,
-0.0110122364028001));
#27356=CARTESIAN_POINT('Ctrl Pts',(-0.0132938009925633,-0.0350702314362064,
-0.0111915564643518));
#27357=CARTESIAN_POINT('Ctrl Pts',(-0.0133288768194129,-0.0350730698899776,
-0.011219843893042));
#27358=CARTESIAN_POINT('Ctrl Pts',(-0.013362411605519,-0.0350759083437487,
-0.0112499863474084));
#27359=CARTESIAN_POINT('Ctrl Pts',(-0.0133942138568448,-0.0350787467975199,
-0.011281794100471));
#27360=CARTESIAN_POINT('Ctrl Pts',(-0.0135995989622101,-0.0350970780823365,
-0.0114872147371192));
#27361=CARTESIAN_POINT('Ctrl Pts',(-0.0137314396478263,-0.0351154093671531,
-0.0117666516692974));
#27362=CARTESIAN_POINT('Ctrl Pts',(-0.0137588814672488,-0.0351337406519698,
-0.0120567831332134));
#27363=CARTESIAN_POINT('Ctrl Pts',(-0.0137626250513938,-0.0351362413865654,
-0.0120963625623891));
#27364=CARTESIAN_POINT('Ctrl Pts',(-0.0137644997485598,-0.0351387421211611,
-0.0121361103638794));
#27365=CARTESIAN_POINT('Ctrl Pts',(-0.0137644999999747,-0.0351412428557567,
-0.0121758452856833));
#27366=CARTESIAN_POINT('Origin',(-0.0125,-0.0412787743898723,-0.0121758532865581));
#27367=CARTESIAN_POINT('',(-0.0137644997162062,-0.0356413083664635,-0.0121752330744908));
#27368=CARTESIAN_POINT('',(-0.0137644999999548,-0.035578810380488,-0.0121758425904543));
#27369=CARTESIAN_POINT('',(-0.0137645,-0.0412787743898723,-0.0121758532865581));
#27370=CARTESIAN_POINT('Ctrl Pts',(-0.0137644998645128,-0.0355787743898623,
-0.0121752679258704));
#27371=CARTESIAN_POINT('Ctrl Pts',(-0.0137643650298108,-0.0355604448524855,
-0.0118839971487647));
#27372=CARTESIAN_POINT('Ctrl Pts',(-0.0136593775416596,-0.0355421153151086,
-0.0115932861456091));
#27373=CARTESIAN_POINT('Ctrl Pts',(-0.0134738753817643,-0.0355237857777318,
-0.0113693007521294));
#27374=CARTESIAN_POINT('Ctrl Pts',(-0.0134485598460573,-0.0355212843402379,
-0.0113387333979288));
#27375=CARTESIAN_POINT('Ctrl Pts',(-0.0134218176053227,-0.035518782902744,
-0.0113093753215851));
#27376=CARTESIAN_POINT('Ctrl Pts',(-0.0133937749411315,-0.0355162814652501,
-0.0112813553242321));
#27377=CARTESIAN_POINT('Ctrl Pts',(-0.0131920754641933,-0.0354982896428374,
-0.011079818880641));
#27378=CARTESIAN_POINT('Ctrl Pts',(-0.0129185904718619,-0.0354802978204246,
-0.0109489100783296));
#27379=CARTESIAN_POINT('Ctrl Pts',(-0.012634470720931,-0.0354623059980119,
-0.0109185236260425));
#27380=CARTESIAN_POINT('Ctrl Pts',(-0.01258963594707,-0.0354594668455539,
-0.0109137285714492));
#27381=CARTESIAN_POINT('Ctrl Pts',(-0.0125445766306353,-0.0354566276930959,
-0.0109113378005705));
#27382=CARTESIAN_POINT('Ctrl Pts',(-0.0124995628543102,-0.0354537885406379,
-0.0109113533621201));
#27383=CARTESIAN_POINT('Ctrl Pts',(-0.0122132536914851,-0.0354357301720729,
-0.010911452341024));
#27384=CARTESIAN_POINT('Ctrl Pts',(-0.0119263545560491,-0.0354176718035078,
-0.0110130438307979));
#27385=CARTESIAN_POINT('Ctrl Pts',(-0.0117036087326358,-0.0353996134349428,
-0.011193651067427));
#27386=CARTESIAN_POINT('Ctrl Pts',(-0.0116694092714644,-0.0353968408286371,
-0.0112213807464024));
#27387=CARTESIAN_POINT('Ctrl Pts',(-0.0116366824156856,-0.0353940682223314,
-0.0112508800461999));
#27388=CARTESIAN_POINT('Ctrl Pts',(-0.011605606805275,-0.0353912956160257,
-0.0112819735053629));
#27389=CARTESIAN_POINT('Ctrl Pts',(-0.0114032450821832,-0.0353732406403693,
-0.0114844514580067));
#27390=CARTESIAN_POINT('Ctrl Pts',(-0.0112722099834925,-0.0353551856647129,
-0.0117590920093227));
#27391=CARTESIAN_POINT('Ctrl Pts',(-0.0112423683634143,-0.0353371306890566,
-0.0120442367349436));
#27392=CARTESIAN_POINT('Ctrl Pts',(-0.0112377801371288,-0.0353343546898422,
-0.0120880784741608));
#27393=CARTESIAN_POINT('Ctrl Pts',(-0.0112354899766516,-0.0353315786906279,
-0.0121321307471615));
#27394=CARTESIAN_POINT('Ctrl Pts',(-0.0112355000330095,-0.0353288026914135,
-0.012176142217244));
#27395=CARTESIAN_POINT('Ctrl Pts',(-0.0112355654391149,-0.0353107477157571,
-0.0124623908648782));
#27396=CARTESIAN_POINT('Ctrl Pts',(-0.0113370825786684,-0.0352926927401007,
-0.0127492538332294));
#27397=CARTESIAN_POINT('Ctrl Pts',(-0.0115176024370534,-0.0352746377644444,
-0.012972003572821));
#27398=CARTESIAN_POINT('Ctrl Pts',(-0.0115453578322745,-0.03527186176523,
-0.013006251921524));
#27399=CARTESIAN_POINT('Ctrl Pts',(-0.0115748875291204,-0.0352690857660157,
-0.0130390244141873));
#27400=CARTESIAN_POINT('Ctrl Pts',(-0.0116060153910218,-0.0352663097668013,
-0.0130701417013942));
#27401=CARTESIAN_POINT('Ctrl Pts',(-0.0118085076683799,-0.0352482513982362,
-0.013272565188484));
#27402=CARTESIAN_POINT('Ctrl Pts',(-0.0120831928824371,-0.0352301930296712,
-0.0134036410334657));
#27403=CARTESIAN_POINT('Ctrl Pts',(-0.0123683944744434,-0.0352121346611062,
-0.0134334860770192));
#27404=CARTESIAN_POINT('Ctrl Pts',(-0.012412183132845,-0.0352093620548005,
-0.0134380683600561));
#27405=CARTESIAN_POINT('Ctrl Pts',(-0.0124561820031353,-0.0352065894484948,
-0.0134403581705277));
#27406=CARTESIAN_POINT('Ctrl Pts',(-0.012500140715678,-0.0352038168421891,
-0.0134403532787286));
#27407=CARTESIAN_POINT('Ctrl Pts',(-0.0127853948276369,-0.035185825019777,
-0.013440321535173));
#27408=CARTESIAN_POINT('Ctrl Pts',(-0.0130713668724668,-0.0351678331973647,
-0.0133395097199173));
#27409=CARTESIAN_POINT('Ctrl Pts',(-0.0132937319760708,-0.0351498413749526,
-0.0131602057641609));
#27410=CARTESIAN_POINT('Ctrl Pts',(-0.0133288217194071,-0.035147002222494,
-0.0131319111725874));
#27411=CARTESIAN_POINT('Ctrl Pts',(-0.0133623695013503,-0.0351441630700355,
-0.0131017601841739));
#27412=CARTESIAN_POINT('Ctrl Pts',(-0.0133941836226608,-0.0351413239175769,
-0.0130699427110371));
#27413=CARTESIAN_POINT('Ctrl Pts',(-0.0135995752436411,-0.0351229943802,
-0.0128645294507032));
#27414=CARTESIAN_POINT('Ctrl Pts',(-0.013731425379661,-0.0351046648428231,
-0.0125850975507378));
#27415=CARTESIAN_POINT('Ctrl Pts',(-0.0137588773038086,-0.0350863353054463,
-0.0122949674500972));
#27416=CARTESIAN_POINT('Ctrl Pts',(-0.0137626236761763,-0.0350838338679524,
-0.0122553733077617));
#27417=CARTESIAN_POINT('Ctrl Pts',(-0.0137644997642347,-0.0350813324304586,
-0.012215610600945));
#27418=CARTESIAN_POINT('Ctrl Pts',(-0.0137644999999778,-0.0350788309929647,
-0.01217586078589));
#27419=CARTESIAN_POINT('Ctrl Pts',(-0.0137644999049527,-0.0351412743898623,
-0.0121763435666085));
#27420=CARTESIAN_POINT('Ctrl Pts',(-0.0137643869710071,-0.0351596085328665,
-0.0124676157963035));
#27421=CARTESIAN_POINT('Ctrl Pts',(-0.013659420380221,-0.0351779426758707,
-0.0127583358472446));
#27422=CARTESIAN_POINT('Ctrl Pts',(-0.0134739334875397,-0.0351962768188749,
-0.0129823356557694));
#27423=CARTESIAN_POINT('Ctrl Pts',(-0.0134486491288289,-0.035198776009204,
-0.0130128698429997));
#27424=CARTESIAN_POINT('Ctrl Pts',(-0.0134219412424153,-0.0352012751995332,
-0.0130421976272212));
#27425=CARTESIAN_POINT('Ctrl Pts',(-0.0133939356586194,-0.0352037743898623,
-0.0130701906324454));
#27426=CARTESIAN_POINT('Ctrl Pts',(-0.0131922701491049,-0.0352217708185307,
-0.0132717655648774));
#27427=CARTESIAN_POINT('Ctrl Pts',(-0.0129188055429118,-0.0352397672471992,
-0.0134027236820722));
#27428=CARTESIAN_POINT('Ctrl Pts',(-0.0126346885717544,-0.0352577636758676,
-0.0134331596289579));
#27429=CARTESIAN_POINT('Ctrl Pts',(-0.0125899011988981,-0.0352606005805325,
-0.0134379574630889));
#27430=CARTESIAN_POINT('Ctrl Pts',(-0.0125448893315503,-0.0352634374851974,
-0.0134403560505243));
#27431=CARTESIAN_POINT('Ctrl Pts',(-0.012499922208476,-0.0352662743898623,
-0.0134403532841652));
#27432=CARTESIAN_POINT('Ctrl Pts',(-0.0122136100445227,-0.0352843373713921,
-0.0134403356703577));
#27433=CARTESIAN_POINT('Ctrl Pts',(-0.0119266798407084,-0.0353024003529218,
-0.0133388237427738));
#27434=CARTESIAN_POINT('Ctrl Pts',(-0.0117038819485851,-0.0353204633344516,
-0.0131582769722515));
#27435=CARTESIAN_POINT('Ctrl Pts',(-0.0116697110371408,-0.0353232336862552,
-0.0131305861909417));
#27436=CARTESIAN_POINT('Ctrl Pts',(-0.0116370091137744,-0.0353260040380587,
-0.0131011291320357));
#27437=CARTESIAN_POINT('Ctrl Pts',(-0.0116059543096101,-0.0353287743898623,
-0.0130700806365621));
#27438=CARTESIAN_POINT('Ctrl Pts',(-0.0114035118493503,-0.0353468339735561,
-0.0128676793018832));
#27439=CARTESIAN_POINT('Ctrl Pts',(-0.01127236984912,-0.0353648935572498,
-0.0125930868256952));
#27440=CARTESIAN_POINT('Ctrl Pts',(-0.0112424188376614,-0.0353829531409437,
-0.0123079512431328));
#27441=CARTESIAN_POINT('Ctrl Pts',(-0.011237818697999,-0.0353857268905832,
-0.0122641576135141));
#27442=CARTESIAN_POINT('Ctrl Pts',(-0.011235511681278,-0.0353885006402228,
-0.0122201530146197));
#27443=CARTESIAN_POINT('Ctrl Pts',(-0.011235500044295,-0.0353912743898623,
-0.0121761879835687));
#27444=CARTESIAN_POINT('Ctrl Pts',(-0.0112354242771583,-0.0354093339735561,
-0.0118899364248321));
#27445=CARTESIAN_POINT('Ctrl Pts',(-0.0113368018549001,-0.0354273935572499,
-0.011603021273402));
#27446=CARTESIAN_POINT('Ctrl Pts',(-0.0115172146027577,-0.0354454531409437,
-0.0113801818009766));
#27447=CARTESIAN_POINT('Ctrl Pts',(-0.0115449239787224,-0.0354482268905832,
-0.0113459561556465));
#27448=CARTESIAN_POINT('Ctrl Pts',(-0.0115744046216873,-0.0354510006402228,
-0.0113132023786766));
#27449=CARTESIAN_POINT('Ctrl Pts',(-0.0116054810537669,-0.0354537743898623,
-0.0112820993468017));
#27450=CARTESIAN_POINT('Ctrl Pts',(-0.0118078544081118,-0.0354718373713921,
-0.0110795527714841));
#27451=CARTESIAN_POINT('Ctrl Pts',(-0.0120824641821012,-0.0354899003529219,
-0.0109483126018268));
#27452=CARTESIAN_POINT('Ctrl Pts',(-0.0123676504375781,-0.0355079633344517,
-0.0109182985786719));
#27453=CARTESIAN_POINT('Ctrl Pts',(-0.0124113899639629,-0.0355107336862552,
-0.0109136952742262));
#27454=CARTESIAN_POINT('Ctrl Pts',(-0.0124553406130904,-0.0355135040380588,
-0.0109113794547743));
#27455=CARTESIAN_POINT('Ctrl Pts',(-0.0124992528144902,-0.0355162743898623,
-0.0109113535073118));
#27456=CARTESIAN_POINT('Ctrl Pts',(-0.0127845100150923,-0.0355342708185307,
-0.0109111849505036));
#27457=CARTESIAN_POINT('Ctrl Pts',(-0.0130705551071837,-0.0355522672471992,
-0.011011798004815));
#27458=CARTESIAN_POINT('Ctrl Pts',(-0.0132930468687106,-0.0355702636758676,
-0.0111909487662982));
#27459=CARTESIAN_POINT('Ctrl Pts',(-0.0133281198227843,-0.0355731005805325,
-0.0112191895712011));
#27460=CARTESIAN_POINT('Ctrl Pts',(-0.0133616553129469,-0.0355759374851974,
-0.011249283986549));
#27461=CARTESIAN_POINT('Ctrl Pts',(-0.0133934620940176,-0.0355787743898623,
-0.0112810428392825));
#27462=CARTESIAN_POINT('Ctrl Pts',(-0.0135990206663115,-0.0355971085328665,
-0.0114862916637728));
#27463=CARTESIAN_POINT('Ctrl Pts',(-0.0137310961679854,-0.0356154426758706,
-0.0117656188650991));
#27464=CARTESIAN_POINT('Ctrl Pts',(-0.0137587812276437,-0.0356337768188748,
-0.0120557280563526));
#27465=CARTESIAN_POINT('Ctrl Pts',(-0.0137625550737048,-0.035636276009204,
-0.0120952738417772));
#27466=CARTESIAN_POINT('Ctrl Pts',(-0.0137644630553627,-0.0356387751995331,
-0.0121349893031318));
#27467=CARTESIAN_POINT('Ctrl Pts',(-0.013764499468231,-0.0356412743898623,
-0.0121746936126288));
#27468=CARTESIAN_POINT('Origin',(-0.0125,-0.0412787743898723,-0.0121758532865581));
#27469=CARTESIAN_POINT('',(-0.0137644999998975,-0.0361412743898623,-0.0121758693894333));
#27470=CARTESIAN_POINT('',(-0.0137644999785623,-0.0360787101931254,-0.0121759146659024));
#27471=CARTESIAN_POINT('',(-0.0137645,-0.0412787743898723,-0.0121758532865581));
#27472=CARTESIAN_POINT('',(-0.0133941365248078,-0.0365787743898683,-0.0112817167617503));
#27473=CARTESIAN_POINT('Ctrl Pts',(-0.0137644999998975,-0.0361412743898623,
-0.0121758693894333));
#27474=CARTESIAN_POINT('Ctrl Pts',(-0.0137644963111485,-0.036159503556529,
-0.0124655333785947));
#27475=CARTESIAN_POINT('Ctrl Pts',(-0.0136609354141153,-0.0361777327231956,
-0.0127544975137962));
#27476=CARTESIAN_POINT('Ctrl Pts',(-0.0134774627796051,-0.0361959618898623,
-0.0129780544860627));
#27477=CARTESIAN_POINT('Ctrl Pts',(-0.013293990145095,-0.036214191056529,
-0.0132016114583292));
#27478=CARTESIAN_POINT('Ctrl Pts',(-0.0130304113544186,-0.0362324202231956,
-0.013359623744977));
#27479=CARTESIAN_POINT('Ctrl Pts',(-0.012746679867081,-0.0362506493898623,
-0.0134160586297077));
#27480=CARTESIAN_POINT('Ctrl Pts',(-0.0124629483797433,-0.036268878556529,
-0.0134724935144385));
#27481=CARTESIAN_POINT('Ctrl Pts',(-0.0121590383423167,-0.0362871077231956,
-0.0134274095583513));
#27482=CARTESIAN_POINT('Ctrl Pts',(-0.0119039099503849,-0.0363053368898623,
-0.0132910379810145));
#27483=CARTESIAN_POINT('Ctrl Pts',(-0.011648781558453,-0.036323566056529,
-0.0131546664036777));
#27484=CARTESIAN_POINT('Ctrl Pts',(-0.0114424524832276,-0.0363417952231956,
-0.0129270102800231));
#27485=CARTESIAN_POINT('Ctrl Pts',(-0.0113317512500114,-0.0363600243898623,
-0.0126597490482156));
#27486=CARTESIAN_POINT('Ctrl Pts',(-0.0112210500167952,-0.036378253556529,
-0.012392487816408));
#27487=CARTESIAN_POINT('Ctrl Pts',(-0.0112059734241391,-0.0363964827231956,
-0.0120856137473264));
#27488=CARTESIAN_POINT('Ctrl Pts',(-0.0112899506983871,-0.0364147118898623,
-0.011808782533615));
#27489=CARTESIAN_POINT('Ctrl Pts',(-0.0113739279726352,-0.036432941056529,
-0.0115319513199036));
#27490=CARTESIAN_POINT('Ctrl Pts',(-0.0115569487924721,-0.0364511702231956,
-0.0112851776311697));
#27491=CARTESIAN_POINT('Ctrl Pts',(-0.0117974847876132,-0.0364693993898623,
-0.0111244577252373));
#27492=CARTESIAN_POINT('Ctrl Pts',(-0.0120380207827542,-0.036487628556529,
-0.0109637378193049));
#27493=CARTESIAN_POINT('Ctrl Pts',(-0.0123361316429891,-0.0365058577231956,
-0.0108890948247504));
#27494=CARTESIAN_POINT('Ctrl Pts',(-0.0126239446771135,-0.0365240868898623,
-0.0109174423969774));
#27495=CARTESIAN_POINT('Ctrl Pts',(-0.0129117577112379,-0.036542316056529,
-0.0109457899692044));
#27496=CARTESIAN_POINT('Ctrl Pts',(-0.0131893131537922,-0.0365605452231956,
-0.0110768933907296));
#27497=CARTESIAN_POINT('Ctrl Pts',(-0.0133941365248104,-0.0365787743898623,
-0.0112817167617477));
#27498=CARTESIAN_POINT('',(-0.0137648283188305,-0.0365787649813118,-0.0121757910623594));
#27499=CARTESIAN_POINT('Origin',(-0.01249999999999,-0.0365787743898623,
-0.0121758532865681));
#27500=CARTESIAN_POINT('Ctrl Pts',(-0.0137644999970264,-0.0365787634361464,
-0.0121757665671622));
#27501=CARTESIAN_POINT('Ctrl Pts',(-0.0137644800216386,-0.0365604308650495,
-0.011884495191133));
#27502=CARTESIAN_POINT('Ctrl Pts',(-0.0136596068291505,-0.0365420982939525,
-0.0115937425877689));
#27503=CARTESIAN_POINT('Ctrl Pts',(-0.0134741927136686,-0.0365237657228555,
-0.0113696840694362));
#27504=CARTESIAN_POINT('Ctrl Pts',(-0.0134489204127944,-0.0365212669581236,
-0.0113391444620604));
#27505=CARTESIAN_POINT('Ctrl Pts',(-0.0134222244523923,-0.0365187681933917,
-0.0113098105901343));
#27506=CARTESIAN_POINT('Ctrl Pts',(-0.0133942305890836,-0.0365162694286598,
-0.0112818108359177));
#27507=CARTESIAN_POINT('Ctrl Pts',(-0.0131926327748777,-0.0364982745737657,
-0.0110801705983359));
#27508=CARTESIAN_POINT('Ctrl Pts',(-0.0129192130519281,-0.0364802797188715,
-0.0109491223851327));
#27509=CARTESIAN_POINT('Ctrl Pts',(-0.0126351075664765,-0.0364622848639774,
-0.0109185918994628));
#27510=CARTESIAN_POINT('Ctrl Pts',(-0.0125902969703159,-0.0364594466217859,
-0.0109137764723275));
#27511=CARTESIAN_POINT('Ctrl Pts',(-0.0125452608315856,-0.0364566083795944,
-0.0109113628806159));
#27512=CARTESIAN_POINT('Ctrl Pts',(-0.0125002688378061,-0.036453770137403,
-0.0109113533151361));
#27513=CARTESIAN_POINT('Ctrl Pts',(-0.0122139582707617,-0.0364357087299618,
-0.010911292444352));
#27514=CARTESIAN_POINT('Ctrl Pts',(-0.011927001428768,-0.0364176473225207,
-0.0110127246613591));
#27515=CARTESIAN_POINT('Ctrl Pts',(-0.0117041544539178,-0.0363995859150795,
-0.0111932088357107));
#27516=CARTESIAN_POINT('Ctrl Pts',(-0.0116699565291717,-0.0363968142254351,
-0.0112209057977919));
#27517=CARTESIAN_POINT('Ctrl Pts',(-0.0116372287675296,-0.0363940425357906,
-0.0112503714453245));
#27518=CARTESIAN_POINT('Ctrl Pts',(-0.0116061496458173,-0.0363912708461462,
-0.0112814306826803));
#27519=CARTESIAN_POINT('Ctrl Pts',(-0.0114036640767703,-0.0363732128340805,
-0.0114837867018874));
#27520=CARTESIAN_POINT('Ctrl Pts',(-0.0112724621911305,-0.0363551548220149,
-0.0117583489942559));
#27521=CARTESIAN_POINT('Ctrl Pts',(-0.0112424481357505,-0.0363370968099492,
-0.0120434767073505));
#27522=CARTESIAN_POINT('Ctrl Pts',(-0.0112378356925221,-0.0363343217249293,
-0.0120872940246996));
#27523=CARTESIAN_POINT('Ctrl Pts',(-0.0112355189166647,-0.0363315466399093,
-0.0121313230566792));
#27524=CARTESIAN_POINT('Ctrl Pts',(-0.0112355001154928,-0.0363287715548894,
-0.0121753128410888));
#27525=CARTESIAN_POINT('Ctrl Pts',(-0.0112353777726506,-0.0363107135428238,
-0.0124615628305231));
#27526=CARTESIAN_POINT('Ctrl Pts',(-0.0113367076382122,-0.0362926555307582,
-0.0127484933262912));
#27527=CARTESIAN_POINT('Ctrl Pts',(-0.0115170826499863,-0.0362745975186926,
-0.0129713617610837));
#27528=CARTESIAN_POINT('Ctrl Pts',(-0.0115448019798509,-0.0362718224336726,
-0.013005611314831));
#27529=CARTESIAN_POINT('Ctrl Pts',(-0.0115742948215681,-0.0362690473486526,
-0.0130383876299737));
#27530=CARTESIAN_POINT('Ctrl Pts',(-0.0116053854225937,-0.0362662722636327,
-0.0130695115030437));
#27531=CARTESIAN_POINT('Ctrl Pts',(-0.0118077359843553,-0.0362482108561913,
-0.0132720786131075));
#27532=CARTESIAN_POINT('Ctrl Pts',(-0.0120823301407312,-0.0362301494487498,
-0.0134033480734044));
#27533=CARTESIAN_POINT('Ctrl Pts',(-0.0123675118223398,-0.0362120880413084,
-0.0134333933983558));
#27534=CARTESIAN_POINT('Ctrl Pts',(-0.0124112755830647,-0.0362093163516642,
-0.0134380041307306));
#27535=CARTESIAN_POINT('Ctrl Pts',(-0.0124552509563464,-0.0362065446620201,
-0.013440324809775));
#27536=CARTESIAN_POINT('Ctrl Pts',(-0.0124991879468924,-0.0362037729723759,
-0.0134403530258106));
#27537=CARTESIAN_POINT('Ctrl Pts',(-0.0127844434664075,-0.0361857781174813,
-0.0134405362149596));
#27538=CARTESIAN_POINT('Ctrl Pts',(-0.0130704924772702,-0.0361677832625866,
-0.0133399389361538));
#27539=CARTESIAN_POINT('Ctrl Pts',(-0.0132929929969568,-0.036149788407692,
-0.0131608011820214));
#27540=CARTESIAN_POINT('Ctrl Pts',(-0.013328086937207,-0.036146950165501,
-0.0131325466428907));
#27541=CARTESIAN_POINT('Ctrl Pts',(-0.0133616418066973,-0.0361441119233101,
-0.0131024363525336));
#27542=CARTESIAN_POINT('Ctrl Pts',(-0.013393466037558,-0.0361412736811191,
-0.0130706597962184));
#27543=CARTESIAN_POINT('Ctrl Pts',(-0.0135990230033344,-0.0361229410950005,
-0.012865410766711));
#27544=CARTESIAN_POINT('Ctrl Pts',(-0.0137310972748207,-0.0361046085088818,
-0.0125860839173667));
#27545=CARTESIAN_POINT('Ctrl Pts',(-0.0137587815333782,-0.0360862759227632,
-0.0122959753129568));
#27546=CARTESIAN_POINT('Ctrl Pts',(-0.0137625575850322,-0.0360837754117962,
-0.0122564053503643));
#27547=CARTESIAN_POINT('Ctrl Pts',(-0.0137644654887648,-0.0360812749008293,
-0.0122166655083911));
#27548=CARTESIAN_POINT('Ctrl Pts',(-0.0137644995356581,-0.0360787743898623,
-0.0121769369472666));
#27549=CARTESIAN_POINT('Origin',(-0.0125,-0.0412787743898723,-0.0121758532865581));
#27550=CARTESIAN_POINT('Ctrl Pts',(-0.0137644999999428,-0.0360787070941287,
-0.0121758653168742));
#27551=CARTESIAN_POINT('Ctrl Pts',(-0.0137645027710451,-0.0360604037462595,
-0.0118845962566965));
#27552=CARTESIAN_POINT('Ctrl Pts',(-0.0136596538279521,-0.0360420968508638,
-0.0115938372087226));
#27553=CARTESIAN_POINT('Ctrl Pts',(-0.0134489478207998,-0.0360212816143236,
-0.0113391724258185));
#27554=CARTESIAN_POINT('Ctrl Pts',(-0.0134222076012039,-0.0360187809718295,
-0.011309789642501));
#27555=CARTESIAN_POINT('Ctrl Pts',(-0.0131925528985201,-0.035998300488268,
-0.0110801201704503));
#27556=CARTESIAN_POINT('Ctrl Pts',(-0.0129191234392818,-0.0359803126804235,
-0.0109490916009595));
#27557=CARTESIAN_POINT('Ctrl Pts',(-0.0125901687238666,-0.0359594902232465,
-0.0109137660339032));
#27558=CARTESIAN_POINT('Ctrl Pts',(-0.0125450967097083,-0.0359566516063094,
-0.0109113557557444));
#27559=CARTESIAN_POINT('Ctrl Pts',(-0.0122137592380001,-0.0359357645411937,
-0.0109113376000308));
#27560=CARTESIAN_POINT('Ctrl Pts',(-0.011926818932112,-0.0359177219816858,
-0.0110128147670077));
#27561=CARTESIAN_POINT('Ctrl Pts',(-0.0116697789103805,-0.0358968631466295,
-0.0112210585362829));
#27562=CARTESIAN_POINT('Ctrl Pts',(-0.0116370299322194,-0.0358940851140304,
-0.0112505551257888));
#27563=CARTESIAN_POINT('Ctrl Pts',(-0.0114035277909905,-0.0358732173124676,
-0.0114840211069177));
#27564=CARTESIAN_POINT('Ctrl Pts',(-0.0112723991914978,-0.0358550825527723,
-0.0117585659288796));
#27565=CARTESIAN_POINT('Ctrl Pts',(-0.0112378150477382,-0.0358342964986842,
-0.0120875490318841));
#27566=CARTESIAN_POINT('Ctrl Pts',(-0.0112355044165741,-0.0358315258616311,
-0.0121316580707312));
#27567=CARTESIAN_POINT('Ctrl Pts',(-0.011235471344901,-0.035810775654875,
-0.0124621217168363));
#27568=CARTESIAN_POINT('Ctrl Pts',(-0.0113369931344784,-0.0357929409320698,
-0.0127491482396458));
#27569=CARTESIAN_POINT('Ctrl Pts',(-0.011545280568908,-0.0357722991176314,
-0.0130061558519736));
#27570=CARTESIAN_POINT('Ctrl Pts',(-0.0115747139842782,-0.0357695554470609,
-0.0130388315090776));
#27571=CARTESIAN_POINT('Ctrl Pts',(-0.0118080646633445,-0.0357489005707485,
-0.0132722483314945));
#27572=CARTESIAN_POINT('Ctrl Pts',(-0.0120825614129742,-0.0357308942040033,
-0.0134033983119082));
#27573=CARTESIAN_POINT('Ctrl Pts',(-0.0124115825287087,-0.0357100660326244,
-0.0134380324734021));
#27574=CARTESIAN_POINT('Ctrl Pts',(-0.012455753473972,-0.0357072824220144,
-0.0134403492366539));
#27575=CARTESIAN_POINT('Ctrl Pts',(-0.0127851523474117,-0.035686499711345,
-0.0134403794262162));
#27576=CARTESIAN_POINT('Ctrl Pts',(-0.0130711567415406,-0.0356684713902834,
-0.01333961612615));
#27577=CARTESIAN_POINT('Ctrl Pts',(-0.0133286829772299,-0.0356475433198898,
-0.0131320329729809));
#27578=CARTESIAN_POINT('Ctrl Pts',(-0.0133622591511792,-0.0356446881239693,
-0.0131018645347246));
#27579=CARTESIAN_POINT('Ctrl Pts',(-0.0135995132123415,-0.03562340395237,
-0.0128646302103059));
#27580=CARTESIAN_POINT('Ctrl Pts',(-0.0137313901983395,-0.0356049261749303,
-0.0125852062335056));
#27581=CARTESIAN_POINT('Ctrl Pts',(-0.0137626208620077,-0.0355838735829413,
-0.0122554389422992));
#27582=CARTESIAN_POINT('Ctrl Pts',(-0.0137645003365433,-0.0355813423894253,
-0.0122156342959332));
#27583=CARTESIAN_POINT('Ctrl Pts',(-0.0137644999999548,-0.035578810380488,
-0.0121758425904543));
#27584=CARTESIAN_POINT('Ctrl Pts',(-0.0137644999999968,-0.0356413472503601,
-0.0121758504516997));
#27585=CARTESIAN_POINT('Ctrl Pts',(-0.0137645006529895,-0.0356596747292774,
-0.0124671204460104));
#27586=CARTESIAN_POINT('Ctrl Pts',(-0.0136596489458883,-0.0356780022081948,
-0.0127578796025123));
#27587=CARTESIAN_POINT('Ctrl Pts',(-0.013474251883555,-0.0356963296871122,
-0.0129819509961378));
#27588=CARTESIAN_POINT('Ctrl Pts',(-0.0134489342907337,-0.0356988324648953,
-0.0130125499076594));
#27589=CARTESIAN_POINT('Ctrl Pts',(-0.0134221875850932,-0.0357013352426784,
-0.013041938643616));
#27590=CARTESIAN_POINT('Ctrl Pts',(-0.0133941382376717,-0.0357038380204616,
-0.0130699880985039));
#27591=CARTESIAN_POINT('Ctrl Pts',(-0.0131925219158135,-0.035721827774144,
-0.0132716051928208));
#27592=CARTESIAN_POINT('Ctrl Pts',(-0.0129190918965321,-0.0357398175278265,
-0.0134026249827858));
#27593=CARTESIAN_POINT('Ctrl Pts',(-0.0126349860273449,-0.0357578072815089,
-0.0134331277285244));
#27594=CARTESIAN_POINT('Ctrl Pts',(-0.012590126959616,-0.0357606477845269,
-0.0134379439779772));
#27595=CARTESIAN_POINT('Ctrl Pts',(-0.0125450421010048,-0.035763488287545,
-0.0134403532149679));
#27596=CARTESIAN_POINT('Ctrl Pts',(-0.0125000020098496,-0.035766328790563,
-0.0134403532865565));
#27597=CARTESIAN_POINT('Ctrl Pts',(-0.0122136945132895,-0.0357843850885679,
-0.0134403537416257));
#27598=CARTESIAN_POINT('Ctrl Pts',(-0.0119267613588196,-0.0358024413865726,
-0.0133388630106222));
#27599=CARTESIAN_POINT('Ctrl Pts',(-0.0117039532486444,-0.0358204976845775,
-0.013158334746768));
#27600=CARTESIAN_POINT('Ctrl Pts',(-0.0116697236133939,-0.0358232716432731,
-0.0131306004932021));
#27601=CARTESIAN_POINT('Ctrl Pts',(-0.0116369677265673,-0.0358260456019688,
-0.0131010939841645));
#27602=CARTESIAN_POINT('Ctrl Pts',(-0.0116058646046839,-0.0358288195606644,
-0.0130699909408613));
#27603=CARTESIAN_POINT('Ctrl Pts',(-0.0114034456603145,-0.03584687246844,
-0.0128675725078917));
#27604=CARTESIAN_POINT('Ctrl Pts',(-0.0112723314625597,-0.0358649253762156,
-0.0125929713762996));
#27605=CARTESIAN_POINT('Ctrl Pts',(-0.0112424068074952,-0.0358829782839913,
-0.0123078366649266));
#27606=CARTESIAN_POINT('Ctrl Pts',(-0.0112378030500505,-0.0358857556329161,
-0.0122639701258676));
#27607=CARTESIAN_POINT('Ctrl Pts',(-0.011235500041264,-0.035888532981841,
-0.012219892132267));
#27608=CARTESIAN_POINT('Ctrl Pts',(-0.0112355000000006,-0.0358913103307658,
-0.0121758544713988));
#27609=CARTESIAN_POINT('Ctrl Pts',(-0.0112354997317862,-0.0359093632385414,
-0.0118896074596547));
#27610=CARTESIAN_POINT('Ctrl Pts',(-0.0113369499668099,-0.035927416146317,
-0.0116027224208943));
#27611=CARTESIAN_POINT('Ctrl Pts',(-0.0115174171538356,-0.0359454690540927,
-0.0113799316821124));
#27612=CARTESIAN_POINT('Ctrl Pts',(-0.0115451811215069,-0.0359482464030175,
-0.0113456564491964));
#27613=CARTESIAN_POINT('Ctrl Pts',(-0.0115747218524613,-0.0359510237519424,
-0.0113128584225173));
#27614=CARTESIAN_POINT('Ctrl Pts',(-0.0116058629290656,-0.0359538011008673,
-0.0112817173078721));
#27615=CARTESIAN_POINT('Ctrl Pts',(-0.01180831950711,-0.0359718573988721,
-0.011079260482513));
#27616=CARTESIAN_POINT('Ctrl Pts',(-0.0120829807049326,-0.035989913696877,
-0.0109481379037549));
#27617=CARTESIAN_POINT('Ctrl Pts',(-0.0123681757652149,-0.0360079699948819,
-0.0109182434022445));
#27618=CARTESIAN_POINT('Ctrl Pts',(-0.0124119898026876,-0.0360107439535774,
-0.0109136507602537));
#27619=CARTESIAN_POINT('Ctrl Pts',(-0.0124560147009807,-0.036013517912273,
-0.0109113532990747));
#27620=CARTESIAN_POINT('Ctrl Pts',(-0.0124999996401681,-0.0360162918709686,
-0.0109113532865581));
#27621=CARTESIAN_POINT('Ctrl Pts',(-0.0127852519847615,-0.036034281624651,
-0.0109113532053854));
#27622=CARTESIAN_POINT('Ctrl Pts',(-0.0130712339615104,-0.0360522713783335,
-0.0110121319488751));
#27623=CARTESIAN_POINT('Ctrl Pts',(-0.0132936186122632,-0.0360702611320159,
-0.0111914094088944));
#27624=CARTESIAN_POINT('Ctrl Pts',(-0.0133287321709466,-0.0360731016350339,
-0.0112197165316733));
#27625=CARTESIAN_POINT('Ctrl Pts',(-0.0133623021715428,-0.036075942138052,
-0.011249882405828));
#27626=CARTESIAN_POINT('Ctrl Pts',(-0.0133941365620555,-0.03607878264107,
-0.0112817167989928));
#27627=CARTESIAN_POINT('Ctrl Pts',(-0.0135995382522714,-0.0360971101199873,
-0.0114871185063207));
#27628=CARTESIAN_POINT('Ctrl Pts',(-0.0137314030973446,-0.0361154375989046,
-0.011766542477848));
#27629=CARTESIAN_POINT('Ctrl Pts',(-0.013758870797837,-0.036133765077822,
-0.0120566703836178));
#27630=CARTESIAN_POINT('Ctrl Pts',(-0.0137626217529387,-0.0361362678556051,
-0.0120962898904854));
#27631=CARTESIAN_POINT('Ctrl Pts',(-0.0137645000146323,-0.0361387706333883,
-0.0121360782826731));
#27632=CARTESIAN_POINT('Ctrl Pts',(-0.0137644999999999,-0.0361412734111714,
-0.0121758537517351));
#27633=CARTESIAN_POINT('Origin',(0.006,-0.0412787743898723,-0.0121758532865581));
#27634=CARTESIAN_POINT('Ctrl Pts',(0.0047355001379818,-0.040342276368498,
-0.0121764440115014));
#27635=CARTESIAN_POINT('Ctrl Pts',(0.00473549271943105,-0.0403412424985884,
-0.0121605639364976));
#27636=CARTESIAN_POINT('Ctrl Pts',(0.00473578444258578,-0.0403402172682197,
-0.0121446845106245));
#27637=CARTESIAN_POINT('Ctrl Pts',(0.0047369331751707,-0.0403382411308512,
-0.0121138258203437));
#27638=CARTESIAN_POINT('Ctrl Pts',(0.00473775776908206,-0.0403372894215712,
-0.0120988481449022));
#27639=CARTESIAN_POINT('Ctrl Pts',(0.00473986108795072,-0.0403354700358818,
-0.0120700045674296));
#27640=CARTESIAN_POINT('Ctrl Pts',(0.00474110272091954,-0.0403346013649773,
-0.0120561382338009));
#27641=CARTESIAN_POINT('Ctrl Pts',(0.00474452974249035,-0.0403325926739768,
-0.0120238735032967));
#27642=CARTESIAN_POINT('Ctrl Pts',(0.00474689101229707,-0.0403314581869107,
-0.0120054967770707));
#27643=CARTESIAN_POINT('Ctrl Pts',(0.00475602882948269,-0.0403277450889632,
-0.0119449408307062));
#27644=CARTESIAN_POINT('Ctrl Pts',(0.00476453872318097,-0.0403252185090613,
-0.0119030516012084));
#27645=CARTESIAN_POINT('Ctrl Pts',(0.00478729586255755,-0.0403198814868954,
-0.0118143325619181));
#27646=CARTESIAN_POINT('Ctrl Pts',(0.00480217272520959,-0.0403170874643592,
-0.0117677374022093));
#27647=CARTESIAN_POINT('Ctrl Pts',(0.004836235694752,-0.0403116415692896,
-0.0116791298839421));
#27648=CARTESIAN_POINT('Ctrl Pts',(0.00485509760512865,-0.0403089944262697,
-0.0116370773149042));
#27649=CARTESIAN_POINT('Ctrl Pts',(0.00488480398366416,-0.0403051653446008,
-0.0115794897132839));
#27650=CARTESIAN_POINT('Ctrl Pts',(0.00489376706054111,-0.0403040456476962,
-0.0115630235509855));
#27651=CARTESIAN_POINT('Ctrl Pts',(0.00491040869319124,-0.0403020170262455,
-0.0115340064952627));
#27652=CARTESIAN_POINT('Ctrl Pts',(0.00491794662652621,-0.0403011148206083,
-0.0115213787076834));
#27653=CARTESIAN_POINT('Ctrl Pts',(0.00493033822018665,-0.0402996528403234,
-0.0115014193281616));
#27654=CARTESIAN_POINT('Ctrl Pts',(0.0049350513299327,-0.0402991013752712,
-0.0114940015369747));
#27655=CARTESIAN_POINT('Ctrl Pts',(0.00494469910014684,-0.0402979803582356,
-0.011479161320187));
#27656=CARTESIAN_POINT('Ctrl Pts',(0.00494963566221157,-0.0402974107182029,
-0.011471740772816));
#27657=CARTESIAN_POINT('Ctrl Pts',(0.00496327391120557,-0.0402958489017943,
-0.0114517026232173));
#27658=CARTESIAN_POINT('Ctrl Pts',(0.0049721269766726,-0.0402948478511739,
-0.0114391904285324));
#27659=CARTESIAN_POINT('Ctrl Pts',(0.00502133612707275,-0.0402893640310613,
-0.0113722567160644));
#27660=CARTESIAN_POINT('Ctrl Pts',(0.00506578674114777,-0.0402846996568197,
-0.0113209879373225));
#27661=CARTESIAN_POINT('Ctrl Pts',(0.00515330688422206,-0.0402762854850955,
-0.0112350632685026));
#27662=CARTESIAN_POINT('Ctrl Pts',(0.00519495448414556,-0.0402725374139024,
-0.0111991866755963));
#27663=CARTESIAN_POINT('Ctrl Pts',(0.00525914395718843,-0.0402671742323331,
-0.0111507965466428));
#27664=CARTESIAN_POINT('Ctrl Pts',(0.00527994217087957,-0.0402654935732286,
-0.0111360812655809));
#27665=CARTESIAN_POINT('Ctrl Pts',(0.00531924561335684,-0.0402624222863743,
-0.0111100183937852));
#27666=CARTESIAN_POINT('Ctrl Pts',(0.0053376255429344,-0.0402610261596243,
-0.0110984997120659));
#27667=CARTESIAN_POINT('Ctrl Pts',(0.00536915088632124,-0.0402586968112379,
-0.0110798547561693));
#27668=CARTESIAN_POINT('Ctrl Pts',(0.00538214231516302,-0.0402577549323554,
-0.0110724787832965));
#27669=CARTESIAN_POINT('Ctrl Pts',(0.00540719955890394,-0.0402559712545489,
-0.0110588337452892));
#27670=CARTESIAN_POINT('Ctrl Pts',(0.00541924165519825,-0.0402551281995443,
-0.0110525257360996));
#27671=CARTESIAN_POINT('Ctrl Pts',(0.00545158747941527,-0.0402528994045979,
-0.0110362412378471));
#27672=CARTESIAN_POINT('Ctrl Pts',(0.00547206159725739,-0.0402515255059595,
-0.0110266130809181));
#27673=CARTESIAN_POINT('Ctrl Pts',(0.00557222838599391,-0.040244960657379,
-0.0109827508947513));
#27674=CARTESIAN_POINT('Ctrl Pts',(0.00565504138380275,-0.0402400234900514,
-0.0109562275729702));
#27675=CARTESIAN_POINT('Ctrl Pts',(0.00578220288660786,-0.0402325642945694,
-0.0109295021139085));
#27676=CARTESIAN_POINT('Ctrl Pts',(0.00582490850553635,-0.0402300747754092,
-0.0109227892860348));
#27677=CARTESIAN_POINT('Ctrl Pts',(0.00588587353753644,-0.0402264467684285,
-0.0109163839295228));
#27678=CARTESIAN_POINT('Ctrl Pts',(0.00590391357925132,-0.0402253639854568,
-0.0109148793571764));
#27679=CARTESIAN_POINT('Ctrl Pts',(0.00593628266020448,-0.0402233950372136,
-0.0109128783336088));
#27680=CARTESIAN_POINT('Ctrl Pts',(0.00595059980214547,-0.0402225150214586,
-0.0109122373589607));
#27681=CARTESIAN_POINT('Ctrl Pts',(0.00597363092048177,-0.04022108035792,
-0.010911598253091));
#27682=CARTESIAN_POINT('Ctrl Pts',(0.00598233984228549,-0.0402205334828755,
-0.0109114466155501));
#27683=CARTESIAN_POINT('Ctrl Pts',(0.00600004443411616,-0.0402194116056112,
-0.0109113212932764));
#27684=CARTESIAN_POINT('Ctrl Pts',(0.00600903953982635,-0.040218836361299,
-0.010911353607111));
#27685=CARTESIAN_POINT('Ctrl Pts',(0.00603377225323582,-0.0402172416144852,
-0.0109117063596917));
#27686=CARTESIAN_POINT('Ctrl Pts',(0.00604950493082304,-0.0402162126347371,
-0.0109122246907602));
#27687=CARTESIAN_POINT('Ctrl Pts',(0.0061458423710201,-0.0402098384888006,
-0.0109172004050394));
#27688=CARTESIAN_POINT('Ctrl Pts',(0.00622587325787001,-0.0402042417685395,
-0.0109290745724271));
#27689=CARTESIAN_POINT('Ctrl Pts',(0.0063665197513422,-0.0401943307249478,
-0.01096393621316));
#27690=CARTESIAN_POINT('Ctrl Pts',(0.0064275580821258,-0.0401900001654303,
-0.0109841000941119));
#27691=CARTESIAN_POINT('Ctrl Pts',(0.00650790904439407,-0.0401843154598997,
-0.0110176169562622));
#27692=CARTESIAN_POINT('Ctrl Pts',(0.00652876882235517,-0.040182840398907,
-0.0110269900943405));
#27693=CARTESIAN_POINT('Ctrl Pts',(0.0065630017512803,-0.0401804195353464,
-0.0110435023973629));
#27694=CARTESIAN_POINT('Ctrl Pts',(0.00657652061754807,-0.0401794634479277,
-0.0110503251805717));
#27695=CARTESIAN_POINT('Ctrl Pts',(0.00660333125990088,-0.0401775660167492,
-0.0110644659833282));
#27696=CARTESIAN_POINT('Ctrl Pts',(0.00661662035832072,-0.0401766248599926,
-0.011071783673063));
#27697=CARTESIAN_POINT('Ctrl Pts',(0.00664973530513637,-0.0401742757247778,
-0.0110908030019563));
#27698=CARTESIAN_POINT('Ctrl Pts',(0.00666937967289366,-0.0401728786595907,
-0.0111028103992557));
#27699=CARTESIAN_POINT('Ctrl Pts',(0.00675741459774797,-0.0401665822612498,
-0.011159979789202));
#27700=CARTESIAN_POINT('Ctrl Pts',(0.00682164282701327,-0.0401619034134789,
-0.0112111873792264));
#27701=CARTESIAN_POINT('Ctrl Pts',(0.00691338440002574,-0.0401545712312639,
-0.0113001864769143));
#27702=CARTESIAN_POINT('Ctrl Pts',(0.00694453757430276,-0.0401519351448475,
-0.0113338843193444));
#27703=CARTESIAN_POINT('Ctrl Pts',(0.00698572010051996,-0.0401481201158153,
-0.0113835996129995));
#27704=CARTESIAN_POINT('Ctrl Pts',(0.00699732879665733,-0.0401470030138161,
-0.0113982639307353));
#27705=CARTESIAN_POINT('Ctrl Pts',(0.00701746110916463,-0.0401449786394995,
-0.011424888161371));
#27706=CARTESIAN_POINT('Ctrl Pts',(0.00702610975923346,-0.0401440780522466,
-0.0114367494723579));
#27707=CARTESIAN_POINT('Ctrl Pts',(0.00703959790356993,-0.0401426182624365,
-0.011455941117517));
#27708=CARTESIAN_POINT('Ctrl Pts',(0.00704457116197873,-0.0401420673383676,
-0.0114631763534981));
#27709=CARTESIAN_POINT('Ctrl Pts',(0.0070544414291497,-0.0401409467378313,
-0.0114778611724585));
#27710=CARTESIAN_POINT('Ctrl Pts',(0.00705933577515871,-0.0401403769648988,
-0.0114853118879558));
#27711=CARTESIAN_POINT('Ctrl Pts',(0.00707243634367353,-0.0401388142200958,
-0.0115057220887536));
#27712=CARTESIAN_POINT('Ctrl Pts',(0.00708048594282326,-0.0401378123555242,
-0.0115187797649281));
#27713=CARTESIAN_POINT('Ctrl Pts',(0.00711409794524443,-0.0401334548791656,
-0.0115755918612047));
#27714=CARTESIAN_POINT('Ctrl Pts',(0.00713725348116252,-0.0401299997159101,
-0.0116207121017299));
#27715=CARTESIAN_POINT('Ctrl Pts',(0.00717947034994673,-0.0401228062373415,
-0.01171677327409));
#27716=CARTESIAN_POINT('Ctrl Pts',(0.00719808325444494,-0.0401190732544188,
-0.0117678070107088));
#27717=CARTESIAN_POINT('Ctrl Pts',(0.00722722024219893,-0.0401120758577486,
-0.011867122544748));
#27718=CARTESIAN_POINT('Ctrl Pts',(0.00723831046276647,-0.0401088055543218,
-0.0119151382140673));
#27719=CARTESIAN_POINT('Ctrl Pts',(0.00724978609844917,-0.0401043799255059,
-0.0119825616146551));
#27720=CARTESIAN_POINT('Ctrl Pts',(0.00725257010034125,-0.0401031536918412,
-0.0120015111804207));
#27721=CARTESIAN_POINT('Ctrl Pts',(0.00725671266056455,-0.0401010176302278,
-0.0120349779954311));
#27722=CARTESIAN_POINT('Ctrl Pts',(0.00725825257418958,-0.0401001024217962,
-0.0120494687684206));
#27723=CARTESIAN_POINT('Ctrl Pts',(0.00726098865407339,-0.0400981760496522,
-0.0120802742635309));
#27724=CARTESIAN_POINT('Ctrl Pts',(0.00726211942864145,-0.0400971670422458,
-0.0120965921922759));
#27725=CARTESIAN_POINT('Ctrl Pts',(0.00726435918403415,-0.0400944154724462,
-0.0121415449430569));
#27726=CARTESIAN_POINT('Ctrl Pts',(0.00726481202684669,-0.0400926927167552,
-0.0121702033736002));
#27727=CARTESIAN_POINT('Ctrl Pts',(0.00726243583940873,-0.0400849427395138,
-0.0123008158959845));
#27728=CARTESIAN_POINT('Ctrl Pts',(0.00724825423884516,-0.0400792444492893,
-0.0124021729668372));
#27729=CARTESIAN_POINT('Ctrl Pts',(0.00721527190557364,-0.0400717691464125,
-0.0125262409220381));
#27730=CARTESIAN_POINT('Ctrl Pts',(0.00720769174409166,-0.0400702154599285,
-0.012551536403038));
#27731=CARTESIAN_POINT('Ctrl Pts',(0.00719337014596564,-0.0400675037772246,
-0.0125943997583817));
#27732=CARTESIAN_POINT('Ctrl Pts',(0.00718701807920654,-0.0400663610634193,
-0.0126120888342709));
#27733=CARTESIAN_POINT('Ctrl Pts',(0.00717683320091959,-0.0400646045656637,
-0.0126385798058883));
#27734=CARTESIAN_POINT('Ctrl Pts',(0.00717329023461174,-0.0400640058384437,
-0.0126474910993906));
#27735=CARTESIAN_POINT('Ctrl Pts',(0.007166456822607,-0.0400628719191018,
-0.012664124916019));
#27736=CARTESIAN_POINT('Ctrl Pts',(0.00716319026798234,-0.0400623380319494,
-0.012671856399086));
#27737=CARTESIAN_POINT('Ctrl Pts',(0.00715484355182419,-0.040060994424708,
-0.0126910759576779));
#27738=CARTESIAN_POINT('Ctrl Pts',(0.00714966880082104,-0.0400601795575952,
-0.0127025217310663));
#27739=CARTESIAN_POINT('Ctrl Pts',(0.00712695889102837,-0.0400566836118754,
-0.0127508225356729));
#27740=CARTESIAN_POINT('Ctrl Pts',(0.00710781655954294,-0.0400539304569279,
-0.0127868916479098));
#27741=CARTESIAN_POINT('Ctrl Pts',(0.00703609736103444,-0.0400443593058478,
-0.0129075454907999));
#27742=CARTESIAN_POINT('Ctrl Pts',(0.00697529151291681,-0.0400374606480069,
-0.012986829619674));
#27743=CARTESIAN_POINT('Ctrl Pts',(0.0068858809777128,-0.0400290046129356,
-0.0130786217716277));
#27744=CARTESIAN_POINT('Ctrl Pts',(0.0068652630524394,-0.0400271460533999,
-0.0130984019844701));
#27745=CARTESIAN_POINT('Ctrl Pts',(0.00683193544471295,-0.0400242792359711,
-0.0131282742994764));
#27746=CARTESIAN_POINT('Ctrl Pts',(0.00681967256508146,-0.0400232516384117,
-0.0131388482475118));
#27747=CARTESIAN_POINT('Ctrl Pts',(0.00679596562509729,-0.0400213148444947,
-0.0131585090514449));
#27748=CARTESIAN_POINT('Ctrl Pts',(0.00678456063817248,-0.0400204040437298,
-0.0131676386773921));
#27749=CARTESIAN_POINT('Ctrl Pts',(0.00675785794922321,-0.0400183176685875,
-0.0131882650847784));
#27750=CARTESIAN_POINT('Ctrl Pts',(0.00674245219865486,-0.0400171477600379,
-0.0131996164972148));
#27751=CARTESIAN_POINT('Ctrl Pts',(0.00668813968113017,-0.0400131309187555,
-0.0132377644511274));
#27752=CARTESIAN_POINT('Ctrl Pts',(0.00664799219032947,-0.0400103494101557,
-0.0132627287563542));
#27753=CARTESIAN_POINT('Ctrl Pts',(0.00651827557113986,-0.0400017710078011,
-0.0133336395802402));
#27754=CARTESIAN_POINT('Ctrl Pts',(0.00642458109009128,-0.0399961688950079,
-0.013371179821941));
#27755=CARTESIAN_POINT('Ctrl Pts',(0.00630922579312222,-0.039989003941938,
-0.0134021058327556));
#27756=CARTESIAN_POINT('Ctrl Pts',(0.00629090447206087,-0.039987857430459,
-0.0134065808781319));
#27757=CARTESIAN_POINT('Ctrl Pts',(0.00626311524426538,-0.0399860963314647,
-0.0134127133450927));
#27758=CARTESIAN_POINT('Ctrl Pts',(0.00625371654119853,-0.0399854969227135,
-0.0134146754446956));
#27759=CARTESIAN_POINT('Ctrl Pts',(0.00623606578631421,-0.0399843626299647,
-0.0134181509844042));
#27760=CARTESIAN_POINT('Ctrl Pts',(0.00622781950864395,-0.0399838290695727,
-0.0134196896427894));
#27761=CARTESIAN_POINT('Ctrl Pts',(0.00620721657688126,-0.0399824876598383,
-0.013423322166915));
#27762=CARTESIAN_POINT('Ctrl Pts',(0.00619484316552589,-0.0399816746997847,
-0.0134253145425432));
#27763=CARTESIAN_POINT('Ctrl Pts',(0.0061424087369798,-0.0399782042462449,
-0.013432959804256));
#27764=CARTESIAN_POINT('Ctrl Pts',(0.00610212090450855,-0.0399754759248984,
-0.0134368718456499));
#27765=CARTESIAN_POINT('Ctrl Pts',(0.00598405628191336,-0.0399674172022816,
-0.0134426413127285));
#27766=CARTESIAN_POINT('Ctrl Pts',(0.0059062028711642,-0.0399620346527578,
-0.013439265177324));
#27767=CARTESIAN_POINT('Ctrl Pts',(0.00579953294236739,-0.0399547953882157,
-0.0134247194921208));
#27768=CARTESIAN_POINT('Ctrl Pts',(0.00577006500849551,-0.039952808313091,
-0.0134196313816113));
#27769=CARTESIAN_POINT('Ctrl Pts',(0.00571697847431758,-0.0399492560618952,
-0.0134085136556847));
#27770=CARTESIAN_POINT('Ctrl Pts',(0.00569330146227426,-0.0399476817606314,
-0.0134028369481928));
#27771=CARTESIAN_POINT('Ctrl Pts',(0.0056549252033243,-0.0399451452244423,
-0.0133924555803342));
#27772=CARTESIAN_POINT('Ctrl Pts',(0.00564012298897309,-0.0399441705532669,
-0.0133881594883199));
#27773=CARTESIAN_POINT('Ctrl Pts',(0.00561129287905744,-0.0399422783234251,
-0.0133792174278886));
#27774=CARTESIAN_POINT('Ctrl Pts',(0.00559726062251742,-0.0399413602208137,
-0.0133745940862731));
#27775=CARTESIAN_POINT('Ctrl Pts',(0.00556292993124942,-0.0399391192669821,
-0.0133626119165037));
#27776=CARTESIAN_POINT('Ctrl Pts',(0.00554273242799329,-0.0399378054813009,
-0.0133549770036265));
#27777=CARTESIAN_POINT('Ctrl Pts',(0.00543462590048533,-0.0399307805007482,
-0.0133109154432584));
#27778=CARTESIAN_POINT('Ctrl Pts',(0.00535084788926817,-0.0399253903871653,
-0.0132651727866826));
#27779=CARTESIAN_POINT('Ctrl Pts',(0.00524098846071442,-0.0399176686138853,
-0.0131879755351449));
#27780=CARTESIAN_POINT('Ctrl Pts',(0.00521004976903454,-0.039915405479245,
-0.0131640173708914));
#27781=CARTESIAN_POINT('Ctrl Pts',(0.00516172695295846,-0.039911639677013,
-0.0131228758919729));
#27782=CARTESIAN_POINT('Ctrl Pts',(0.00514364238231976,-0.0399101728170191,
-0.0131065546277538));
#27783=CARTESIAN_POINT('Ctrl Pts',(0.00511843279369019,-0.039908024690825,
-0.0130824460027521));
#27784=CARTESIAN_POINT('Ctrl Pts',(0.00511091542744187,-0.0399073702699722,
-0.0130750750045097));
#27785=CARTESIAN_POINT('Ctrl Pts',(0.00509768393009534,-0.0399061914819535,
-0.0130617730180069));
#27786=CARTESIAN_POINT('Ctrl Pts',(0.00509193427140479,-0.0399056697642076,
-0.0130558786739378));
#27787=CARTESIAN_POINT('Ctrl Pts',(0.00507873376660814,-0.0399044497631946,
-0.0130420788784797));
#27788=CARTESIAN_POINT('Ctrl Pts',(0.00507132675034842,-0.039903748547216,
-0.0130341330925903));
#27789=CARTESIAN_POINT('Ctrl Pts',(0.00504738415814247,-0.0399014294509445,
-0.0130077761693709));
#27790=CARTESIAN_POINT('Ctrl Pts',(0.00503128737206398,-0.0398997861222379,
-0.0129889758497332));
#27791=CARTESIAN_POINT('Ctrl Pts',(0.00495740729654985,-0.0398918758387407,
-0.0128973779929062));
#27792=CARTESIAN_POINT('Ctrl Pts',(0.00490721296573304,-0.039885396782596,
-0.0128188271002635));
#27793=CARTESIAN_POINT('Ctrl Pts',(0.00485197528692502,-0.0398769790983398,
-0.0127069041849032));
#27794=CARTESIAN_POINT('Ctrl Pts',(0.00483895619389082,-0.0398748546039561,
-0.0126778028119593));
#27795=CARTESIAN_POINT('Ctrl Pts',(0.0048175340927321,-0.0398710908308532,
-0.012624610959997));
#27796=CARTESIAN_POINT('Ctrl Pts',(0.00480873401065512,-0.0398694405380058,
-0.0126006998018542));
#27797=CARTESIAN_POINT('Ctrl Pts',(0.00479571193713884,-0.0398668154278319,
-0.0125617218165928));
#27798=CARTESIAN_POINT('Ctrl Pts',(0.00479103692849374,-0.0398658264381139,
-0.0125468149925733));
#27799=CARTESIAN_POINT('Ctrl Pts',(0.00478251409657398,-0.0398639267311554,
-0.0125177641570955));
#27800=CARTESIAN_POINT('Ctrl Pts',(0.00477863361939101,-0.0398630151078194,
-0.0125036324205847));
#27801=CARTESIAN_POINT('Ctrl Pts',(0.00476983207840232,-0.0398608253939452,
-0.0124692494871266));
#27802=CARTESIAN_POINT('Ctrl Pts',(0.00476516418664008,-0.0398595553602545,
-0.0124489375850342));
#27803=CARTESIAN_POINT('Ctrl Pts',(0.0047440354368581,-0.0398531807795075,
-0.0123453281619604));
#27804=CARTESIAN_POINT('Ctrl Pts',(0.00473550000701352,-0.0398483286333551,
-0.0122606813520481));
#27805=CARTESIAN_POINT('Ctrl Pts',(0.0047355,-0.0398434635507866,-0.0121758533911061));
#27806=CARTESIAN_POINT('Ctrl Pts',(0.00473550000001467,-0.0399058329518585,
-0.0121758593776931));
#27807=CARTESIAN_POINT('Ctrl Pts',(0.00473550140307262,-0.0399241615430135,
-0.0124671296870887));
#27808=CARTESIAN_POINT('Ctrl Pts',(0.00484035537256781,-0.0399424901341685,
-0.0127578883555264));
#27809=CARTESIAN_POINT('Ctrl Pts',(0.00502575436044838,-0.0399608187253235,
-0.0129819585425977));
#27810=CARTESIAN_POINT('Ctrl Pts',(0.00505106586813013,-0.0399633210274187,
-0.0130125496171561));
#27811=CARTESIAN_POINT('Ctrl Pts',(0.00507780576562169,-0.0399658233295138,
-0.0130419311106039));
#27812=CARTESIAN_POINT('Ctrl Pts',(0.00510584767754908,-0.039968325631609,
-0.0130699740134488));
#27813=CARTESIAN_POINT('Ctrl Pts',(0.00530746131447154,-0.039986316495691,
-0.013271594774796));
#27814=CARTESIAN_POINT('Ctrl Pts',(0.00558088995559621,-0.040004307359773,
-0.0134026189102355));
#27815=CARTESIAN_POINT('Ctrl Pts',(0.00586499593047847,-0.0400222982238551,
-0.013433125791313));
#27816=CARTESIAN_POINT('Ctrl Pts',(0.00590984476329907,-0.0400251382530232,
-0.0134379415929162));
#27817=CARTESIAN_POINT('Ctrl Pts',(0.00595491931973503,-0.0400279782821913,
-0.0134403514774338));
#27818=CARTESIAN_POINT('Ctrl Pts',(0.00599994922599528,-0.0400308183113595,
-0.0134403532855387));
#27819=CARTESIAN_POINT('Ctrl Pts',(0.0062862573739437,-0.0400488757216182,
-0.0134403647817912));
#27820=CARTESIAN_POINT('Ctrl Pts',(0.00657319492440129,-0.0400669331318769,
-0.0133388846850336));
#27821=CARTESIAN_POINT('Ctrl Pts',(0.00679601016042393,-0.0400849905421356,
-0.013158364393112));
#27822=CARTESIAN_POINT('Ctrl Pts',(0.00683023291210797,-0.0400877640251271,
-0.013130637828113));
#27823=CARTESIAN_POINT('Ctrl Pts',(0.0068629826641763,-0.0400905375081185,
-0.0131011397728834));
#27824=CARTESIAN_POINT('Ctrl Pts',(0.00689408051555027,-0.0400933109911099,
-0.0130700458171204));
#27825=CARTESIAN_POINT('Ctrl Pts',(0.00709651233115139,-0.0401113650100434,
-0.0128676393600427));
#27826=CARTESIAN_POINT('Ctrl Pts',(0.00722764341798178,-0.0401294190289768,
-0.0125930456480888));
#27827=CARTESIAN_POINT('Ctrl Pts',(0.00725758525939554,-0.0401474730479103,
-0.0123079122330595));
#27828=CARTESIAN_POINT('Ctrl Pts',(0.00726219059024867,-0.040150249922227,
-0.0122640560888983));
#27829=CARTESIAN_POINT('Ctrl Pts',(0.00726449624762511,-0.0401530267965437,
-0.0122199884489719));
#27830=CARTESIAN_POINT('Ctrl Pts',(0.00726449999541867,-0.0401558036708604,
-0.0121759609257025));
#27831=CARTESIAN_POINT('Ctrl Pts',(0.00726452436192866,-0.040173857689794,
-0.0118897132788708));
#27832=CARTESIAN_POINT('Ctrl Pts',(0.00716309785865325,-0.0401919117087277,
-0.0116028192306949));
#27833=CARTESIAN_POINT('Ctrl Pts',(0.00698264882413635,-0.0402099657276614,
-0.0113800131402828));
#27834=CARTESIAN_POINT('Ctrl Pts',(0.00695489410142147,-0.0402127426019779,
-0.011345743512434));
#27835=CARTESIAN_POINT('Ctrl Pts',(0.0069253633130834,-0.0402155194762944,
-0.0113129502609626));
#27836=CARTESIAN_POINT('Ctrl Pts',(0.00689423273686524,-0.0402182963506109,
-0.0112818129841564));
#27837=CARTESIAN_POINT('Ctrl Pts',(0.00669179736447306,-0.0402363537608694,
-0.0110793340392964));
#27838=CARTESIAN_POINT('Ctrl Pts',(0.00641714955401632,-0.0402544111711278,
-0.0109481820350889));
#27839=CARTESIAN_POINT('Ctrl Pts',(0.00613195713696627,-0.0402724685813862,
-0.0109182573403164));
#27840=CARTESIAN_POINT('Ctrl Pts',(0.00608815371738732,-0.0402752420643779,
-0.0109136611312921));
#27841=CARTESIAN_POINT('Ctrl Pts',(0.00604413929143607,-0.0402780155473697,
-0.0109113590181293));
#27842=CARTESIAN_POINT('Ctrl Pts',(0.00600016450428374,-0.0402807890303614,
-0.0109113532972586));
#27843=CARTESIAN_POINT('Ctrl Pts',(0.00571491147729529,-0.0402987798944434,
-0.0109113161874561));
#27844=CARTESIAN_POINT('Ctrl Pts',(0.00542891591239803,-0.0403167707585254,
-0.0110120582582409));
#27845=CARTESIAN_POINT('Ctrl Pts',(0.00520650781506261,-0.0403347616226074,
-0.0111913075017196));
#27846=CARTESIAN_POINT('Ctrl Pts',(0.00517139857957576,-0.0403376016517755,
-0.0112196037012534));
#27847=CARTESIAN_POINT('Ctrl Pts',(0.00513783196264546,-0.0403404416809437,
-0.0112497580074664));
#27848=CARTESIAN_POINT('Ctrl Pts',(0.00510599991255491,-0.0403432817101119,
-0.0112815803451984));
#27849=CARTESIAN_POINT('Ctrl Pts',(0.00490056658874369,-0.0403616103012668,
-0.0114869509887204));
#27850=CARTESIAN_POINT('Ctrl Pts',(0.00476865909976607,-0.0403799388924218,
-0.011766355214167));
#27851=CARTESIAN_POINT('Ctrl Pts',(0.00474114731563261,-0.0403982674835768,
-0.0120564792145784));
#27852=CARTESIAN_POINT('Ctrl Pts',(0.00473739128253129,-0.040400769785672,
-0.0120960882542447));
#27853=CARTESIAN_POINT('Ctrl Pts',(0.00473550698092259,-0.0404032720877671,
-0.012135866378795));
#27854=CARTESIAN_POINT('Ctrl Pts',(0.004735500019377,-0.0404057743898623,
-0.0121756319171353));
#27855=CARTESIAN_POINT('Origin',(-0.015,-0.0412787743898723,-0.0201758532865581));
#27856=CARTESIAN_POINT('',(-0.015,-0.0379787743898623,-0.00457585328655813));
#27857=CARTESIAN_POINT('',(-0.0149999999999975,-0.0408787743898673,-0.00457585328656563));
#27858=CARTESIAN_POINT('',(-0.015,-0.0412787743898723,-0.00457585328656813));
#27859=CARTESIAN_POINT('',(-0.015,-0.0379787743898723,-0.0197758532865581));
#27860=CARTESIAN_POINT('',(-0.015,-0.0379787743898623,-0.0121758532865681));
#27861=CARTESIAN_POINT('',(-0.015,-0.0408787743898723,-0.0197758532865581));
#27862=CARTESIAN_POINT('',(-0.015,-0.0412787743898723,-0.0197758532865681));
#27863=CARTESIAN_POINT('',(-0.015,-0.0408787743898623,-0.0161758532865681));
#27864=CARTESIAN_POINT('Origin',(-0.0148,-0.0410787743898723,-0.0161758532865581));
#27865=CARTESIAN_POINT('',(-0.0145999999999925,-0.0412787743898673,-0.00457585328656563));
#27866=CARTESIAN_POINT('',(-0.01459999999999,-0.0412787743898723,-0.00457585328656813));
#27867=CARTESIAN_POINT('',(-0.0146,-0.0412787743898723,-0.0197758532865581));
#27868=CARTESIAN_POINT('',(-0.015,-0.0408787743898623,-0.0197758532865681));
#27869=CARTESIAN_POINT('',(-0.01459999999999,-0.0412787743898723,-0.0161758532865681));
#27870=CARTESIAN_POINT('Origin',(-0.0148,-0.0412787743898723,-0.0199758532865582));
#27871=CARTESIAN_POINT('',(-0.0146,-0.0379787743898723,-0.0201758532865581));
#27872=CARTESIAN_POINT('',(-0.0174042976073008,-0.0379787743898623,-0.0173715556792775));
#27873=CARTESIAN_POINT('',(-0.0146,-0.0408787743898723,-0.0201758532865581));
#27874=CARTESIAN_POINT('',(-0.01459999999999,-0.0412787743898723,-0.0201758532865681));
#27875=CARTESIAN_POINT('',(-0.01459999999999,-0.0408787743898623,-0.0201758532865681));
#27876=CARTESIAN_POINT('Origin',(-0.00941719042916296,-0.0379787743898723,
-0.00417585328655812));
#27877=CARTESIAN_POINT('',(-0.00982716095192005,-0.0379787743898677,-0.0201758532865654));
#27878=CARTESIAN_POINT('',(-0.00941719042915764,-0.0379787743898678,-0.0197758532865628));
#27879=CARTESIAN_POINT('Ctrl Pts',(-0.00941719042916247,-0.0379787743898723,
-0.0197758532865577));
#27880=CARTESIAN_POINT('Ctrl Pts',(-0.00960936411170753,-0.0379787743898723,
-0.0199627223623769));
#27881=CARTESIAN_POINT('Ctrl Pts',(-0.00982716095192546,-0.0379787743898723,
-0.0201758532865608));
#27882=CARTESIAN_POINT('',(-0.000708595214571501,-0.0379787743898623,-0.0201758532865681));
#27883=CARTESIAN_POINT('',(-0.0145999999999967,-0.0379787743898656,-0.00417585328655812));
#27884=CARTESIAN_POINT('',(-0.0134042976072807,-0.0379787743898623,-0.00298015089383886));
#27885=CARTESIAN_POINT('',(-0.00982716095192005,-0.0379787743898677,-0.00417585328655585));
#27886=CARTESIAN_POINT('',(-0.0122085952145715,-0.0379787743898623,-0.00417585328655812));
#27887=CARTESIAN_POINT('',(-0.00941719042915521,-0.0379787743898672,-0.00457585328656588));
#27888=CARTESIAN_POINT('Ctrl Pts',(-0.00982716095192254,-0.0379787743898723,
-0.0041758532865584));
#27889=CARTESIAN_POINT('Ctrl Pts',(-0.00960936411170209,-0.0379787743898723,
-0.00438898421074477));
#27890=CARTESIAN_POINT('Ctrl Pts',(-0.0094171904291551,-0.0379787743898723,
-0.00457585328656577));
#27891=CARTESIAN_POINT('',(-0.00941719042915296,-0.0379787743898623,-0.00417585328655812));
#27892=CARTESIAN_POINT('',(-0.014,-0.0379787743898623,-0.0121758532865581));
#27893=CARTESIAN_POINT('Origin',(-0.01249999999999,-0.0379787743898623,
-0.0121758532865681));
#27894=CARTESIAN_POINT('Origin',(-0.0148,-0.0412787743898723,-0.00437585328655813));
#27895=CARTESIAN_POINT('',(-0.01459999999999,-0.040878774389866,-0.00417585328655938));
#27896=CARTESIAN_POINT('',(-0.015,-0.0408787743898623,-0.00457585328656813));
#27897=CARTESIAN_POINT('',(-0.01459999999999,-0.0412787743898723,-0.00417585328655813));
#27898=CARTESIAN_POINT('Origin',(-0.0035,-0.0412787743898723,-0.0121758532865581));
#27899=CARTESIAN_POINT('',(0.007600000000005,-0.0412787743898698,-0.00457585328656563));
#27900=CARTESIAN_POINT('',(0.0076,-0.0412787743898723,-0.0116013970219043));
#27901=CARTESIAN_POINT('',(0.00760000000001,-0.0412787743898723,-0.00817585328656813));
#27902=CARTESIAN_POINT('',(-0.00924999999999,-0.0412787743898723,-0.00457585328656813));
#27903=CARTESIAN_POINT('',(0.0076,-0.0412787743898723,-0.0197758532865581));
#27904=CARTESIAN_POINT('',(0.00225000000001,-0.0412787743898723,-0.0197758532865681));
#27905=CARTESIAN_POINT('',(0.0076,-0.0412787743898723,-0.0127503095512119));
#27906=CARTESIAN_POINT('',(0.00760000000001,-0.0412787743898723,-0.00817585328656813));
#27907=CARTESIAN_POINT('',(0.0042999999999872,-0.0412787743898851,-0.0121758532865581));
#27908=CARTESIAN_POINT('Origin',(0.00600000000001,-0.0412787743898723,-0.0121758532865681));
#27909=CARTESIAN_POINT('Origin',(0.00600000000001,-0.0412787743898723,-0.0121758532865681));
#27910=CARTESIAN_POINT('',(-0.00320000000001261,-0.0412787743898849,-0.0121758532865581));
#27911=CARTESIAN_POINT('Origin',(1.00006808390063E-14,-0.0412787743898723,
-0.0121758532865681));
#27912=CARTESIAN_POINT('',(-0.0142000000000126,-0.0412787743898849,-0.0121758532865581));
#27913=CARTESIAN_POINT('Origin',(-0.01249999999999,-0.0412787743898723,
-0.0121758532865681));
#27914=CARTESIAN_POINT('Origin',(-0.015,-0.0408787743898723,-0.0197758532865581));
#27915=CARTESIAN_POINT('',(-0.01459999999999,-0.0412787743898723,-0.0197758532865681));
#27916=CARTESIAN_POINT('Origin',(-0.0146,-0.0412787743898723,-0.00457585328655813));
#27917=CARTESIAN_POINT('',(-0.01459999999999,-0.0408787743898623,-0.00417585328655813));
#27918=CARTESIAN_POINT('Origin',(0.008,-0.0412787743898723,-0.0201758532865581));
#27919=CARTESIAN_POINT('',(0.00760000000000835,-0.03664344923035,-0.0201758532865647));
#27920=CARTESIAN_POINT('',(0.00404999999998256,-0.0355287743898723,-0.0201758532865756));
#27921=CARTESIAN_POINT('Origin',(0.00600000000001,-0.0355287743898623,-0.0201758532865681));
#27922=CARTESIAN_POINT('',(0.0076,-0.0408787743898723,-0.0201758532865581));
#27923=CARTESIAN_POINT('',(0.00760000000001,-0.0412787743898723,-0.0201758532865681));
#27924=CARTESIAN_POINT('',(0.00225000000001,-0.0408787743898623,-0.0201758532865681));
#27925=CARTESIAN_POINT('',(-0.00982716095192098,-0.0365787743898654,-0.0201758532865681));
#27926=CARTESIAN_POINT('Origin',(-0.00649999999999,-0.0372787743898623,
-0.0201758532865681));
#27927=CARTESIAN_POINT('',(-0.0146,-0.0365787743898723,-0.0201758532865581));
#27928=CARTESIAN_POINT('',(-0.00349999999999,-0.0365787743898623,-0.0201758532865681));
#27929=CARTESIAN_POINT('',(-0.0146,-0.0301787743898723,-0.0201758532865581));
#27930=CARTESIAN_POINT('',(-0.01459999999999,-0.0412787743898723,-0.0201758532865681));
#27931=CARTESIAN_POINT('',(0.0076,-0.0301787743898723,-0.0201758532865581));
#27932=CARTESIAN_POINT('',(0.00225000000001,-0.0301787743898623,-0.0201758532865681));
#27933=CARTESIAN_POINT('',(0.0076000000000095,-0.0344140995493838,-0.0201758532865661));
#27934=CARTESIAN_POINT('',(0.00760000000001,-0.0412787743898723,-0.0201758532865681));
#27935=CARTESIAN_POINT('Origin',(0.00600000000001,-0.0355287743898623,-0.0201758532865681));
#27936=CARTESIAN_POINT('Origin',(-0.0125,-0.0412787743898723,-0.0121758532865581));
#27937=CARTESIAN_POINT('',(-0.014,-0.0410787743898623,-0.0121758532865581));
#27938=CARTESIAN_POINT('Origin',(-0.01249999999999,-0.0410787743898623,
-0.0121758532865681));
#27939=CARTESIAN_POINT('',(-0.014,-0.0412787743898723,-0.0121758532865581));
#27940=CARTESIAN_POINT('Origin',(-0.0065,-0.0372787743898723,-0.00417585328655812));
#27941=CARTESIAN_POINT('',(-0.00941719042915714,-0.0365787743898654,-0.0197758532865648));
#27942=CARTESIAN_POINT('Origin',(-0.00649999999999,-0.0372787743898623,
-0.0197758532865681));
#27943=CARTESIAN_POINT('',(-0.00941719042915714,-0.0365787743898654,-0.00457585328656813));
#27944=CARTESIAN_POINT('Origin',(-0.00649999999999,-0.0372787743898623,
-0.00457585328656813));
#27945=CARTESIAN_POINT('',(-0.00941719042915296,-0.0365787743898623,-0.00417585328655812));
#27946=CARTESIAN_POINT('Origin',(-0.0065,-0.0372787743898723,-0.00437585328655812));
#27947=CARTESIAN_POINT('',(-0.00982716095192024,-0.0365787743898655,-0.00417585328655479));
#27948=CARTESIAN_POINT('Origin',(-0.00649999999999,-0.0372787743898623,
-0.00417585328655812));
#27949=CARTESIAN_POINT('Ctrl Pts',(-0.00982716095192317,-0.0365787743898723,
-0.00417585328655778));
#27950=CARTESIAN_POINT('Ctrl Pts',(-0.00960936411170229,-0.0365787743898723,
-0.00438898421074458));
#27951=CARTESIAN_POINT('Ctrl Pts',(-0.00941719042915497,-0.0365787743898723,
-0.0045758532865659));
#27952=CARTESIAN_POINT('Origin',(-0.015,-0.0412787743898723,-0.00417585328655813));
#27953=CARTESIAN_POINT('',(0.00760000000001035,-0.034414099549385,-0.00417585328655513));
#27954=CARTESIAN_POINT('',(0.00404999999998751,-0.0355287743898723,-0.00417585328654563));
#27955=CARTESIAN_POINT('Origin',(0.00600000000001,-0.0355287743898623,-0.00417585328655812));
#27956=CARTESIAN_POINT('',(0.007600000000005,-0.0301787743898623,-0.00417585328655812));
#27957=CARTESIAN_POINT('',(0.00760000000001,-0.0412787743898723,-0.00417585328655813));
#27958=CARTESIAN_POINT('',(-0.01459999999999,-0.0301787743898673,-0.00417585328655812));
#27959=CARTESIAN_POINT('',(-0.00924999999999,-0.0301787743898623,-0.00417585328655812));
#27960=CARTESIAN_POINT('',(-0.0145999999999933,-0.0365787743898623,-0.00417585328656146));
#27961=CARTESIAN_POINT('',(-0.01459999999999,-0.0412787743898723,-0.00417585328655813));
#27962=CARTESIAN_POINT('',(-0.015,-0.0365787743898623,-0.00417585328655812));
#27963=CARTESIAN_POINT('',(0.00760000000000625,-0.0408787743898623,-0.00417585328655688));
#27964=CARTESIAN_POINT('',(-0.00924999999999,-0.0408787743898623,-0.00417585328655813));
#27965=CARTESIAN_POINT('',(0.00760000000000835,-0.03664344923035,-0.00417585328655657));
#27966=CARTESIAN_POINT('',(0.00760000000001,-0.0412787743898723,-0.00417585328655813));
#27967=CARTESIAN_POINT('Origin',(0.00600000000001,-0.0355287743898623,-0.00417585328655812));
#27968=CARTESIAN_POINT('Origin',(-0.0065,-0.0372787743898723,-0.0199758532865582));
#27969=CARTESIAN_POINT('Ctrl Pts',(-0.00941719042916361,-0.0365787743898723,
-0.0197758532865588));
#27970=CARTESIAN_POINT('Ctrl Pts',(-0.00960936411170878,-0.0365787743898723,
-0.0199627223623781));
#27971=CARTESIAN_POINT('Ctrl Pts',(-0.00982716095192684,-0.0365787743898723,
-0.0201758532865621));
#27972=CARTESIAN_POINT('Origin',(-0.0125,-0.0411787743898723,-0.0121758532865581));
#27973=CARTESIAN_POINT('',(-0.0141,-0.0411787743898723,-0.0121758532865581));
#27974=CARTESIAN_POINT('Origin',(0.,-0.0411787743898723,-0.0121758532865581));
#27975=CARTESIAN_POINT('',(-0.00249999922097496,-0.0405787743898623,-0.012173879679554));
#27976=CARTESIAN_POINT('',(-0.00176776695296376,-0.0405787743898673,-0.0104080863335944));
#27977=CARTESIAN_POINT('Origin',(1.00006808390063E-14,-0.0405787743898623,
-0.0121758532865681));
#27978=CARTESIAN_POINT('Origin',(1.00006808390063E-14,-0.0405787743898623,
-0.0121758532865681));
#27979=CARTESIAN_POINT('',(-0.0031,-0.0411787743898723,-0.0121758532865581));
#27980=CARTESIAN_POINT('Origin',(0.006,-0.0411787743898723,-0.0121758532865581));
#27981=CARTESIAN_POINT('Origin',(0.00600000000001,-0.0408432743898623,-0.0121758532865681));
#27982=CARTESIAN_POINT('',(0.0044,-0.0411787743898723,-0.0121758532865581));
#27983=CARTESIAN_POINT('Ctrl Pts',(0.00760000000001,-0.0412787743898623,
-0.0116013970219143));
#27984=CARTESIAN_POINT('Ctrl Pts',(0.00770000000001,-0.0411787743898623,
-0.0121758532865681));
#27985=CARTESIAN_POINT('Ctrl Pts',(0.00760000000001,-0.0412787743898623,
-0.0127503095512219));
#27986=CARTESIAN_POINT('Origin',(0.0078,-0.0410787743898723,-0.00817585328655813));
#27987=CARTESIAN_POINT('',(0.008,-0.0408787743898723,-0.0197758532865581));
#27988=CARTESIAN_POINT('',(0.00760000000001,-0.0412787743898723,-0.0197758532865681));
#27989=CARTESIAN_POINT('',(0.00800000000000625,-0.0408787743898673,-0.0045758532865625));
#27990=CARTESIAN_POINT('',(0.00800000000001,-0.0408787743898623,-0.00817585328656813));
#27991=CARTESIAN_POINT('',(0.00800000000001,-0.0408787743898623,-0.00457585328656813));
#27992=CARTESIAN_POINT('Origin',(0.00225,-0.0410787743898723,-0.0199758532865582));
#27993=CARTESIAN_POINT('',(0.00760000000001,-0.0408787743898623,-0.0201758532865681));
#27994=CARTESIAN_POINT('Origin',(-0.00925,-0.0410787743898723,-0.00437585328655813));
#27995=CARTESIAN_POINT('',(0.00760000000001,-0.0412787743898723,-0.00457585328656813));
#27996=CARTESIAN_POINT('Origin',(0.0078,-0.0412787743898723,-0.0199758532865582));
#27997=CARTESIAN_POINT('Ctrl Pts',(0.0076,-0.0366434492303427,-0.0201758532865581));
#27998=CARTESIAN_POINT('Ctrl Pts',(0.00783333333333333,-0.0359003326700224,
-0.0199425199532248));
#27999=CARTESIAN_POINT('Ctrl Pts',(0.00783333333333333,-0.0351572161097022,
-0.0199425199532248));
#28000=CARTESIAN_POINT('Ctrl Pts',(0.0076,-0.0344140995493819,-0.0201758532865581));
#28001=CARTESIAN_POINT('',(0.00800000000001126,-0.0301787743898623,-0.0197758532865643));
#28002=CARTESIAN_POINT('',(0.00760000000001,-0.0301787743898623,-0.0201758532865681));
#28003=CARTESIAN_POINT('',(0.00800000000001,-0.0412787743898723,-0.0197758532865681));
#28004=CARTESIAN_POINT('',(0.00800000000001,-0.0408787743898623,-0.0197758532865681));
#28005=CARTESIAN_POINT('Origin',(0.00225,-0.0299787743898723,-0.0199758532865581));
#28006=CARTESIAN_POINT('',(-0.0145999999999931,-0.0297787743898623,-0.019775853286565));
#28007=CARTESIAN_POINT('',(-0.01459999999999,-0.0301787743898623,-0.0201758532865681));
#28008=CARTESIAN_POINT('',(0.00760000000001,-0.0297787743898617,-0.0197758532865649));
#28009=CARTESIAN_POINT('',(0.00225000000001,-0.0297787743898623,-0.0197758532865681));
#28010=CARTESIAN_POINT('',(0.00760000000001,-0.0297787743898623,-0.0197758532865681));
#28011=CARTESIAN_POINT('Origin',(-0.0148,-0.0412787743898723,-0.0199758532865582));
#28012=CARTESIAN_POINT('',(-0.015,-0.0365787743898723,-0.0197758532865581));
#28013=CARTESIAN_POINT('',(-0.01880000000001,-0.0365787743898623,-0.0159758532865681));
#28014=CARTESIAN_POINT('',(-0.0150000000000006,-0.030178774389866,-0.0197758532865649));
#28015=CARTESIAN_POINT('',(-0.015,-0.0412787743898723,-0.0197758532865681));
#28016=CARTESIAN_POINT('',(-0.015,-0.0301787743898623,-0.0197758532865681));
#28017=CARTESIAN_POINT('Origin',(-0.015,-0.0365787743898723,-0.00417585328655812));
#28018=CARTESIAN_POINT('',(-0.0149999999999967,-0.0365787743898623,-0.00457585328656813));
#28019=CARTESIAN_POINT('',(-0.01479999999999,-0.0365787743898623,-0.00437585328656812));
#28020=CARTESIAN_POINT('',(-0.015,-0.0365787743898623,-0.0121758532865681));
#28021=CARTESIAN_POINT('Ctrl Pts',(-0.0118291591918131,-0.0365787743898723,
-0.0135653933579744));
#28022=CARTESIAN_POINT('Ctrl Pts',(-0.012060061067293,-0.0365787743898723,
-0.0136524861577944));
#28023=CARTESIAN_POINT('Ctrl Pts',(-0.0123125894300976,-0.0365787743898723,
-0.0136792436280273));
#28024=CARTESIAN_POINT('Ctrl Pts',(-0.0125574025636052,-0.0365787743898723,
-0.0136472777291935));
#28025=CARTESIAN_POINT('Ctrl Pts',(-0.0127250974036528,-0.0365787743898723,
-0.0136253813700599));
#28026=CARTESIAN_POINT('Ctrl Pts',(-0.0128891708546214,-0.0365787743898723,
-0.0135758966937495));
#28027=CARTESIAN_POINT('Ctrl Pts',(-0.0130392347235788,-0.0365787743898723,
-0.0134989032831501));
#28028=CARTESIAN_POINT('Ctrl Pts',(-0.0131082450132257,-0.0365787743898723,
-0.0134634961088363));
#28029=CARTESIAN_POINT('Ctrl Pts',(-0.0131753067095831,-0.0365787743898723,
-0.0134214203887249));
#28030=CARTESIAN_POINT('Ctrl Pts',(-0.0132355458760869,-0.0365787743898723,
-0.0133757167396176));
#28031=CARTESIAN_POINT('Ctrl Pts',(-0.0133533787985701,-0.0365787743898723,
-0.0132863165228648));
#28032=CARTESIAN_POINT('Ctrl Pts',(-0.0134424576307166,-0.0365787743898723,
-0.0131870659007685));
#28033=CARTESIAN_POINT('Ctrl Pts',(-0.0135097162431771,-0.0365787743898723,
-0.0130944668684115));
#28034=CARTESIAN_POINT('Ctrl Pts',(-0.0135610488334419,-0.0365787743898723,
-0.0130237941617795));
#28035=CARTESIAN_POINT('Ctrl Pts',(-0.0136022225954696,-0.0365787743898723,
-0.0129542292552571));
#28036=CARTESIAN_POINT('Ctrl Pts',(-0.0136385197303841,-0.0365787743898723,
-0.0128791079143929));
#28037=CARTESIAN_POINT('Ctrl Pts',(-0.0137280481667466,-0.0365787743898723,
-0.0126938179128299));
#28038=CARTESIAN_POINT('Ctrl Pts',(-0.0137761444620793,-0.0365787743898723,
-0.012487113971115));
#28039=CARTESIAN_POINT('Ctrl Pts',(-0.0137738110437006,-0.0365787743898723,
-0.0122905106090682));
#28040=CARTESIAN_POINT('Ctrl Pts',(-0.0137734593352465,-0.0365787743898723,
-0.0122608772329151));
#28041=CARTESIAN_POINT('Ctrl Pts',(-0.0137720035177717,-0.0365787743898723,
-0.0122313476771935));
#28042=CARTESIAN_POINT('Ctrl Pts',(-0.0137694124812826,-0.0365787743898723,
-0.0122019199453004));
#28043=CARTESIAN_POINT('Ctrl Pts',(-0.0137686492173546,-0.0365787743898723,
-0.0121932511649365));
#28044=CARTESIAN_POINT('Ctrl Pts',(-0.0137677873061495,-0.0365787743898723,
-0.012184591241161));
#28045=CARTESIAN_POINT('Ctrl Pts',(-0.0137668274805527,-0.0365787743898723,
-0.0121759402143804));
#28046=CARTESIAN_POINT('Ctrl Pts',(-0.0133941365248104,-0.0365787743898724,
-0.0112817167617477));
#28047=CARTESIAN_POINT('Ctrl Pts',(-0.0132597060893964,-0.0365787743898723,
-0.011114394916356));
#28048=CARTESIAN_POINT('Ctrl Pts',(-0.0130804465300667,-0.0365787743898723,
-0.0109853813929878));
#28049=CARTESIAN_POINT('Ctrl Pts',(-0.0128820499211865,-0.0365787743898723,
-0.0109023634156306));
#28050=CARTESIAN_POINT('Ctrl Pts',(-0.0127886426167731,-0.0365787743898723,
-0.0108632776392831));
#28051=CARTESIAN_POINT('Ctrl Pts',(-0.0126927759244174,-0.0365787743898723,
-0.0108346803378181));
#28052=CARTESIAN_POINT('Ctrl Pts',(-0.0125911049282069,-0.0365787743898723,
-0.0108163699769736));
#28053=CARTESIAN_POINT('Ctrl Pts',(-0.0124768272788988,-0.0365787743898723,
-0.0107957892305141));
#28054=CARTESIAN_POINT('Ctrl Pts',(-0.0123453825492587,-0.0365787743898723,
-0.0107866442237817));
#28055=CARTESIAN_POINT('Ctrl Pts',(-0.0122012816269697,-0.0365787743898723,
-0.0108034555473256));
#28056=CARTESIAN_POINT('Ctrl Pts',(-0.0120960331525637,-0.0365787743898723,
-0.0108157342068071));
#28057=CARTESIAN_POINT('Ctrl Pts',(-0.0119859286825378,-0.0365787743898723,
-0.0108427326623353));
#28058=CARTESIAN_POINT('Ctrl Pts',(-0.0118828353784451,-0.0365787743898723,
-0.0108814909939163));
#28059=CARTESIAN_POINT('Ctrl Pts',(-0.0117210892635519,-0.0365787743898723,
-0.0109423000795124));
#28060=CARTESIAN_POINT('Ctrl Pts',(-0.0115703802921963,-0.0365787743898723,
-0.0110322107690672));
#28061=CARTESIAN_POINT('Ctrl Pts',(-0.0114382293014629,-0.0365787743898723,
-0.0111440745982799));
#28062=CARTESIAN_POINT('Ctrl Pts',(-0.0113874539496207,-0.0365787743898723,
-0.011187055171147));
#28063=CARTESIAN_POINT('Ctrl Pts',(-0.0113394391814985,-0.0365787743898723,
-0.0112332851966829));
#28064=CARTESIAN_POINT('Ctrl Pts',(-0.0112946598499865,-0.0365787743898723,
-0.0112823688862808));
#28065=CARTESIAN_POINT('Ctrl Pts',(-0.0112586129422819,-0.0365787743898723,
-0.0113218807585887));
#28066=CARTESIAN_POINT('Ctrl Pts',(-0.0112180794482739,-0.0365787743898723,
-0.0113702875028219));
#28067=CARTESIAN_POINT('Ctrl Pts',(-0.0111761548550522,-0.0365787743898723,
-0.0114297153330889));
#28068=CARTESIAN_POINT('Ctrl Pts',(-0.0111346114653199,-0.0365787743898723,
-0.0114886028099613));
#28069=CARTESIAN_POINT('Ctrl Pts',(-0.0110920966712173,-0.0365787743898723,
-0.0115579296649615));
#28070=CARTESIAN_POINT('Ctrl Pts',(-0.0110538234060338,-0.0365787743898723,
-0.0116378502540936));
#28071=CARTESIAN_POINT('Ctrl Pts',(-0.0110495499905092,-0.0365787743898723,
-0.0116467738169172));
#28072=CARTESIAN_POINT('Ctrl Pts',(-0.0110453304317794,-0.0365787743898723,
-0.011655828468478));
#28073=CARTESIAN_POINT('Ctrl Pts',(-0.0110411708242858,-0.0365787743898723,
-0.0116650129552322));
#28074=CARTESIAN_POINT('Origin',(0.006,-0.0355287743898723,-0.0199758532865582));
#28075=CARTESIAN_POINT('',(0.00444999999999767,-0.0355287743898723,-0.0197758532865605));
#28076=CARTESIAN_POINT('Origin',(0.00600000000001,-0.0355287743898623,-0.0197758532865681));
#28077=CARTESIAN_POINT('',(0.00425,-0.0355287743898723,-0.0199758532865582));
#28078=CARTESIAN_POINT('Origin',(0.0078,-0.0412787743898723,-0.00437585328655813));
#28079=CARTESIAN_POINT('Ctrl Pts',(0.0076,-0.0344140995493819,-0.00417585328655812));
#28080=CARTESIAN_POINT('Ctrl Pts',(0.00783333333334,-0.0351572161097022,
-0.00440918661989812));
#28081=CARTESIAN_POINT('Ctrl Pts',(0.00783333333334,-0.0359003326700224,
-0.00440918661989812));
#28082=CARTESIAN_POINT('Ctrl Pts',(0.0076,-0.0366434492303427,-0.00417585328655813));
#28083=CARTESIAN_POINT('',(0.00760000000001,-0.0408787743898623,-0.00417585328655813));
#28084=CARTESIAN_POINT('',(0.00800000000000625,-0.030178774389861,-0.00457585328656312));
#28085=CARTESIAN_POINT('',(0.00800000000001,-0.0412787743898723,-0.00457585328656813));
#28086=CARTESIAN_POINT('',(0.00800000000001,-0.0301787743898623,-0.00457585328656812));
#28087=CARTESIAN_POINT('Origin',(-0.0148,-0.0412787743898723,-0.00437585328655813));
#28088=CARTESIAN_POINT('',(-0.015,-0.030178774389866,-0.00457585328656624));
#28089=CARTESIAN_POINT('',(-0.01459999999999,-0.0301787743898623,-0.00417585328655812));
#28090=CARTESIAN_POINT('',(-0.015,-0.0412787743898723,-0.00457585328656813));
#28091=CARTESIAN_POINT('Origin',(-0.00925,-0.0299787743898723,-0.00437585328655811));
#28092=CARTESIAN_POINT('',(0.0076000000000075,-0.0297787743898636,-0.00457585328656249));
#28093=CARTESIAN_POINT('',(0.00760000000001,-0.0301787743898623,-0.00417585328655812));
#28094=CARTESIAN_POINT('',(-0.0145999999999956,-0.0297787743898661,-0.00457585328656312));
#28095=CARTESIAN_POINT('',(-0.00924999999999,-0.0297787743898623,-0.00457585328656812));
#28096=CARTESIAN_POINT('',(-0.01459999999999,-0.0297787743898623,-0.00457585328656812));
#28097=CARTESIAN_POINT('Origin',(0.006,-0.0355287743898723,-0.00437585328655812));
#28098=CARTESIAN_POINT('',(0.00445000000000762,-0.0355287743898723,-0.00457585328656574));
#28099=CARTESIAN_POINT('Origin',(0.00600000000001,-0.0355287743898623,-0.00457585328656812));
#28100=CARTESIAN_POINT('',(0.00425,-0.0355287743898723,-0.00437585328655812));
#28101=CARTESIAN_POINT('Origin',(0.,-0.0412787743898723,-0.0121758532865581));
#28102=CARTESIAN_POINT('',(-0.00249999955320377,-0.0395787127102368,-0.0121769399287834));
#28103=CARTESIAN_POINT('',(-0.00249999997283516,-0.0385787905737985,-0.0121755877114987));
#28104=CARTESIAN_POINT('Ctrl Pts',(-0.00249999999999882,-0.0395786432478283,
-0.0121758508550077));
#28105=CARTESIAN_POINT('Ctrl Pts',(-0.00249999952765863,-0.0395477317163263,
-0.0116902140117491));
#28106=CARTESIAN_POINT('Ctrl Pts',(-0.00235420867782621,-0.0395168201848242,
-0.0112046011700908));
#28107=CARTESIAN_POINT('Ctrl Pts',(-0.00208694474875081,-0.0394859086533222,
-0.0107993862089782));
#28108=CARTESIAN_POINT('Ctrl Pts',(-0.00199401377133162,-0.0394751603310703,
-0.0106584879496008));
#28109=CARTESIAN_POINT('Ctrl Pts',(-0.00188684506187664,-0.0394644120088185,
-0.0105271641201691));
#28110=CARTESIAN_POINT('Ctrl Pts',(-0.00176776456039862,-0.0394536636865666,
-0.0104080839410272));
#28111=CARTESIAN_POINT('Ctrl Pts',(-0.00143160692048451,-0.0394233217699943,
-0.0100719272110501));
#28112=CARTESIAN_POINT('Ctrl Pts',(-0.000995195371062074,-0.0393929798534221,
-0.00983340281983273));
#28113=CARTESIAN_POINT('Ctrl Pts',(-0.000529040034186219,-0.0393626379368499,
-0.00973247107285754));
#28114=CARTESIAN_POINT('Ctrl Pts',(-0.000355157912828381,-0.0393513199996682,
-0.00969482219299269));
#28115=CARTESIAN_POINT('Ctrl Pts',(-0.000177402100138263,-0.0393400020624865,
-0.00967585297889307));
#28116=CARTESIAN_POINT('Ctrl Pts',(4.33564861886497E-9,-0.0393286841253049,
-0.00967585328656186));
#28117=CARTESIAN_POINT('Ctrl Pts',(0.000477367164465555,-0.0392982299735971,
-0.00967585411443285));
#28118=CARTESIAN_POINT('Ctrl Pts',(0.000956261322705523,-0.0392677758218892,
-0.00981689817770217));
#28119=CARTESIAN_POINT('Ctrl Pts',(0.00135812160581124,-0.0392373216701814,
-0.0100769236298453));
#28120=CARTESIAN_POINT('Ctrl Pts',(0.00150598737596406,-0.0392261159681353,
-0.0101726008225335));
#28121=CARTESIAN_POINT('Ctrl Pts',(0.00164356551969349,-0.0392149102660893,
-0.0102838843749181));
#28122=CARTESIAN_POINT('Ctrl Pts',(0.00176777069192936,-0.0392037045640432,
-0.0104080900725626));
#28123=CARTESIAN_POINT('Ctrl Pts',(0.00210526431200422,-0.0391732561303674,
-0.0107455851202919));
#28124=CARTESIAN_POINT('Ctrl Pts',(0.00234413374807478,-0.0391428076966918,
-0.0111838614835386));
#28125=CARTESIAN_POINT('Ctrl Pts',(0.00244445215636216,-0.039112359263016,
-0.0116517791932694));
#28126=CARTESIAN_POINT('Ctrl Pts',(0.00248139040510301,-0.0391011478429379,
-0.0118240712087365));
#28127=CARTESIAN_POINT('Ctrl Pts',(0.00250000043860317,-0.0390899364228596,
-0.0120001268556178));
#28128=CARTESIAN_POINT('Ctrl Pts',(0.00249999999999221,-0.0390787250027815,
-0.012175859526305));
#28129=CARTESIAN_POINT('Ctrl Pts',(0.00249999880879463,-0.0390482765691058,
-0.0126531215083521));
#28130=CARTESIAN_POINT('Ctrl Pts',(0.00235901179047531,-0.0390178281354301,
-0.0131319317915853));
#28131=CARTESIAN_POINT('Ctrl Pts',(0.00209907640032062,-0.0389873797017544,
-0.0135337480783653));
#28132=CARTESIAN_POINT('Ctrl Pts',(0.00200336557055327,-0.0389761682816762,
-0.0136817008838638));
#28133=CARTESIAN_POINT('Ctrl Pts',(0.0018920310394174,-0.0389649568615981,
-0.0138193568680316));
#28134=CARTESIAN_POINT('Ctrl Pts',(0.00176776186759135,-0.0389537454415199,
-0.0139436253248849));
#28135=CARTESIAN_POINT('Ctrl Pts',(0.00143020318323218,-0.038923291289812,
-0.0142811820671271));
#28136=CARTESIAN_POINT('Ctrl Pts',(0.00099183243510392,-0.0388928371381041,
-0.0145200730555509));
#28137=CARTESIAN_POINT('Ctrl Pts',(0.000523815083728861,-0.0388623829863963,
-0.0146203609584745));
#28138=CARTESIAN_POINT('Ctrl Pts',(0.000351606609750884,-0.0388511772843502,
-0.0146572622115374));
#28139=CARTESIAN_POINT('Ctrl Pts',(0.000175639028300414,-0.0388399715823042,
-0.0146758538587222));
#28140=CARTESIAN_POINT('Ctrl Pts',(-8.14384507266024E-9,-0.0388287658802581,
-0.0146758532865448));
#28141=CARTESIAN_POINT('Ctrl Pts',(-0.000475611709019986,-0.0387984239636858,
-0.0146758517372481));
#28142=CARTESIAN_POINT('Ctrl Pts',(-0.000952894728007072,-0.0387680820471136,
-0.014535808823928));
#28143=CARTESIAN_POINT('Ctrl Pts',(-0.00135378915737485,-0.0387377401305413,
-0.0142775799379984));
#28144=CARTESIAN_POINT('Ctrl Pts',(-0.0015033280949442,-0.0387264221933597,
-0.0141812571397182));
#28145=CARTESIAN_POINT('Ctrl Pts',(-0.00164238275388543,-0.038715104256178,
-0.0140690053510172));
#28146=CARTESIAN_POINT('Ctrl Pts',(-0.00176777338472311,-0.0387037863189964,
-0.0139436138077443));
#28147=CARTESIAN_POINT('Ctrl Pts',(-0.00211024007039254,-0.0386728747874944,
-0.0136011446300332));
#28148=CARTESIAN_POINT('Ctrl Pts',(-0.00235093239488195,-0.0386419632559923,
-0.0131553245197027));
#28149=CARTESIAN_POINT('Ctrl Pts',(-0.00244879874153802,-0.0386110517244903,
-0.0126792266305502));
#28150=CARTESIAN_POINT('Ctrl Pts',(-0.00248282808205786,-0.0386003034022384,
-0.0125136814994166));
#28151=CARTESIAN_POINT('Ctrl Pts',(-0.0025000006786659,-0.0385895550799866,
-0.0123447051822019));
#28152=CARTESIAN_POINT('Ctrl Pts',(-0.00249999999997981,-0.0385788067577347,
-0.0121758432386148));
#28153=CARTESIAN_POINT('',(-0.00249999979604092,-0.0375788205392406,-0.0121751469739251));
#28154=CARTESIAN_POINT('Ctrl Pts',(-0.0024999999456905,-0.0385787743898623,
-0.0121753321843825));
#28155=CARTESIAN_POINT('Ctrl Pts',(-0.00249989871899367,-0.0385478595459227,
-0.0116896947250819));
#28156=CARTESIAN_POINT('Ctrl Pts',(-0.00235400676731844,-0.0385169447019829,
-0.0112041116200849));
#28157=CARTESIAN_POINT('Ctrl Pts',(-0.00208665818069438,-0.0384860298580432,
-0.0107989518242373));
#28158=CARTESIAN_POINT('Ctrl Pts',(-0.00199371071341842,-0.0384752818810978,
-0.0106580923667716));
#28159=CARTESIAN_POINT('Ctrl Pts',(-0.0018865314487592,-0.0384645339041523,
-0.0105268076403119));
#28160=CARTESIAN_POINT('Ctrl Pts',(-0.0017674458724513,-0.0384537859272069,
-0.0104077653113841));
#28161=CARTESIAN_POINT('Ctrl Pts',(-0.00143122666542549,-0.0384234407217021,
-0.0100716682064659));
#28162=CARTESIAN_POINT('Ctrl Pts',(-0.000994770813954565,-0.0383930955161973,
-0.00983322226997918));
#28163=CARTESIAN_POINT('Ctrl Pts',(-0.000528596084364588,-0.0383627503106924,
-0.00973237499125969));
#28164=CARTESIAN_POINT('Ctrl Pts',(-0.000354730519714355,-0.0383514326953121,
-0.00969476276574625));
#28165=CARTESIAN_POINT('Ctrl Pts',(-0.00017699570173726,-0.0383401150799318,
-0.00967582585992544));
#28166=CARTESIAN_POINT('Ctrl Pts',(3.86968202952469E-7,-0.0383287974645515,
-0.00967585331650698));
#28167=CARTESIAN_POINT('Ctrl Pts',(0.000477751087115689,-0.0382983400162786,
-0.00967592720640196));
#28168=CARTESIAN_POINT('Ctrl Pts',(0.000956624670283315,-0.0382678825680056,
-0.00981704529372479));
#28169=CARTESIAN_POINT('Ctrl Pts',(0.00135844566361926,-0.0382374251197327,
-0.0100771333483591));
#28170=CARTESIAN_POINT('Ctrl Pts',(0.00150627662809758,-0.0382262197471205,
-0.0101728204045447));
#28171=CARTESIAN_POINT('Ctrl Pts',(0.00164382035946017,-0.0382150143745082,
-0.0102841079865441));
#28172=CARTESIAN_POINT('Ctrl Pts',(0.00176799314281305,-0.038203809001896,
-0.0104083125523836));
#28173=CARTESIAN_POINT('Ctrl Pts',(0.00210544517894053,-0.038173357274058,
-0.0107458509606174));
#28174=CARTESIAN_POINT('Ctrl Pts',(0.00234425965674057,-0.0381429055462199,
-0.0111841585824246));
#28175=CARTESIAN_POINT('Ctrl Pts',(0.00244451877559458,-0.0381124538183818,
-0.0116520900234653));
#28176=CARTESIAN_POINT('Ctrl Pts',(0.00248143012316302,-0.0381012427253347,
-0.0118243634311701));
#28177=CARTESIAN_POINT('Ctrl Pts',(0.00250001775731488,-0.0380900316322877,
-0.0120003971208957));
#28178=CARTESIAN_POINT('Ctrl Pts',(0.00249999998721497,-0.0380788205392406,
-0.0121761061207873));
#28179=CARTESIAN_POINT('Ctrl Pts',(0.00249995171982089,-0.0380483688114026,
-0.0126533693654073));
#28180=CARTESIAN_POINT('Ctrl Pts',(0.0023589167616459,-0.0380179170835647,
-0.0131321667312888));
#28181=CARTESIAN_POINT('Ctrl Pts',(0.00209894066755153,-0.0379874653557266,
-0.0135339578753503));
#28182=CARTESIAN_POINT('Ctrl Pts',(0.00200322799743868,-0.0379762542626795,
-0.0136818811040601));
#28183=CARTESIAN_POINT('Ctrl Pts',(0.00189189689820637,-0.0379650431696323,
-0.0138195087500959));
#28184=CARTESIAN_POINT('Ctrl Pts',(0.00176763559080942,-0.0379538320765852,
-0.0139437515919207));
#28185=CARTESIAN_POINT('Ctrl Pts',(0.00143005188452377,-0.0379233746283123,
-0.0142812851323386));
#28186=CARTESIAN_POINT('Ctrl Pts',(0.000991662842117688,-0.0378929171800394,
-0.0145201450129968));
#28187=CARTESIAN_POINT('Ctrl Pts',(0.000523637186059175,-0.0378624597317665,
-0.014620399072052));
#28188=CARTESIAN_POINT('Ctrl Pts',(0.000351449357938283,-0.0378512543591542,
-0.0146572827951248));
#28189=CARTESIAN_POINT('Ctrl Pts',(0.000175504773985148,-0.037840048986542,
-0.0146758616223606));
#28190=CARTESIAN_POINT('Ctrl Pts',(-1.18700254736605E-7,-0.0378288436139298,
-0.0146758532837401));
#28191=CARTESIAN_POINT('Ctrl Pts',(-0.00047572362672246,-0.037798498408425,
-0.0146758307019698));
#28192=CARTESIAN_POINT('Ctrl Pts',(-0.000953001524368115,-0.0377681532029201,
-0.0145357659183382));
#28193=CARTESIAN_POINT('Ctrl Pts',(-0.00135388507917457,-0.0377378079974153,
-0.0142775181486112));
#28194=CARTESIAN_POINT('Ctrl Pts',(-0.00150339950196762,-0.037726490382035,
-0.0141812014856665));
#28195=CARTESIAN_POINT('Ctrl Pts',(-0.00164243175618251,-0.0377151727666547,
-0.0140689606143419));
#28196=CARTESIAN_POINT('Ctrl Pts',(-0.0017678034628228,-0.0377038551512744,
-0.013943583728914));
#28197=CARTESIAN_POINT('Ctrl Pts',(-0.00211026489263892,-0.0376729403073345,
-0.0136011081528836));
#28198=CARTESIAN_POINT('Ctrl Pts',(-0.00235094972065609,-0.0376420254633948,
-0.0131552832078728));
#28199=CARTESIAN_POINT('Ctrl Pts',(-0.00244880770272406,-0.0376111106194549,
-0.0126791830344166));
#28200=CARTESIAN_POINT('Ctrl Pts',(-0.00248282939590269,-0.0376003626425096,
-0.0125136601646279));
#28201=CARTESIAN_POINT('Ctrl Pts',(-0.00249999895762901,-0.0375896146655642,
-0.0123447073642587));
#28202=CARTESIAN_POINT('Ctrl Pts',(-0.00249999999995236,-0.0375788666886189,
-0.0121758687202782));
#28203=CARTESIAN_POINT('',(-0.00249999943132573,-0.0365786614003052,-0.0121771638243569));
#28204=CARTESIAN_POINT('Ctrl Pts',(-0.00249999959212947,-0.0375787743898623,
-0.012174425227572));
#28205=CARTESIAN_POINT('Ctrl Pts',(-0.00249972218252544,-0.0375478504116054,
-0.0116887842955938));
#28206=CARTESIAN_POINT('Ctrl Pts',(-0.00235365206766289,-0.0375169264333485,
-0.0112032512070332));
#28207=CARTESIAN_POINT('Ctrl Pts',(-0.00208615315541311,-0.0374860024550917,
-0.0107981867767815));
#28208=CARTESIAN_POINT('Ctrl Pts',(-0.0019932266425179,-0.0374752597666819,
-0.010657471344765));
#28209=CARTESIAN_POINT('Ctrl Pts',(-0.00188609410542575,-0.0374645170782721,
-0.0105263208120313));
#28210=CARTESIAN_POINT('Ctrl Pts',(-0.0017670763035595,-0.0374537743898623,
-0.0104073959539095));
#28211=CARTESIAN_POINT('Ctrl Pts',(-0.00143078133828147,-0.0374234200061557,
-0.0100713636091205));
#28212=CARTESIAN_POINT('Ctrl Pts',(-0.000994268242573484,-0.0373930656224491,
-0.0098330076723254));
#28213=CARTESIAN_POINT('Ctrl Pts',(-0.000528065628921522,-0.0373627112387425,
-0.00973226029844577));
#28214=CARTESIAN_POINT('Ctrl Pts',(-0.00035432413796164,-0.0373513989557824,
-0.00969471439364909));
#28215=CARTESIAN_POINT('Ctrl Pts',(-0.000176723339944004,-0.0373400866728224,
-0.00967581611874746));
#28216=CARTESIAN_POINT('Ctrl Pts',(5.25011049869234E-7,-0.0373287743898623,
-0.00967585334168542));
#28217=CARTESIAN_POINT('Ctrl Pts',(0.000477896448403842,-0.0372983077550749,
-0.00967595359179943));
#28218=CARTESIAN_POINT('Ctrl Pts',(0.000956767990482746,-0.0372678411202875,
-0.00981710224408529));
#28219=CARTESIAN_POINT('Ctrl Pts',(0.0013585775187882,-0.0372373744855001,
-0.0100772187005848));
#28220=CARTESIAN_POINT('Ctrl Pts',(0.00150628925517822,-0.0372261744536208,
-0.0101728417526692));
#28221=CARTESIAN_POINT('Ctrl Pts',(0.00164372861443351,-0.0372149744217415,
-0.0102840407011479));
#28222=CARTESIAN_POINT('Ctrl Pts',(0.00176781891539311,-0.0372037743898623,
-0.0104081382975459));
#28223=CARTESIAN_POINT('Ctrl Pts',(0.00210530925518493,-0.0371733134873149,
-0.0107456484788562));
#28224=CARTESIAN_POINT('Ctrl Pts',(0.00234416805757305,-0.0371428525847675,
-0.0111839393494879));
#28225=CARTESIAN_POINT('Ctrl Pts',(0.00244447101894353,-0.0371123916822201,
-0.0116518671822145));
#28226=CARTESIAN_POINT('Ctrl Pts',(0.00248136983780919,-0.0371011859181008,
-0.0118240055129882));
#28227=CARTESIAN_POINT('Ctrl Pts',(0.00249997342184992,-0.0370899801539816,
-0.0119999000376457));
#28228=CARTESIAN_POINT('Ctrl Pts',(0.00249999997141761,-0.0370787743898623,
-0.0121754752496033));
#28229=CARTESIAN_POINT('Ctrl Pts',(0.00250007214175651,-0.0370483134873149,
-0.012652745640471));
#28230=CARTESIAN_POINT('Ctrl Pts',(0.00235915399073559,-0.0370178525847676,
-0.0131315841864723));
#28231=CARTESIAN_POINT('Ctrl Pts',(0.00209927324429766,-0.0369873916822203,
-0.0135334437423937));
#28232=CARTESIAN_POINT('Ctrl Pts',(0.00200366995942426,-0.036976185918101,
-0.0136812772934761));
#28233=CARTESIAN_POINT('Ctrl Pts',(0.00189246969922872,-0.0369649801539816,
-0.0138188349016734));
#28234=CARTESIAN_POINT('Ctrl Pts',(0.00176835344381461,-0.0369537743898623,
-0.013943033554032));
#28235=CARTESIAN_POINT('Ctrl Pts',(0.00143090170160338,-0.036923307755075,
-0.0142807093200213));
#28236=CARTESIAN_POINT('Ctrl Pts',(0.00099260274506201,-0.0368928411202877,
-0.014519748390164));
#28237=CARTESIAN_POINT('Ctrl Pts',(0.00052461138696062,-0.0368623744855004,
-0.0146201901890065));
#28238=CARTESIAN_POINT('Ctrl Pts',(0.000352570130465234,-0.036851174453621,
-0.0146571142325351));
#28239=CARTESIAN_POINT('Ctrl Pts',(0.000176770592362688,-0.0368399744217417,
-0.0146757630315266));
#28240=CARTESIAN_POINT('Ctrl Pts',(1.28108491020491E-6,-0.0368287743898624,
-0.0146758529583224));
#28241=CARTESIAN_POINT('Ctrl Pts',(-0.00047433147611545,-0.0367984200061557,
-0.0146760966783844));
#28242=CARTESIAN_POINT('Ctrl Pts',(-0.000951693785334355,-0.036768065622449,
-0.0145362948381555));
#28243=CARTESIAN_POINT('Ctrl Pts',(-0.0013527249599611,-0.0367377112387423,
-0.0142782650404013));
#28244=CARTESIAN_POINT('Ctrl Pts',(-0.00150217876429455,-0.0367263989557823,
-0.0141821040999417));
#28245=CARTESIAN_POINT('Ctrl Pts',(-0.00164117520491927,-0.0367150866728224,
-0.0140700374903543));
#28246=CARTESIAN_POINT('Ctrl Pts',(-0.00176654138897415,-0.0367037743898624,
-0.0139448449544416));
#28247=CARTESIAN_POINT('Ctrl Pts',(-0.00210925038622623,-0.0366728504116055,
-0.0136026106528273));
#28248=CARTESIAN_POINT('Ctrl Pts',(-0.00235025384378205,-0.0366419264333487,
-0.0131569534190921));
#28249=CARTESIAN_POINT('Ctrl Pts',(-0.0024484501037743,-0.0366110024550918,
-0.0126809197072669));
#28250=CARTESIAN_POINT('Ctrl Pts',(-0.00248256252667631,-0.036600259766682,
-0.0125155502390746));
#28251=CARTESIAN_POINT('Ctrl Pts',(-0.00249985165456606,-0.0365895170782721,
-0.0123467443051594));
#28252=CARTESIAN_POINT('Ctrl Pts',(-0.00249999904591269,-0.0365787743898623,
-0.0121780374192565));
#28253=CARTESIAN_POINT('',(-0.00250020961650365,-0.0355784048170972,-0.0121753040281057));
#28254=CARTESIAN_POINT('Ctrl Pts',(-0.00249999999990522,-0.0365784947127869,
-0.0121758750560007));
#28255=CARTESIAN_POINT('Ctrl Pts',(-0.00250000418566703,-0.0365458789096059,
-0.0116951827047534));
#28256=CARTESIAN_POINT('Ctrl Pts',(-0.00235822192526014,-0.0365179347736311,
-0.0112384571840363));
#28257=CARTESIAN_POINT('Ctrl Pts',(-0.00213008674960362,-0.0364908206152539,
-0.0108671400104112));
#28258=CARTESIAN_POINT('Ctrl Pts',(-0.00205373010295132,-0.036481745529816,
-0.0107428604724538));
#28259=CARTESIAN_POINT('Ctrl Pts',(-0.00196792392084753,-0.0364727634213843,
-0.01062757268742));
#28260=CARTESIAN_POINT('Ctrl Pts',(-0.00187459701875102,-0.0364637302489831,
-0.0105218018915616));
#28261=CARTESIAN_POINT('Ctrl Pts',(-0.0018621755065719,-0.0364625279626275,
-0.0105077241369224));
#28262=CARTESIAN_POINT('Ctrl Pts',(-0.0018496289474859,-0.036461326404273,
-0.0104938243014308));
#28263=CARTESIAN_POINT('Ctrl Pts',(-0.00183696178642117,-0.0364601257498979,
-0.0104801023038875));
#28264=CARTESIAN_POINT('Ctrl Pts',(-0.00150575505816513,-0.0364287323851718,
-0.0101213148938081));
#28265=CARTESIAN_POINT('Ctrl Pts',(-0.00109127169274443,-0.0363979570343344,
-0.00988588654905173));
#28266=CARTESIAN_POINT('Ctrl Pts',(-0.000677447847037822,-0.0363709454072252,
-0.00976939023582496));
#28267=CARTESIAN_POINT('Ctrl Pts',(-0.000632903748404836,-0.0363680378691636,
-0.00975685054455151));
#28268=CARTESIAN_POINT('Ctrl Pts',(-0.000588359671639667,-0.0363651739391918,
-0.00974564601115946));
#28269=CARTESIAN_POINT('Ctrl Pts',(-0.000543903940809233,-0.0363623575405296,
-0.00973573679278732));
#28270=CARTESIAN_POINT('Ctrl Pts',(-0.000213584020162325,-0.0363414308216289,
-0.00966210821520658));
#28271=CARTESIAN_POINT('Ctrl Pts',(0.000111819203387214,-0.0363215057164393,
-0.00966046320090738));
#28272=CARTESIAN_POINT('Ctrl Pts',(0.000407302089605617,-0.0363024018203738,
-0.00970925542557571));
#28273=CARTESIAN_POINT('Ctrl Pts',(0.000535161797734825,-0.0362941352889129,
-0.00973036852516975));
#28274=CARTESIAN_POINT('Ctrl Pts',(0.000657857796727303,-0.0362860225221071,
-0.00976084731948529));
#28275=CARTESIAN_POINT('Ctrl Pts',(0.000774427030647227,-0.0362780489031766,
-0.00979882514743081));
#28276=CARTESIAN_POINT('Ctrl Pts',(0.00116038694429653,-0.0362516483069783,
-0.00992456946865118));
#28277=CARTESIAN_POINT('Ctrl Pts',(0.00147418571268115,-0.0362274269837356,
-0.0101303574594857));
#28278=CARTESIAN_POINT('Ctrl Pts',(0.00171277270765056,-0.0362072415087562,
-0.0103547520669859));
#28279=CARTESIAN_POINT('Ctrl Pts',(0.00195135970261997,-0.0361870560337768,
-0.010579146674486));
#28280=CARTESIAN_POINT('Ctrl Pts',(0.0021156417199298,-0.0361696226856249,
-0.0108208939642838));
#28281=CARTESIAN_POINT('Ctrl Pts',(0.00222838256833176,-0.036153701563077,
-0.0110425787703198));
#28282=CARTESIAN_POINT('Ctrl Pts',(0.0022487466239749,-0.0361508257764383,
-0.0110826210601318));
#28283=CARTESIAN_POINT('Ctrl Pts',(0.00226743126048375,-0.0361480335409641,
-0.0111220294032082));
#28284=CARTESIAN_POINT('Ctrl Pts',(0.00228460794597736,-0.0361453234122333,
-0.0111606850575551));
#28285=CARTESIAN_POINT('Ctrl Pts',(0.00236252597684173,-0.0361330295448181,
-0.011336037425135));
#28286=CARTESIAN_POINT('Ctrl Pts',(0.0024096912660948,-0.0361224252468084,
-0.0114954903342938));
#28287=CARTESIAN_POINT('Ctrl Pts',(0.00244008456321309,-0.0361133756872451,
-0.0116318061154698));
#28288=CARTESIAN_POINT('Ctrl Pts',(0.00247717792833776,-0.0361023311922766,
-0.011798172108068));
#28289=CARTESIAN_POINT('Ctrl Pts',(0.00248947351924683,-0.0360934332308427,
-0.011929701616968));
#28290=CARTESIAN_POINT('Ctrl Pts',(0.00249509674334778,-0.0360874750694145,
-0.0120193533142409));
#28291=CARTESIAN_POINT('Ctrl Pts',(0.00249790835539826,-0.0360844959887004,
-0.0120641791628773));
#28292=CARTESIAN_POINT('Ctrl Pts',(0.00249896338344871,-0.0360822056816631,
-0.0120985365347907));
#28293=CARTESIAN_POINT('Ctrl Pts',(0.00249951757551438,-0.036080381945129,
-0.0121267422929342));
#28294=CARTESIAN_POINT('Ctrl Pts',(0.00249979467154721,-0.036079470076862,
-0.0121408451720059));
#28295=CARTESIAN_POINT('Ctrl Pts',(0.00249990418587905,-0.0360786573716534,
-0.0121534104681674));
#28296=CARTESIAN_POINT('Ctrl Pts',(0.00249993888064981,-0.0360783128037313,
-0.0121583720676249));
#28297=CARTESIAN_POINT('Ctrl Pts',(0.00249995622803519,-0.0360781405197703,
-0.0121608528673536));
#28298=CARTESIAN_POINT('Ctrl Pts',(0.00249995904440589,-0.0360780869820338,
-0.0121614328520031));
#28299=CARTESIAN_POINT('Ctrl Pts',(0.00249996804958266,-0.0360779674293166,
-0.0121632140197337));
#28300=CARTESIAN_POINT('Ctrl Pts',(0.00249997705475943,-0.0360778478765993,
-0.0121649951874644));
#28301=CARTESIAN_POINT('Ctrl Pts',(0.00249999820891719,-0.0360776647581573,
-0.0121679775971263));
#28302=CARTESIAN_POINT('Ctrl Pts',(0.00249999993021469,-0.0360772118286501,
-0.0121752625865014));
#28303=CARTESIAN_POINT('Ctrl Pts',(0.00250000337280969,-0.0360763059696357,
-0.0121898325652517));
#28304=CARTESIAN_POINT('Ctrl Pts',(0.00249978451240064,-0.0360742615648602,
-0.0122216107223804));
#28305=CARTESIAN_POINT('Ctrl Pts',(0.00249879466416602,-0.0360721820404578,
-0.0122534756179804));
#28306=CARTESIAN_POINT('Ctrl Pts',(0.0024978048159314,-0.0360701025160554,
-0.0122853405135803));
#28307=CARTESIAN_POINT('Ctrl Pts',(0.00249625951962489,-0.0360680761960123,
-0.0123173047059828));
#28308=CARTESIAN_POINT('Ctrl Pts',(0.00249367707095277,-0.0360658038812438,
-0.0123535459026242));
#28309=CARTESIAN_POINT('Ctrl Pts',(0.00248851217360852,-0.0360612592517069,
-0.0124260282959072));
#28310=CARTESIAN_POINT('Ctrl Pts',(0.00247902399267083,-0.0360556680737251,
-0.0125156086507209));
#28311=CARTESIAN_POINT('Ctrl Pts',(0.00246044666945603,-0.0360491838802819,
-0.0126188004467959));
#28312=CARTESIAN_POINT('Ctrl Pts',(0.00242329202302643,-0.0360362154933956,
-0.0128251840389459));
#28313=CARTESIAN_POINT('Ctrl Pts',(0.00235115394115315,-0.0360202690307048,
-0.0130862258480166));
#28314=CARTESIAN_POINT('Ctrl Pts',(0.00219473351942376,-0.0359993653520514,
-0.0133729935367869));
#28315=CARTESIAN_POINT('Ctrl Pts',(0.00216711349913969,-0.0359956742737252,
-0.0134236296960113));
#28316=CARTESIAN_POINT('Ctrl Pts',(0.00213682075988632,-0.0359918576501639,
-0.0134749978775204));
#28317=CARTESIAN_POINT('Ctrl Pts',(0.00210360074943439,-0.0359879202945817,
-0.0135267285165401));
#28318=CARTESIAN_POINT('Ctrl Pts',(0.00204275334083118,-0.0359807084400197,
-0.0136214809048422));
#28319=CARTESIAN_POINT('Ctrl Pts',(0.00197204693864971,-0.035973091536877,
-0.0137175048015559));
#28320=CARTESIAN_POINT('Ctrl Pts',(0.00189014621722043,-0.0359650991627008,
-0.0138121134362676));
#28321=CARTESIAN_POINT('Ctrl Pts',(0.00176353130196833,-0.035952743303542,
-0.0139583742268576));
#28322=CARTESIAN_POINT('Ctrl Pts',(0.00160994696874169,-0.0359387633021856,
-0.0141014178695565));
#28323=CARTESIAN_POINT('Ctrl Pts',(0.00142683534628718,-0.0359240898023569,
-0.014228690565688));
#28324=CARTESIAN_POINT('Ctrl Pts',(0.00133527953505993,-0.0359167530524426,
-0.0142923269137538));
#28325=CARTESIAN_POINT('Ctrl Pts',(0.00123634479103978,-0.0359093187201582,
-0.0143520079338338));
#28326=CARTESIAN_POINT('Ctrl Pts',(0.00113005941135025,-0.0359018750126493,
-0.0144058680234643));
#28327=CARTESIAN_POINT('Ctrl Pts',(0.00102377403166072,-0.0358944313051404,
-0.0144597281130948));
#28328=CARTESIAN_POINT('Ctrl Pts',(0.00091009824057508,-0.0358869588257101,
-0.0145077245907675));
#28329=CARTESIAN_POINT('Ctrl Pts',(0.000790462296476036,-0.0358793314169019,
-0.0145475972351853));
#28330=CARTESIAN_POINT('Ctrl Pts',(0.000670826352376991,-0.0358717040080937,
-0.0145874698796031));
#28331=CARTESIAN_POINT('Ctrl Pts',(0.000545326692536426,-0.0358638733479101,
-0.0146194111130419));
#28332=CARTESIAN_POINT('Ctrl Pts',(0.000411691870729785,-0.035855223196561,
-0.0146417222619043));
#28333=CARTESIAN_POINT('Ctrl Pts',(0.000350001179416516,-0.0358512299722691,
-0.0146520218992197));
#28334=CARTESIAN_POINT('Ctrl Pts',(0.000286547210286716,-0.0358471431795319,
-0.0146601474951376));
#28335=CARTESIAN_POINT('Ctrl Pts',(0.000224935218740908,-0.035843185019992,
-0.0146657135531935));
#28336=CARTESIAN_POINT('Ctrl Pts',(0.000183610600758106,-0.0358405301888983,
-0.0146694468398));
#28337=CARTESIAN_POINT('Ctrl Pts',(0.000144070717888571,-0.0358379940330427,
-0.0146721604783673));
#28338=CARTESIAN_POINT('Ctrl Pts',(9.60857070035578E-5,-0.0358349189925652,
-0.0146740061115289));
#28339=CARTESIAN_POINT('Ctrl Pts',(7.25285662780407E-5,-0.0358334093719581,
-0.0146749121828064));
#28340=CARTESIAN_POINT('Ctrl Pts',(4.77410863304185E-5,-0.0358318215863145,
-0.014675480515774));
#28341=CARTESIAN_POINT('Ctrl Pts',(2.73585790620338E-5,-0.0358305161258757,
-0.0146757035837062));
#28342=CARTESIAN_POINT('Ctrl Pts',(-1.52019121188965E-6,-0.0358286664961114,
-0.0146760196354797));
#28343=CARTESIAN_POINT('Ctrl Pts',(-1.68475855919575E-5,-0.0358276849859516,
-0.014675810629484));
#28344=CARTESIAN_POINT('Ctrl Pts',(-2.52470137588822E-5,-0.0358271470645206,
-0.0146757258009668));
#28345=CARTESIAN_POINT('Ctrl Pts',(-3.50302907154595E-5,-0.0358265205177801,
-0.0146756269965172));
#28346=CARTESIAN_POINT('Ctrl Pts',(-4.32145297488147E-5,-0.0358259963827926,
-0.0146755160720884));
#28347=CARTESIAN_POINT('Ctrl Pts',(-5.66846306278233E-5,-0.0358251336424485,
-0.0146752105744724));
#28348=CARTESIAN_POINT('Ctrl Pts',(-8.5164457235402E-5,-0.0358233095510309,
-0.0146745646610373));
#28349=CARTESIAN_POINT('Ctrl Pts',(-0.000113918265205585,-0.0358214675091151,
-0.0146734044237407));
#28350=CARTESIAN_POINT('Ctrl Pts',(-0.000141060502960187,-0.03581972767307,
-0.0146718705009428));
#28351=CARTESIAN_POINT('Ctrl Pts',(-0.000196336952449102,-0.0358161844147676,
-0.0146687465946965));
#28352=CARTESIAN_POINT('Ctrl Pts',(-0.000256766630260332,-0.0358123068140234,
-0.0146634154854298));
#28353=CARTESIAN_POINT('Ctrl Pts',(-0.000318665857405779,-0.0358083202692532,
-0.0146554605279017));
#28354=CARTESIAN_POINT('Ctrl Pts',(-0.000375972893758019,-0.0358046294789704,
-0.0146480957341674));
#28355=CARTESIAN_POINT('Ctrl Pts',(-0.000434357639183018,-0.0358008573708011,
-0.0146385946235638));
#28356=CARTESIAN_POINT('Ctrl Pts',(-0.000494476682713578,-0.0357969283946965,
-0.0146264639880471));
#28357=CARTESIAN_POINT('Ctrl Pts',(-0.000554595726244137,-0.0357929994185919,
-0.0146143333525305));
#28358=CARTESIAN_POINT('Ctrl Pts',(-0.000616439893323082,-0.0357886737530282,
-0.0145995489705675));
#28359=CARTESIAN_POINT('Ctrl Pts',(-0.00067953737948281,-0.0357842438436293,
-0.0145817271298603));
#28360=CARTESIAN_POINT('Ctrl Pts',(-0.000805732351802272,-0.0357753840248316,
-0.0145460834484459));
#28361=CARTESIAN_POINT('Ctrl Pts',(-0.000936956447855169,-0.035766127875995,
-0.0144983096416178));
#28362=CARTESIAN_POINT('Ctrl Pts',(-0.00107006174729965,-0.0357566455349307,
-0.0144352708789845));
#28363=CARTESIAN_POINT('Ctrl Pts',(-0.00120316704674414,-0.0357471631938664,
-0.0143722321163512));
#28364=CARTESIAN_POINT('Ctrl Pts',(-0.00133814273401691,-0.0357374711033914,
-0.0142939274948216));
#28365=CARTESIAN_POINT('Ctrl Pts',(-0.00147068513453818,-0.0357275803340383,
-0.0141975073704825));
#28366=CARTESIAN_POINT('Ctrl Pts',(-0.00168843994722776,-0.0357113307216925,
-0.0140390980913961));
#28367=CARTESIAN_POINT('Ctrl Pts',(-0.00189902193339737,-0.0356930246745004,
-0.013831540748202));
#28368=CARTESIAN_POINT('Ctrl Pts',(-0.00207353224951405,-0.0356730902563284,
-0.0135724434233646));
#28369=CARTESIAN_POINT('Ctrl Pts',(-0.00211146285195289,-0.0356687574208413,
-0.0135161274539705));
#28370=CARTESIAN_POINT('Ctrl Pts',(-0.00214768961790324,-0.035664347656259,
-0.0134573905581797));
#28371=CARTESIAN_POINT('Ctrl Pts',(-0.0021818901138409,-0.0356598653581442,
-0.0133962448348422));
#28372=CARTESIAN_POINT('Ctrl Pts',(-0.00235982569966132,-0.0356365452185082,
-0.0130781207900241));
#28373=CARTESIAN_POINT('Ctrl Pts',(-0.00248175197454682,-0.0356095958898492,
-0.0126936817681841));
#28374=CARTESIAN_POINT('Ctrl Pts',(-0.00249811171657688,-0.0355834167713905,
-0.0122730018918044));
#28375=CARTESIAN_POINT('Ctrl Pts',(-0.00249936339852753,-0.035581413810097,
-0.0122408157236303));
#28376=CARTESIAN_POINT('Ctrl Pts',(-0.0024999991528398,-0.0355794153574309,
-0.0122084456346896));
#28377=CARTESIAN_POINT('Ctrl Pts',(-0.00249999999915379,-0.0355774233837539,
-0.0121759183329917));
#28378=CARTESIAN_POINT('',(-0.00249999995263966,-0.0345787968006169,-0.0121755152554376));
#28379=CARTESIAN_POINT('Ctrl Pts',(-0.00249999969813745,-0.0355787743898623,
-0.0121746247456977));
#28380=CARTESIAN_POINT('Ctrl Pts',(-0.00249976104754906,-0.0355478566406557,
-0.0116889865238204));
#28381=CARTESIAN_POINT('Ctrl Pts',(-0.00235373123316885,-0.0355169388914492,
-0.0112034440484873));
#28382=CARTESIAN_POINT('Ctrl Pts',(-0.00208626723826142,-0.0354860211422426,
-0.0107983595440833));
#28383=CARTESIAN_POINT('Ctrl Pts',(-0.00199329640523685,-0.0354752740923454,
-0.0106575516426953));
#28384=CARTESIAN_POINT('Ctrl Pts',(-0.00188610159089402,-0.0354645270424482,
-0.0105263190663315));
#28385=CARTESIAN_POINT('Ctrl Pts',(-0.00176700773165438,-0.035453779992551,
-0.0104073274382105));
#28386=CARTESIAN_POINT('Ctrl Pts',(-0.0014307039947812,-0.0354234318867471,
-0.0100713123871473));
#28387=CARTESIAN_POINT('Ctrl Pts',(-0.000994187377721932,-0.0353930837809432,
-0.00983297432017851));
#28388=CARTESIAN_POINT('Ctrl Pts',(-0.00052798611458786,-0.0353627356751393,
-0.00973224311658367));
#28389=CARTESIAN_POINT('Ctrl Pts',(-0.000354141435614634,-0.0353514189818394,
-0.00969468083364645));
#28390=CARTESIAN_POINT('Ctrl Pts',(-0.000176433514161334,-0.0353401022885395,
-0.00967578830322123));
#28391=CARTESIAN_POINT('Ctrl Pts',(9.18400352385882E-7,-0.0353287855952396,
-0.00967585345524994));
#28392=CARTESIAN_POINT('Ctrl Pts',(0.000478284169225964,-0.035298325241806,
-0.00967602882041791));
#28393=CARTESIAN_POINT('Ctrl Pts',(0.000957129060230269,-0.0352678648883724,
-0.00981724964416271));
#28394=CARTESIAN_POINT('Ctrl Pts',(0.00135889541973528,-0.0352374045349388,
-0.0100774245319366));
#28395=CARTESIAN_POINT('Ctrl Pts',(0.00150667996061326,-0.0352262000892686,
-0.0101731264876329));
#28396=CARTESIAN_POINT('Ctrl Pts',(0.00164417755205256,-0.0352149956435984,
-0.0102844212731613));
#28397=CARTESIAN_POINT('Ctrl Pts',(0.00176830662644891,-0.0352037911979283,
-0.010408626171879));
#28398=CARTESIAN_POINT('Ctrl Pts',(0.00210569993998899,-0.0351733365677829,
-0.0107462255823322));
#28399=CARTESIAN_POINT('Ctrl Pts',(0.00234443692751372,-0.0351428819376375,
-0.0111845771105222));
#28400=CARTESIAN_POINT('Ctrl Pts',(0.00244461252497621,-0.0351124273074921,
-0.0116525277638388));
#28401=CARTESIAN_POINT('Ctrl Pts',(0.00248148656901149,-0.0351012171385337,
-0.0118247776274166));
#28402=CARTESIAN_POINT('Ctrl Pts',(0.00250004266924381,-0.0350900069695753,
-0.0120007831749893));
#28403=CARTESIAN_POINT('Ctrl Pts',(0.002499999926004,-0.0350787968006169,
-0.0121764615463884));
#28404=CARTESIAN_POINT('Ctrl Pts',(0.00249988380558114,-0.0350483421704715,
-0.0126537264159345));
#28405=CARTESIAN_POINT('Ctrl Pts',(0.00235877985707804,-0.0350178875403261,
-0.0131325050088043));
#28406=CARTESIAN_POINT('Ctrl Pts',(0.00209874525723065,-0.0349874329101807,
-0.0135342598329395));
#28407=CARTESIAN_POINT('Ctrl Pts',(0.00200302806134313,-0.0349762227412224,
-0.0136821434039069));
#28408=CARTESIAN_POINT('Ctrl Pts',(0.00189169940591702,-0.034965012572264,
-0.0138197327684265));
#28409=CARTESIAN_POINT('Ctrl Pts',(0.00176744647050627,-0.0349538024033056,
-0.0139439406638941));
#28410=CARTESIAN_POINT('Ctrl Pts',(0.00142982548175629,-0.034923342049872,
-0.0142814392697798));
#28411=CARTESIAN_POINT('Ctrl Pts',(0.000991409298149122,-0.0348928816964383,
-0.0145202525210834));
#28412=CARTESIAN_POINT('Ctrl Pts',(0.000523371442888126,-0.0348624213430047,
-0.0146204559808152));
#28413=CARTESIAN_POINT('Ctrl Pts',(0.00035120979242438,-0.0348512168973345,
-0.0146573145229517));
#28414=CARTESIAN_POINT('Ctrl Pts',(0.000175294693721739,-0.0348400124516644,
-0.0146758742078257));
#28415=CARTESIAN_POINT('Ctrl Pts',(-2.98119298794901E-7,-0.0348288080059942,
-0.0146758532687831));
#28416=CARTESIAN_POINT('Ctrl Pts',(-0.000475904804791021,-0.0347984599001903,
-0.01467579655377));
#28417=CARTESIAN_POINT('Ctrl Pts',(-0.000953174036178508,-0.0347681117943864,
-0.0145356965291672));
#28418=CARTESIAN_POINT('Ctrl Pts',(-0.00135403976161624,-0.0347377636885825,
-0.0142774184946738));
#28419=CARTESIAN_POINT('Ctrl Pts',(-0.00150352106692448,-0.0347264469952826,
-0.0141811075973368));
#28420=CARTESIAN_POINT('Ctrl Pts',(-0.00164252270203225,-0.0347151303019828,
-0.0140688788299219));
#28421=CARTESIAN_POINT('Ctrl Pts',(-0.00176786810101232,-0.0347038136086829,
-0.0139435190856907));
#28422=CARTESIAN_POINT('Ctrl Pts',(-0.00211031774660788,-0.0346728958594764,
-0.0136010302481805));
#28423=CARTESIAN_POINT('Ctrl Pts',(-0.0023509863876243,-0.03464197811027,
-0.0131551955459422));
#28424=CARTESIAN_POINT('Ctrl Pts',(-0.00244882661909244,-0.0346110603610635,
-0.0126790909934365));
#28425=CARTESIAN_POINT('Ctrl Pts',(-0.0024828360109965,-0.0346003133111662,
-0.0125135964308164));
#28426=CARTESIAN_POINT('Ctrl Pts',(-0.00249999918825629,-0.0345895662612688,
-0.0123446738066878));
#28427=CARTESIAN_POINT('Ctrl Pts',(-0.0024999999999711,-0.0345788192113715,
-0.0121758653077954));
#28428=CARTESIAN_POINT('',(-0.00249999974521768,-0.0335786873852289,-0.0121765002461478));
#28429=CARTESIAN_POINT('Ctrl Pts',(-0.00249999990530822,-0.0345787743898623,
-0.0121751652030797));
#28430=CARTESIAN_POINT('Ctrl Pts',(-0.00249986624097334,-0.0345478522652573,
-0.0116895252552616));
#28431=CARTESIAN_POINT('Ctrl Pts',(-0.00235394043889903,-0.0345169301406521,
-0.0112039498211489));
#28432=CARTESIAN_POINT('Ctrl Pts',(-0.00208656242431829,-0.0344860080160471,
-0.0107988067189276));
#28433=CARTESIAN_POINT('Ctrl Pts',(-0.00199365631386498,-0.0344752634739855,
-0.010658031233466));
#28434=CARTESIAN_POINT('Ctrl Pts',(-0.00188653476899345,-0.0344645189319239,
-0.010526820863554));
#28435=CARTESIAN_POINT('Ctrl Pts',(-0.00176751944018786,-0.0344537743898623,
-0.0104078388554637));
#28436=CARTESIAN_POINT('Ctrl Pts',(-0.00143131032715907,-0.0344234218882755,
-0.0100717238708825));
#28437=CARTESIAN_POINT('Ctrl Pts',(-0.000994859168403589,-0.0343930693866886,
-0.00983325890923276));
#28438=CARTESIAN_POINT('Ctrl Pts',(-0.00052868382947506,-0.0343627168851018,
-0.00973239397475206));
#28439=CARTESIAN_POINT('Ctrl Pts',(-0.000354912823296572,-0.034351402720022,
-0.00969479567280601));
#28440=CARTESIAN_POINT('Ctrl Pts',(-0.000177276052050649,-0.0343400885549421,
-0.00967585243990393));
#28441=CARTESIAN_POINT('Ctrl Pts',(1.19393685333613E-8,-0.0343287743898623,
-0.0096758532865866));
#28442=CARTESIAN_POINT('Ctrl Pts',(0.000477381226344273,-0.0342983096365892,
-0.00967585556638174));
#28443=CARTESIAN_POINT('Ctrl Pts',(0.000956280028606871,-0.034267844883316,
-0.00981690472123153));
#28444=CARTESIAN_POINT('Ctrl Pts',(0.00135814207659454,-0.0342373801300428,
-0.0100769368756966));
#28445=CARTESIAN_POINT('Ctrl Pts',(0.00150590706314561,-0.0342261782166493,
-0.0101725509004591));
#28446=CARTESIAN_POINT('Ctrl Pts',(0.00164339823397583,-0.0342149763032558,
-0.0102837500288529));
#28447=CARTESIAN_POINT('Ctrl Pts',(0.0017675363272879,-0.0342037743898623,
-0.0104078557379971));
#28448=CARTESIAN_POINT('Ctrl Pts',(0.00210507912693486,-0.0341733153655019,
-0.0107453104821375));
#28449=CARTESIAN_POINT('Ctrl Pts',(0.00234400765423946,-0.0341428563411416,
-0.0111835611625902));
#28450=CARTESIAN_POINT('Ctrl Pts',(0.00244438608379509,-0.0341123973167812,
-0.0116514711040338));
#28451=CARTESIAN_POINT('Ctrl Pts',(0.002481321132023,-0.0341011896744749,
-0.0118236423198025));
#28452=CARTESIAN_POINT('Ctrl Pts',(0.0024999532541214,-0.0340899820321686,
-0.0119995743940331));
#28453=CARTESIAN_POINT('Ctrl Pts',(0.00249999991176641,-0.0340787743898623,
-0.0121751890818159));
#28454=CARTESIAN_POINT('Ctrl Pts',(0.00250012671331015,-0.0340483153655019,
-0.0126524573517198));
#28455=CARTESIAN_POINT('Ctrl Pts',(0.00235926456083444,-0.0340178563411416,
-0.0131313103708889));
#28456=CARTESIAN_POINT('Ctrl Pts',(0.00209943160156203,-0.0339873973167811,
-0.0135331988396));
#28457=CARTESIAN_POINT('Ctrl Pts',(0.00200382398023952,-0.0339761896744748,
-0.0136810769249592));
#28458=CARTESIAN_POINT('Ctrl Pts',(0.00189261111142232,-0.0339649820321686,
-0.0138186762224371));
#28459=CARTESIAN_POINT('Ctrl Pts',(0.00176847552760974,-0.0339537743898624,
-0.013942911380749));
#28460=CARTESIAN_POINT('Ctrl Pts',(0.00143104863353808,-0.0339233096365892,
-0.0142806089394681));
#28461=CARTESIAN_POINT('Ctrl Pts',(0.000992768245731332,-0.033892844883316,
-0.0145196779453882));
#28462=CARTESIAN_POINT('Ctrl Pts',(0.000524785733290654,-0.0338623801300428,
-0.0146201527637365));
#28463=CARTESIAN_POINT('Ctrl Pts',(0.000352708200706007,-0.0338511782166493,
-0.014657097432327));
#28464=CARTESIAN_POINT('Ctrl Pts',(0.00017686938043608,-0.0338399763032558,
-0.0146757588191865));
#28465=CARTESIAN_POINT('Ctrl Pts',(1.34034880432785E-6,-0.0338287743898623,
-0.0146758529272511));
#28466=CARTESIAN_POINT('Ctrl Pts',(-0.000474269935258941,-0.0337984218882755,
-0.014676107920758));
#28467=CARTESIAN_POINT('Ctrl Pts',(-0.000951633769556664,-0.0337680693866886,
-0.0145363186693901));
#28468=CARTESIAN_POINT('Ctrl Pts',(-0.00135267015008844,-0.0337377168851017,
-0.0142783003049297));
#28469=CARTESIAN_POINT('Ctrl Pts',(-0.00150216002983868,-0.0337264027200219,
-0.0141821216634175));
#28470=CARTESIAN_POINT('Ctrl Pts',(-0.00164118823616503,-0.0337150885549422,
-0.0140700299046978));
#28471=CARTESIAN_POINT('Ctrl Pts',(-0.00176657973183811,-0.0337037743898624,
-0.0139448066638574));
#28472=CARTESIAN_POINT('Ctrl Pts',(-0.00210928035767172,-0.0336728522652572,
-0.0136025658860874));
#28473=CARTESIAN_POINT('Ctrl Pts',(-0.00235027400587087,-0.033641930140652,
-0.0131569046615656));
#28474=CARTESIAN_POINT('Ctrl Pts',(-0.00244846038690231,-0.0336110080160469,
-0.0126808698543756));
#28475=CARTESIAN_POINT('Ctrl Pts',(-0.00248257730850229,-0.0336002634739854,
-0.0125154615561457));
#28476=CARTESIAN_POINT('Ctrl Pts',(-0.00249986307686693,-0.0335895189319238,
-0.012346615537031));
#28477=CARTESIAN_POINT('Ctrl Pts',(-0.00249999918675125,-0.0335787743898623,
-0.0121778697793265));
#28478=CARTESIAN_POINT('',(-0.00249999968131482,-0.032578830244044,-0.0121749483697152));
#28479=CARTESIAN_POINT('Ctrl Pts',(-0.00249999999989964,-0.0335786477078032,
-0.0121758756868695));
#28480=CARTESIAN_POINT('Ctrl Pts',(-0.00250000435121429,-0.03354777589403,
-0.011690244642358));
#28481=CARTESIAN_POINT('Ctrl Pts',(-0.00235422169308874,-0.0335168994267022,
-0.0112046356695078));
#28482=CARTESIAN_POINT('Ctrl Pts',(-0.00199404053235062,-0.0334752737185985,
-0.0106585233900779));
#28483=CARTESIAN_POINT('Ctrl Pts',(-0.00188687582372486,-0.0334645330462428,
-0.0105271995947348));
#28484=CARTESIAN_POINT('Ctrl Pts',(-0.00143164247358771,-0.033423465707693,
-0.0100719494622799));
#28485=CARTESIAN_POINT('Ctrl Pts',(-0.000995226297729509,-0.0333931293360795,
-0.00983341399802515));
#28486=CARTESIAN_POINT('Ctrl Pts',(-0.00035519762743697,-0.033351483030854,
-0.00969482912049473));
#28487=CARTESIAN_POINT('Ctrl Pts',(-0.000177459478791954,-0.0333401702097692,
-0.00967585823750568));
#28488=CARTESIAN_POINT('Ctrl Pts',(0.000477316285896267,-0.0332984171435253,
-0.00967583996630468));
#28489=CARTESIAN_POINT('Ctrl Pts',(0.000956234436266438,-0.0332679844914464,
-0.00981688305921691));
#28490=CARTESIAN_POINT('Ctrl Pts',(0.00150595431923458,-0.0332262951843495,
-0.010172578594861));
#28491=CARTESIAN_POINT('Ctrl Pts',(0.00164351146432768,-0.0332150772452965,
-0.0102838401306641));
#28492=CARTESIAN_POINT('Ctrl Pts',(0.00210504588375627,-0.0331733547444291,
-0.0107453400500872));
#28493=CARTESIAN_POINT('Ctrl Pts',(0.00234387620624605,-0.0331427945138748,
-0.011183365842278));
#28494=CARTESIAN_POINT('Ctrl Pts',(0.00248132798507893,-0.0331011467372314,
-0.0118235205721592));
#28495=CARTESIAN_POINT('Ctrl Pts',(0.00249999175449094,-0.033089942642566,
-0.0119997927455534));
#28496=CARTESIAN_POINT('Ctrl Pts',(0.00250002238124961,-0.0330484181473094,
-0.0126535268110293));
#28497=CARTESIAN_POINT('Ctrl Pts',(0.0023587575513812,-0.0330182784947822,
-0.0131328112098241));
#28498=CARTESIAN_POINT('Ctrl Pts',(0.00200285349422997,-0.0329770278050595,
-0.0136823131940857));
#28499=CARTESIAN_POINT('Ctrl Pts',(0.001891864930695,-0.0329659560479124,
-0.0138194872129651));
#28500=CARTESIAN_POINT('Ctrl Pts',(0.00143078271491195,-0.0329246669105755,
-0.0142806997828226));
#28501=CARTESIAN_POINT('Ctrl Pts',(0.000992831074572435,-0.0328943299887714,
-0.0145195833260247));
#28502=CARTESIAN_POINT('Ctrl Pts',(0.000352619070780477,-0.0328527049860756,
-0.0146571464594452));
#28503=CARTESIAN_POINT('Ctrl Pts',(0.000176261132541491,-0.0328414755467602,
-0.0146758372723657));
#28504=CARTESIAN_POINT('Ctrl Pts',(-0.000475416776196498,-0.0327998829768102,
-0.0146758965187131));
#28505=CARTESIAN_POINT('Ctrl Pts',(-0.000952748003858568,-0.0327694838534468,
-0.0145358755492953));
#28506=CARTESIAN_POINT('Ctrl Pts',(-0.00150323296627836,-0.0327276627470969,
-0.0141813287735633));
#28507=CARTESIAN_POINT('Ctrl Pts',(-0.00164229600481632,-0.0327162930278274,
-0.0140690810302145));
#28508=CARTESIAN_POINT('Ctrl Pts',(-0.00211018950912318,-0.0326738348307577,
-0.0136012254148823));
#28509=CARTESIAN_POINT('Ctrl Pts',(-0.00235090480190234,-0.0326426854238918,
-0.0131553983571458));
#28510=CARTESIAN_POINT('Ctrl Pts',(-0.002482824807499,-0.0326006178733433,
-0.0125137184272263));
#28511=CARTESIAN_POINT('Ctrl Pts',(-0.00250000167733419,-0.0325897556944878,
-0.0123447162660254));
#28512=CARTESIAN_POINT('Ctrl Pts',(-0.00249999999987668,-0.0325788860982257,
-0.0121758284556141));
#28513=CARTESIAN_POINT('',(-0.00249999999999741,-0.0315787642283226,-0.0121758496907437));
#28514=CARTESIAN_POINT('Ctrl Pts',(-0.00249999936275296,-0.0325787743898623,
-0.0121740682838162));
#28515=CARTESIAN_POINT('Ctrl Pts',(-0.00249965261591296,-0.032547853826465,
-0.0116884293216484));
#28516=CARTESIAN_POINT('Ctrl Pts',(-0.00235351427316652,-0.0325169332630677,
-0.0112029186931701));
#28517=CARTESIAN_POINT('Ctrl Pts',(-0.00208595935539751,-0.0324860126996704,
-0.0107978933569413));
#28518=CARTESIAN_POINT('Ctrl Pts',(-0.00199297357310003,-0.032475266596401,
-0.0106571312358277));
#28519=CARTESIAN_POINT('Ctrl Pts',(-0.00188577101279796,-0.0324645204931317,
-0.0105259441942091));
#28520=CARTESIAN_POINT('Ctrl Pts',(-0.00176667590864148,-0.0324537743898623,
-0.0104069959622309));
#28521=CARTESIAN_POINT('Ctrl Pts',(-0.0014303078820767,-0.0324234234734616,
-0.0100710427562847));
#28522=CARTESIAN_POINT('Ctrl Pts',(-0.000993744870917422,-0.032393072557061,
-0.00983278630991865));
#28523=CARTESIAN_POINT('Ctrl Pts',(-0.000527523167523132,-0.0323627216406603,
-0.00973214313440699));
#28524=CARTESIAN_POINT('Ctrl Pts',(-0.000353701451745077,-0.0323514058903943,
-0.00969462027924725));
#28525=CARTESIAN_POINT('Ctrl Pts',(-0.000176021369284442,-0.0323400901401283,
-0.00967576141850525));
#28526=CARTESIAN_POINT('Ctrl Pts',(1.29998489136426E-6,-0.0323287743898623,
-0.00967585362455026));
#28527=CARTESIAN_POINT('Ctrl Pts',(0.000478667387052929,-0.032298311221266,
-0.00967610185274799));
#28528=CARTESIAN_POINT('Ctrl Pts',(0.000957492025298925,-0.0322678480526696,
-0.00981739670095818));
#28529=CARTESIAN_POINT('Ctrl Pts',(0.00135921932706133,-0.0322373848840733,
-0.0100776343225453));
#28530=CARTESIAN_POINT('Ctrl Pts',(0.00150696334902196,-0.032226181386003,
-0.0101733424128595));
#28531=CARTESIAN_POINT('Ctrl Pts',(0.0016444216184737,-0.0322149778879326,
-0.0102846362907292));
#28532=CARTESIAN_POINT('Ctrl Pts',(0.00176851454323397,-0.0322037743898623,
-0.0104088342401497));
#28533=CARTESIAN_POINT('Ctrl Pts',(0.00210586927790242,-0.0321733169473757,
-0.0107464744912283));
#28534=CARTESIAN_POINT('Ctrl Pts',(0.00234455494301116,-0.0321428595048892,
-0.0111848556501687));
#28535=CARTESIAN_POINT('Ctrl Pts',(0.0024446749625898,-0.0321124020624027,
-0.011652819513952));
#28536=CARTESIAN_POINT('Ctrl Pts',(0.00248152204011029,-0.0321011928382226,
-0.0118250438187232));
#28537=CARTESIAN_POINT('Ctrl Pts',(0.00250005712607798,-0.0320899836140425,
-0.012001020313999));
#28538=CARTESIAN_POINT('Ctrl Pts',(0.00249999986716576,-0.0320787743898623,
-0.01217666825355));
#28539=CARTESIAN_POINT('Ctrl Pts',(0.00249984428458505,-0.0320483169473756,
-0.0126539347379028));
#28540=CARTESIAN_POINT('Ctrl Pts',(0.00235869983460178,-0.0320178595048889,
-0.0131327029367118));
#28541=CARTESIAN_POINT('Ctrl Pts',(0.00209863064063772,-0.0319874020624023,
-0.0135344368998026));
#28542=CARTESIAN_POINT('Ctrl Pts',(0.00200291761749952,-0.0319761928382223,
-0.0136822866759281));
#28543=CARTESIAN_POINT('Ctrl Pts',(0.00189159945511839,-0.0319649836140423,
-0.0138198445281878));
#28544=CARTESIAN_POINT('Ctrl Pts',(0.00176736211766683,-0.0319537743898623,
-0.0139440249821341));
#28545=CARTESIAN_POINT('Ctrl Pts',(0.00142972385689433,-0.031923311221266,
-0.0142815086513147));
#28546=CARTESIAN_POINT('Ctrl Pts',(0.000991294697778186,-0.0318928480526697,
-0.0145203012508883));
#28547=CARTESIAN_POINT('Ctrl Pts',(0.00052325059434184,-0.0318623848840733,
-0.0146204818504755));
#28548=CARTESIAN_POINT('Ctrl Pts',(0.000351117114756464,-0.031851181386003,
-0.0146573254621507));
#28549=CARTESIAN_POINT('Ctrl Pts',(0.000175232400223226,-0.0318399778879326,
-0.014675876435438));
#28550=CARTESIAN_POINT('Ctrl Pts',(-3.2994906170825E-7,-0.0318287743898623,
-0.0146758532647848));
#28551=CARTESIAN_POINT('Ctrl Pts',(-0.000475938384284838,-0.0317984234734617,
-0.0146757904941615));
#28552=CARTESIAN_POINT('Ctrl Pts',(-0.000953207210028182,-0.0317680725570609,
-0.0145356834111494));
#28553=CARTESIAN_POINT('Ctrl Pts',(-0.00135407034799732,-0.0317377216406602,
-0.0142773987875346));
#28554=CARTESIAN_POINT('Ctrl Pts',(-0.00150352439084073,-0.0317264058903942,
-0.0141811023772458));
#28555=CARTESIAN_POINT('Ctrl Pts',(-0.00164250217809006,-0.0317150901401283,
-0.0140688937794005));
#28556=CARTESIAN_POINT('Ctrl Pts',(-0.00176782878136625,-0.0317037743898623,
-0.013943558408962));
#28557=CARTESIAN_POINT('Ctrl Pts',(-0.00211028677936814,-0.031672853826465,
-0.0136010764544755));
#28558=CARTESIAN_POINT('Ctrl Pts',(-0.002350965451897,-0.0316419332630677,
-0.0131552461552842));
#28559=CARTESIAN_POINT('Ctrl Pts',(-0.00244881593451928,-0.0316110126996704,
-0.0126791429832979));
#28560=CARTESIAN_POINT('Ctrl Pts',(-0.00248282279842098,-0.0316002665964011,
-0.0125136785385756));
#28561=CARTESIAN_POINT('Ctrl Pts',(-0.00249998952627055,-0.0315895204931317,
-0.0123447869023314));
#28562=CARTESIAN_POINT('Ctrl Pts',(-0.00249999999519073,-0.0315787743898623,
-0.012176008355439));
#28563=CARTESIAN_POINT('',(-0.00249999796170874,-0.0305787743898623,-0.0121790456919423));
#28564=CARTESIAN_POINT('Ctrl Pts',(-0.00249999999999741,-0.0315787642283226,
-0.0121758496907437));
#28565=CARTESIAN_POINT('Ctrl Pts',(-0.00249999930148813,-0.0315478414143166,
-0.0116902091587184));
#28566=CARTESIAN_POINT('Ctrl Pts',(-0.00235420613190631,-0.0315169186003106,
-0.0112045933187037));
#28567=CARTESIAN_POINT('Ctrl Pts',(-0.00208693851711527,-0.0314859957863047,
-0.0107993767608662));
#28568=CARTESIAN_POINT('Ctrl Pts',(-0.00199408245578486,-0.0314752523570415,
-0.0106585934730142));
#28569=CARTESIAN_POINT('Ctrl Pts',(-0.00188701190510759,-0.0314645089277783,
-0.0105273690150605));
#28570=CARTESIAN_POINT('Ctrl Pts',(-0.00176804687751574,-0.0314537654985151,
-0.010408366302474));
#28571=CARTESIAN_POINT('Ctrl Pts',(-0.00143193718319067,-0.0314234122863254,
-0.0100721501374298));
#28572=CARTESIAN_POINT('Ctrl Pts',(-0.000995556008603784,-0.0313930590741356,
-0.00983355476771765));
#28573=CARTESIAN_POINT('Ctrl Pts',(-0.000529409695698544,-0.0313627058619459,
-0.00973255114107948));
#28574=CARTESIAN_POINT('Ctrl Pts',(-0.000355670992443751,-0.0313513928308664,
-0.00969490579533647));
#28575=CARTESIAN_POINT('Ctrl Pts',(-0.000178061926068187,-0.031340079799787,
-0.00967590981254358));
#28576=CARTESIAN_POINT('Ctrl Pts',(-7.95404688749067E-7,-0.0313287667687076,
-0.00967585341309182));
#28577=CARTESIAN_POINT('Ctrl Pts',(0.000476575028159227,-0.0312983013062999,
-0.00967570153201191));
#28578=CARTESIAN_POINT('Ctrl Pts',(0.000955520274846601,-0.0312678358438924,
-0.00981659668333524));
#28579=CARTESIAN_POINT('Ctrl Pts',(0.00135746673941968,-0.0312373703814847,
-0.010076500040587));
#28580=CARTESIAN_POINT('Ctrl Pts',(0.00150524438374116,-0.0312261696006231,
-0.0101720548203179));
#28581=CARTESIAN_POINT('Ctrl Pts',(0.00164275575461887,-0.0312149688197616,
-0.010283194175715));
#28582=CARTESIAN_POINT('Ctrl Pts',(0.00176692182567706,-0.0312037680389,
-0.0104072416101446));
#28583=CARTESIAN_POINT('Ctrl Pts',(0.00210458267841763,-0.0311733083071484,
-0.0107445798389603));
#28584=CARTESIAN_POINT('Ctrl Pts',(0.002343663667394,-0.031142848575397,
-0.0111827485478995));
#28585=CARTESIAN_POINT('Ctrl Pts',(0.00244420433014957,-0.0311123888436454,
-0.0116506245816322));
#28586=CARTESIAN_POINT('Ctrl Pts',(0.0024811944817488,-0.0311011823321278,
-0.0118227619531502));
#28587=CARTESIAN_POINT('Ctrl Pts',(0.0024998875048212,-0.0310899758206101,
-0.0119986655995088));
#28588=CARTESIAN_POINT('Ctrl Pts',(0.00249999949157442,-0.0310787693090925,
-0.0121742588814475));
#28589=CARTESIAN_POINT('Ctrl Pts',(0.0025003038759011,-0.031048309577341,
-0.0126515282133713));
#28590=CARTESIAN_POINT('Ctrl Pts',(0.00235961926287144,-0.0310178498455895,
-0.0131304345073108));
#28591=CARTESIAN_POINT('Ctrl Pts',(0.00209993488958646,-0.0309873901138379,
-0.0135324200779464));
#28592=CARTESIAN_POINT('Ctrl Pts',(0.00200439380130905,-0.0309761836023203,
-0.0136803155342825));
#28593=CARTESIAN_POINT('Ctrl Pts',(0.00189324748533952,-0.0309649770908026,
-0.0138179405156711));
#28594=CARTESIAN_POINT('Ctrl Pts',(0.00176917629465765,-0.0309537705792849,
-0.0139422097733471));
#28595=CARTESIAN_POINT('Ctrl Pts',(0.00143188255345838,-0.0309233051168773,
-0.0142800419695822));
#28596=CARTESIAN_POINT('Ctrl Pts',(0.000993695915477766,-0.0308928396544697,
-0.0145192849880158));
#28597=CARTESIAN_POINT('Ctrl Pts',(0.00052575226151233,-0.0308623741920621,
-0.0146199450523301));
#28598=CARTESIAN_POINT('Ctrl Pts',(0.000353710417751829,-0.0308511734112005,
-0.0146569532325051));
#28599=CARTESIAN_POINT('Ctrl Pts',(0.000177900980369277,-0.0308399726303389,
-0.014675684116494));
#28600=CARTESIAN_POINT('Ctrl Pts',(2.39340536966486E-6,-0.0308287718494774,
-0.01467585214088));
#28601=CARTESIAN_POINT('Ctrl Pts',(-0.000473217958759423,-0.0307984186372876,
-0.0146763074734057));
#28602=CARTESIAN_POINT('Ctrl Pts',(-0.000950641601993971,-0.0307680654250979,
-0.0145367186222503));
#28603=CARTESIAN_POINT('Ctrl Pts',(-0.00135178712369863,-0.0307377122129081,
-0.0142788681633962));
#28604=CARTESIAN_POINT('Ctrl Pts',(-0.00150129919925867,-0.0307263991818287,
-0.0141827639937085));
#28605=CARTESIAN_POINT('Ctrl Pts',(-0.00164035884141642,-0.0307150861507493,
-0.0140707462013264));
#28606=CARTESIAN_POINT('Ctrl Pts',(-0.00176579096747762,-0.0307037731196699,
-0.0139455940187487));
#28607=CARTESIAN_POINT('Ctrl Pts',(-0.00210864464456624,-0.0306728503056636,
-0.0136035055336064));
#28608=CARTESIAN_POINT('Ctrl Pts',(-0.00234983702321265,-0.0306419274916575,
-0.0131579511193642));
#28609=CARTESIAN_POINT('Ctrl Pts',(-0.00244823537039844,-0.0306110046776513,
-0.0126819595709787));
#28610=CARTESIAN_POINT('Ctrl Pts',(-0.00248242164084506,-0.0306002612483883,
-0.0125165871204365));
#28611=CARTESIAN_POINT('Ctrl Pts',(-0.00249978250656215,-0.0305895178191253,
-0.0123477703250945));
#28612=CARTESIAN_POINT('Ctrl Pts',(-0.00249999796170874,-0.0305787743898623,
-0.0121790456919423));
#28613=CARTESIAN_POINT('',(-0.0020225424859345,-0.0304787743898643,-0.0107063901558304));
#28614=CARTESIAN_POINT('Ctrl Pts',(-0.00249999827498751,-0.0305768133462266,
-0.0121787901317142));
#28615=CARTESIAN_POINT('Ctrl Pts',(-0.00250007190193453,-0.0305725335791676,
-0.0121161149715434));
#28616=CARTESIAN_POINT('Ctrl Pts',(-0.002497788617112,-0.0305683056341438,
-0.0120534556549794));
#28617=CARTESIAN_POINT('Ctrl Pts',(-0.0024931523602667,-0.0305641400813256,
-0.0119909443670962));
#28618=CARTESIAN_POINT('Ctrl Pts',(-0.00249014764196586,-0.030561440422268,
-0.0119504313375166));
#28619=CARTESIAN_POINT('Ctrl Pts',(-0.00248615576125712,-0.0305587677962322,
-0.0119099958863706));
#28620=CARTESIAN_POINT('Ctrl Pts',(-0.00248117998961982,-0.0305561228206165,
-0.0118696738308296));
#28621=CARTESIAN_POINT('Ctrl Pts',(-0.00247831465547303,-0.0305545996922453,
-0.0118464540830132));
#28622=CARTESIAN_POINT('Ctrl Pts',(-0.00247512344458627,-0.0305530859103769,
-0.0118232751292318));
#28623=CARTESIAN_POINT('Ctrl Pts',(-0.0024716072436851,-0.0305515813272362,
-0.0118001437804721));
#28624=CARTESIAN_POINT('Ctrl Pts',(-0.00246856976557504,-0.0305502815896833,
-0.0117801617124708));
#28625=CARTESIAN_POINT('Ctrl Pts',(-0.00246529001379808,-0.0305489888193277,
-0.0117602167955565));
#28626=CARTESIAN_POINT('Ctrl Pts',(-0.00246176867545611,-0.0305477028057356,
-0.0117403134048675));
#28627=CARTESIAN_POINT('Ctrl Pts',(-0.00245794692801323,-0.0305463070809629,
-0.0117187120348532));
#28628=CARTESIAN_POINT('Ctrl Pts',(-0.00245384094344368,-0.0305449194362869,
-0.0116971614306637));
#28629=CARTESIAN_POINT('Ctrl Pts',(-0.00244945174311329,-0.0305435394624721,
-0.0116756671630408));
#28630=CARTESIAN_POINT('Ctrl Pts',(-0.00244368591563245,-0.030541726674186,
-0.0116474314413576));
#28631=CARTESIAN_POINT('Ctrl Pts',(-0.00243743214261921,-0.0305399273839073,
-0.0116192967816556));
#28632=CARTESIAN_POINT('Ctrl Pts',(-0.00243069313014558,-0.0305381402891356,
-0.0115912757407499));
#28633=CARTESIAN_POINT('Ctrl Pts',(-0.00241542092603212,-0.0305340903075945,
-0.0115277734015189));
#28634=CARTESIAN_POINT('Ctrl Pts',(-0.00239766542416501,-0.0305301059677435,
-0.0114648911574963));
#28635=CARTESIAN_POINT('Ctrl Pts',(-0.00237746654675865,-0.0305261643904438,
-0.0114027732007691));
#28636=CARTESIAN_POINT('Ctrl Pts',(-0.00234285388810228,-0.0305194101304471,
-0.0112963282934916));
#28637=CARTESIAN_POINT('Ctrl Pts',(-0.00230113128439389,-0.0305127976518697,
-0.0111923267536372));
#28638=CARTESIAN_POINT('Ctrl Pts',(-0.0022525787066754,-0.0305061482064187,
-0.0110914690510435));
#28639=CARTESIAN_POINT('Ctrl Pts',(-0.0022055666684243,-0.0304997097432396,
-0.0109938114930916));
#28640=CARTESIAN_POINT('Ctrl Pts',(-0.00215225704739796,-0.0304932486502635,
-0.0108993215649116));
#28641=CARTESIAN_POINT('Ctrl Pts',(-0.00209299025559816,-0.03048655461756,
-0.0108085962551367));
#28642=CARTESIAN_POINT('Ctrl Pts',(-0.0020793513660387,-0.0304850141398324,
-0.0107877179109124));
#28643=CARTESIAN_POINT('Ctrl Pts',(-0.00206540128873714,-0.0304834616888587,
-0.0107670455075156));
#28644=CARTESIAN_POINT('Ctrl Pts',(-0.00205114477230131,-0.0304818945665418,
-0.0107465859487024));
#28645=CARTESIAN_POINT('Ctrl Pts',(-0.00204615281254276,-0.0304813458342075,
-0.0107394219760214));
#28646=CARTESIAN_POINT('Ctrl Pts',(-0.00204112342134774,-0.0304807953183517,
-0.0107322843006978));
#28647=CARTESIAN_POINT('Ctrl Pts',(-0.0020360568086995,-0.0304802429033023,
-0.0107251732144028));
#28648=CARTESIAN_POINT('Ctrl Pts',(-0.00203158097889193,-0.030479754901571,
-0.0107188913029537));
#28649=CARTESIAN_POINT('Ctrl Pts',(-0.00202707615544529,-0.0304792654235685,
-0.010712630216571));
#28650=CARTESIAN_POINT('Ctrl Pts',(-0.0020225424859383,-0.0304787743898724,
-0.0107063901558282));
#28651=CARTESIAN_POINT('',(-0.000393037172625865,-0.0304787744837451,-0.0097069422349132));
#28652=CARTESIAN_POINT('Origin',(1.00024155624823E-14,-0.0304787743898623,
-0.0121758532865681));
#28653=CARTESIAN_POINT('',(-0.00249999960057212,-0.0307038306106531,-0.012174809678307));
#28654=CARTESIAN_POINT('Ctrl Pts',(-0.000393037172625865,-0.0304787744837451,
-0.0097069422349132));
#28655=CARTESIAN_POINT('Ctrl Pts',(-0.000873042018136126,-0.0305097515278591,
-0.00978335638810855));
#28656=CARTESIAN_POINT('Ctrl Pts',(-0.00132989543511568,-0.0305407285719731,
-0.0100039314220522));
#28657=CARTESIAN_POINT('Ctrl Pts',(-0.00168811523538598,-0.0305717056160869,
-0.0103318720089802));
#28658=CARTESIAN_POINT('Ctrl Pts',(-0.00176354660113698,-0.0305782285406787,
-0.0104009273943567));
#28659=CARTESIAN_POINT('Ctrl Pts',(-0.00183469500662704,-0.0305847514652705,
-0.0104745810657172));
#28660=CARTESIAN_POINT('Ctrl Pts',(-0.00190103004203007,-0.0305912743898623,
-0.0105522508785471));
#28661=CARTESIAN_POINT('Ctrl Pts',(-0.00221605182441028,-0.030622251434176,
-0.0109211009549228));
#28662=CARTESIAN_POINT('Ctrl Pts',(-0.00242095374775302,-0.0306532284784897,
-0.0113849850894544));
#28663=CARTESIAN_POINT('Ctrl Pts',(-0.00248092016327206,-0.0306842055228035,
-0.0118675755814445));
#28664=CARTESIAN_POINT('Ctrl Pts',(-0.00249354752265257,-0.0306907284784897,
-0.0119691965224867));
#28665=CARTESIAN_POINT('Ctrl Pts',(-0.00249992035016284,-0.030697251434176,
-0.0120715766804667));
#28666=CARTESIAN_POINT('Ctrl Pts',(-0.00249999925703147,-0.0307037743898623,
-0.0121739258939954));
#28667=CARTESIAN_POINT('',(-0.00249999980101701,-0.0317037304164077,-0.0121765701516269));
#28668=CARTESIAN_POINT('Ctrl Pts',(-0.00249999999994761,-0.0307038959688732,
-0.0121758371019472));
#28669=CARTESIAN_POINT('Ctrl Pts',(-0.00250000314392324,-0.0307348003099762,
-0.012661479860859));
#28670=CARTESIAN_POINT('Ctrl Pts',(-0.00235421249077242,-0.0307657055154774,
-0.0131470991042038));
#28671=CARTESIAN_POINT('Ctrl Pts',(-0.00208694555713805,-0.0307966129601098,
-0.0135523191384926));
#28672=CARTESIAN_POINT('Ctrl Pts',(-0.00199403940976012,-0.0308073568690814,
-0.0136931799315364));
#28673=CARTESIAN_POINT('Ctrl Pts',(-0.00188690309448439,-0.030818101048622,
-0.0138244714868721));
#28674=CARTESIAN_POINT('Ctrl Pts',(-0.00176786054562226,-0.0308288455564767,
-0.0139435266419131));
#28675=CARTESIAN_POINT('Ctrl Pts',(-0.00143172188960472,-0.0308591846618166,
-0.0142797008938085));
#28676=CARTESIAN_POINT('Ctrl Pts',(-0.000995324916698483,-0.03088952638487,
-0.014518248219889));
#28677=CARTESIAN_POINT('Ctrl Pts',(-0.000529177622831193,-0.0309198668254454,
-0.0146192057055707));
#28678=CARTESIAN_POINT('Ctrl Pts',(-0.000355334125541598,-0.0309311818933828,
-0.014656856470939));
#28679=CARTESIAN_POINT('Ctrl Pts',(-0.000177617629157195,-0.0309424967829508,
-0.0146758356407072));
#28680=CARTESIAN_POINT('Ctrl Pts',(-2.48542410286077E-7,-0.0309538112918512,
-0.0146758532742034));
#28681=CARTESIAN_POINT('Ctrl Pts',(0.000477085134298968,-0.0309842607700137,
-0.0146759007292687));
#28682=CARTESIAN_POINT('Ctrl Pts',(0.000955967382520689,-0.0310147074911929,
-0.0145349217410522));
#28683=CARTESIAN_POINT('Ctrl Pts',(0.00135783874524607,-0.0310451659129698,
-0.0142749659423983));
#28684=CARTESIAN_POINT('Ctrl Pts',(0.00150570845889031,-0.0310563731760992,
-0.0141793144651534));
#28685=CARTESIAN_POINT('Ctrl Pts',(0.00164329361716952,-0.0310675820233643,
-0.0140680572997739));
#28686=CARTESIAN_POINT('Ctrl Pts',(0.00176750903723605,-0.0310787931749967,
-0.0139438781176306));
#28687=CARTESIAN_POINT('Ctrl Pts',(0.00210520254732306,-0.0311092719444186,
-0.0136062831243902));
#28688=CARTESIAN_POINT('Ctrl Pts',(0.00234418991460515,-0.0311397677450743,
-0.0131678179909039));
#28689=CARTESIAN_POINT('Ctrl Pts',(0.00244450605500945,-0.0311702266377108,
-0.0126996759159109));
#28690=CARTESIAN_POINT('Ctrl Pts',(0.00248137363267524,-0.0311814207046412,
-0.0125276271883695));
#28691=CARTESIAN_POINT('Ctrl Pts',(0.00249996619645104,-0.0311926097865355,
-0.0123518243035685));
#28692=CARTESIAN_POINT('Ctrl Pts',(0.00249999995374699,-0.0312037912059132,
-0.0121763341867927));
#28693=CARTESIAN_POINT('Ctrl Pts',(0.00250009171282573,-0.0312341845390259,
-0.0116993169676925));
#28694=CARTESIAN_POINT('Ctrl Pts',(0.00235933720099796,-0.0312645212567865,
-0.0112206806977134));
#28695=CARTESIAN_POINT('Ctrl Pts',(0.00209969662614369,-0.0312948701586445,
-0.0108189177397613));
#28696=CARTESIAN_POINT('Ctrl Pts',(0.00200391124991896,-0.0313060663323708,
-0.0106707012443148));
#28697=CARTESIAN_POINT('Ctrl Pts',(0.00189245071359453,-0.0313172641643344,
-0.0105328053465568));
#28698=CARTESIAN_POINT('Ctrl Pts',(0.00176801705468482,-0.0313284671088737,
-0.0104083364706993));
#28699=CARTESIAN_POINT('Ctrl Pts',(0.00143048434324852,-0.0313588556731862,
-0.0100707082314775));
#28700=CARTESIAN_POINT('Ctrl Pts',(0.000992115626683919,-0.0313892818555032,
-0.0098317474532645));
#28701=CARTESIAN_POINT('Ctrl Pts',(0.000524080923154784,-0.0314197271687171,
-0.00973140259448324));
#28702=CARTESIAN_POINT('Ctrl Pts',(0.000351865041266604,-0.031430929685165,
-0.00969448016497607));
#28703=CARTESIAN_POINT('Ctrl Pts',(0.000175887412909158,-0.0314421347917672,
-0.00967586932025064));
#28704=CARTESIAN_POINT('Ctrl Pts',(2.2804493397338E-7,-0.0314533415675346,
-0.00967585329695899));
#28705=CARTESIAN_POINT('Ctrl Pts',(-0.00047537783123628,-0.031483684432076,
-0.00967580991315456));
#28706=CARTESIAN_POINT('Ctrl Pts',(-0.000952675722152286,-0.0315140395329462,
-0.00981580905674417));
#28707=CARTESIAN_POINT('Ctrl Pts',(-0.00135359513164503,-0.0315444118556672,
-0.0100740016696291));
#28708=CARTESIAN_POINT('Ctrl Pts',(-0.00150317654237353,-0.0315557436464764,
-0.0101703322896005));
#28709=CARTESIAN_POINT('Ctrl Pts',(-0.001642270366962,-0.0315670778345774,
-0.0102826000216382));
#28710=CARTESIAN_POINT('Ctrl Pts',(-0.00176769456660348,-0.0315784146788944,
-0.0104080139501928));
#28711=CARTESIAN_POINT('Ctrl Pts',(-0.0021101716270565,-0.0316093705002396,
-0.0107504629649284));
#28712=CARTESIAN_POINT('Ctrl Pts',(-0.00235088267097563,-0.0316403461260748,
-0.0111962655494278));
#28713=CARTESIAN_POINT('Ctrl Pts',(-0.00244877259416916,-0.0316713397992797,
-0.0116723527582108));
#28714=CARTESIAN_POINT('Ctrl Pts',(-0.00248282015087859,-0.0316821198552002,
-0.0118379428997785));
#28715=CARTESIAN_POINT('Ctrl Pts',(-0.00250000157476981,-0.0316929020944027,
-0.0120069670480985));
#28716=CARTESIAN_POINT('Ctrl Pts',(-0.00249999999989133,-0.0317036864429531,
-0.0121758765960527));
#28717=CARTESIAN_POINT('',(-0.00249999998015666,-0.0327037598573404,-0.0121760717152833));
#28718=CARTESIAN_POINT('Ctrl Pts',(-0.00249999960214269,-0.0317037743898623,
-0.0121772637072012));
#28719=CARTESIAN_POINT('Ctrl Pts',(-0.00249972562032444,-0.0317346929904582,
-0.0126629021158245));
#28720=CARTESIAN_POINT('Ctrl Pts',(-0.00235366036551277,-0.031765611591054,
-0.0131484341365877));
#28721=CARTESIAN_POINT('Ctrl Pts',(-0.00208616670586763,-0.0317965301916499,
-0.0135534992771266));
#28722=CARTESIAN_POINT('Ctrl Pts',(-0.00199318980764039,-0.0318072770466772,
-0.0136942940174477));
#28723=CARTESIAN_POINT('Ctrl Pts',(-0.00188599091826558,-0.0318180239017046,
-0.013825513267719));
#28724=CARTESIAN_POINT('Ctrl Pts',(-0.00176689483772362,-0.0318287707567319,
-0.0139444919247275));
#28725=CARTESIAN_POINT('Ctrl Pts',(-0.00143056933241676,-0.0318591197105435,
-0.0142804858277763));
#28726=CARTESIAN_POINT('Ctrl Pts',(-0.000994037072133453,-0.0318894686643551,
-0.0145187961010783));
#28727=CARTESIAN_POINT('Ctrl Pts',(-0.000527828984604696,-0.0319198176181668,
-0.0146194974020158));
#28728=CARTESIAN_POINT('Ctrl Pts',(-0.000353989560030296,-0.0319311341199783,
-0.0146570468497349));
#28729=CARTESIAN_POINT('Ctrl Pts',(-0.000176288435109386,-0.0319424506217898,
-0.0146759279515235));
#28730=CARTESIAN_POINT('Ctrl Pts',(1.05568559110729E-6,-0.0319537671236013,
-0.0146758530636637));
#28731=CARTESIAN_POINT('Ctrl Pts',(0.000478421868862688,-0.0319842283266928,
-0.0146756514842052));
#28732=CARTESIAN_POINT('Ctrl Pts',(0.000957259337678074,-0.0320146895297843,
-0.0145344041261251));
#28733=CARTESIAN_POINT('Ctrl Pts',(0.00135901157724633,-0.0320451507328759,
-0.0142742068156162));
#28734=CARTESIAN_POINT('Ctrl Pts',(0.0015067842549624,-0.0320563549854075,
-0.014178500931438));
#28735=CARTESIAN_POINT('Ctrl Pts',(0.00164427003901416,-0.0320675592379392,
-0.0140672041779086));
#28736=CARTESIAN_POINT('Ctrl Pts',(0.0017683879085218,-0.0320787634904709,
-0.0139429990657721));
#28737=CARTESIAN_POINT('Ctrl Pts',(0.00210576598572575,-0.03210921896953,
-0.0136053838450328));
#28738=CARTESIAN_POINT('Ctrl Pts',(0.00234448287598003,-0.032139674448589,
-0.0131670209427273));
#28739=CARTESIAN_POINT('Ctrl Pts',(0.00244463681756341,-0.032170129927648,
-0.0126990653183515));
#28740=CARTESIAN_POINT('Ctrl Pts',(0.00248150122990054,-0.0321813399042121,
-0.012526821382469));
#28741=CARTESIAN_POINT('Ctrl Pts',(0.00250004915629776,-0.0321925498807762,
-0.0123508229465227));
#28742=CARTESIAN_POINT('Ctrl Pts',(0.00249999990173367,-0.0322037598573404,
-0.0121751523360403));
#28743=CARTESIAN_POINT('Ctrl Pts',(0.00249986608599048,-0.0322342153363994,
-0.011697887056473));
#28744=CARTESIAN_POINT('Ctrl Pts',(0.0023587441528943,-0.0322646708154585,
-0.0112191133705348));
#28745=CARTESIAN_POINT('Ctrl Pts',(0.0020986943065755,-0.0322951262945174,
-0.0108173680243828));
#28746=CARTESIAN_POINT('Ctrl Pts',(0.00200297580951634,-0.0323063362710816,
-0.0106694946021195));
#28747=CARTESIAN_POINT('Ctrl Pts',(0.00189164762937877,-0.0323175462476457,
-0.0105319150538955));
#28748=CARTESIAN_POINT('Ctrl Pts',(0.0017673966851248,-0.0323287562242099,
-0.0104077161432884));
#28749=CARTESIAN_POINT('Ctrl Pts',(0.00142976589476869,-0.0323592174273014,
-0.0100702267455101));
#28750=CARTESIAN_POINT('Ctrl Pts',(0.000991342583344342,-0.0323896786303929,
-0.00983142577155676));
#28751=CARTESIAN_POINT('Ctrl Pts',(0.00052330153238317,-0.0324201398334844,
-0.0097312356260219));
#28752=CARTESIAN_POINT('Ctrl Pts',(0.000351146476182227,-0.0324313440860161,
-0.00969438364455593));
#28753=CARTESIAN_POINT('Ctrl Pts',(0.00017523882882955,-0.0324425483385477,
-0.00967582899443021));
#28754=CARTESIAN_POINT('Ctrl Pts',(-3.46215430472113E-7,-0.0324537525910794,
-0.00967585331053111));
#28755=CARTESIAN_POINT('Ctrl Pts',(-0.000475953346134224,-0.0324841015448911,
-0.00967591917554274));
#28756=CARTESIAN_POINT('Ctrl Pts',(-0.000953220233558734,-0.0325144504987029,
-0.00981602863242962));
#28757=CARTESIAN_POINT('Ctrl Pts',(-0.00135408116879281,-0.0325447994525146,
-0.0100743147576891));
#28758=CARTESIAN_POINT('Ctrl Pts',(-0.00150355398185469,-0.0325561159543261,
-0.0101706243511766));
#28759=CARTESIAN_POINT('Ctrl Pts',(-0.00164254774097299,-0.0325674324561375,
-0.0102828501979924));
#28760=CARTESIAN_POINT('Ctrl Pts',(-0.00176788634241805,-0.032578748957949,
-0.0104082057311071));
#28761=CARTESIAN_POINT('Ctrl Pts',(-0.00211033264092056,-0.0326096675585449,
-0.0107506982898004));
#28762=CARTESIAN_POINT('Ctrl Pts',(-0.00235099671033441,-0.0326405861591409,
-0.0111965357179675));
#28763=CARTESIAN_POINT('Ctrl Pts',(-0.00244883194213856,-0.0326715047597367,
-0.0116726414830778));
#28764=CARTESIAN_POINT('Ctrl Pts',(-0.00248283804307749,-0.032682251614764,
-0.0118381289093085));
#28765=CARTESIAN_POINT('Ctrl Pts',(-0.00249999942473484,-0.0326929984697912,
-0.0120070439058234));
#28766=CARTESIAN_POINT('Ctrl Pts',(-0.00249999999998548,-0.0327037453248185,
-0.0121758447668942));
#28767=CARTESIAN_POINT('',(-0.00249999963235903,-0.0337038344979968,-0.0121748826709929));
#28768=CARTESIAN_POINT('Ctrl Pts',(-0.00249999996032784,-0.0327037743898623,
-0.0121762986636724));
#28769=CARTESIAN_POINT('Ctrl Pts',(-0.00249991344322729,-0.0327346958161416,
-0.0126619382284563));
#28770=CARTESIAN_POINT('Ctrl Pts',(-0.00235403500626082,-0.0327656172424207,
-0.0131475274998857));
#28771=CARTESIAN_POINT('Ctrl Pts',(-0.002086696698559,-0.0327965386686998,
-0.0135526963742856));
#28772=CARTESIAN_POINT('Ctrl Pts',(-0.00199379624968891,-0.0328072839090873,
-0.0136934931445783));
#28773=CARTESIAN_POINT('Ctrl Pts',(-0.00188667695832345,-0.0328180291494749,
-0.0138247245135547));
#28774=CARTESIAN_POINT('Ctrl Pts',(-0.00176766084901072,-0.0328287743898623,
-0.013943726337112));
#28775=CARTESIAN_POINT('Ctrl Pts',(-0.00143147923482751,-0.0328591261823979,
-0.0142798675987047));
#28776=CARTESIAN_POINT('Ctrl Pts',(-0.000995047975805245,-0.0328894779749335,
-0.0145183673326568));
#28777=CARTESIAN_POINT('Ctrl Pts',(-0.000528881464056954,-0.032919829767469,
-0.0146192698284062));
#28778=CARTESIAN_POINT('Ctrl Pts',(-0.000355098798720773,-0.0329311446416001,
-0.0146568853675075));
#28779=CARTESIAN_POINT('Ctrl Pts',(-0.000177448203374564,-0.0329424595157312,
-0.0146758429789933));
#28780=CARTESIAN_POINT('Ctrl Pts',(-1.4527881610982E-7,-0.0329537743898623,
-0.0146758532823369));
#28781=CARTESIAN_POINT('Ctrl Pts',(0.000477223193183005,-0.0329842384343121,
-0.0146758810229475));
#28782=CARTESIAN_POINT('Ctrl Pts',(0.000956130225102326,-0.0330147024787618,
-0.0145348624432454));
#28783=CARTESIAN_POINT('Ctrl Pts',(0.00135800830274932,-0.0330451665232116,
-0.0142748562521739));
#28784=CARTESIAN_POINT('Ctrl Pts',(0.00150579197239822,-0.0330563691454285,
-0.0141792434999856));
#28785=CARTESIAN_POINT('Ctrl Pts',(0.00164330105990532,-0.0330675717676454,
-0.0140680423228023));
#28786=CARTESIAN_POINT('Ctrl Pts',(0.00176745536946942,-0.0330787743898623,
-0.0139439317681119));
#28787=CARTESIAN_POINT('Ctrl Pts',(0.0021050130607344,-0.0331092327066532,
-0.0136064930400484));
#28788=CARTESIAN_POINT('Ctrl Pts',(0.00234396153004447,-0.0331396910234439,
-0.0131682540553602));
#28789=CARTESIAN_POINT('Ctrl Pts',(0.00244436163814869,-0.0331701493402348,
-0.0127003494085143));
#28790=CARTESIAN_POINT('Ctrl Pts',(0.00248130785375645,-0.0331813576901106,
-0.0125281652715381));
#28791=CARTESIAN_POINT('Ctrl Pts',(0.0024999481909198,-0.0331925660399865,
-0.0123522187821387));
#28792=CARTESIAN_POINT('Ctrl Pts',(0.00249999989168001,-0.0332037743898623,
-0.0121765892212965));
#28793=CARTESIAN_POINT('Ctrl Pts',(0.00250014038677074,-0.0332342327066532,
-0.01169932175006));
#28794=CARTESIAN_POINT('Ctrl Pts',(0.00235929242057106,-0.0332646910234441,
-0.0112204653127318));
#28795=CARTESIAN_POINT('Ctrl Pts',(0.00209947166519535,-0.0332951493402349,
-0.0108185697026885));
#28796=CARTESIAN_POINT('Ctrl Pts',(0.00200386027763117,-0.0333063576901107,
-0.0106706762179027));
#28797=CARTESIAN_POINT('Ctrl Pts',(0.00189264067368614,-0.0333175660399865,
-0.0105330628179937));
#28798=CARTESIAN_POINT('Ctrl Pts',(0.00176849601540297,-0.0333287743898623,
-0.0104088156968323));
#28799=CARTESIAN_POINT('Ctrl Pts',(0.00143107360888865,-0.0333592384343121,
-0.0100711147985052));
#28800=CARTESIAN_POINT('Ctrl Pts',(0.000992796766610591,-0.0333897024787619,
-0.00983204084068172));
#28801=CARTESIAN_POINT('Ctrl Pts',(0.000524816137036575,-0.0334201665232118,
-0.00973156033719502));
#28802=CARTESIAN_POINT('Ctrl Pts',(0.000352724404221588,-0.0334313691454286,
-0.00969461038058061));
#28803=CARTESIAN_POINT('Ctrl Pts',(0.000176870514703275,-0.0334425717676454,
-0.00967594678850897));
#28804=CARTESIAN_POINT('Ctrl Pts',(1.32659061961387E-6,-0.0334537743898623,
-0.00967585363852665));
#28805=CARTESIAN_POINT('Ctrl Pts',(-0.000474282839167653,-0.033484126182398,
-0.00967560126288786));
#28806=CARTESIAN_POINT('Ctrl Pts',(-0.000951645230172061,-0.0335144779749335,
-0.00981539266180371));
#28807=CARTESIAN_POINT('Ctrl Pts',(-0.00135267984762792,-0.0335448297674692,
-0.0100734125074108));
#28808=CARTESIAN_POINT('Ctrl Pts',(-0.00150218193101796,-0.0335561446416002,
-0.0101695999755126));
#28809=CARTESIAN_POINT('Ctrl Pts',(-0.00164122048733436,-0.0335674595157313,
-0.0102817032164137));
#28810=CARTESIAN_POINT('Ctrl Pts',(-0.00176661971134624,-0.0335787743898623,
-0.0104069398360233));
#28811=CARTESIAN_POINT('Ctrl Pts',(-0.00210931224294895,-0.0336096958161413,
-0.0107491880003286));
#28812=CARTESIAN_POINT('Ctrl Pts',(-0.00235029576238914,-0.0336406172424204,
-0.0111948542068774));
#28813=CARTESIAN_POINT('Ctrl Pts',(-0.00244847155006307,-0.0336715386686993,
-0.0116708908438639));
#28814=CARTESIAN_POINT('Ctrl Pts',(-0.00248258777837945,-0.033682283909087,
-0.0118363142642324));
#28815=CARTESIAN_POINT('Ctrl Pts',(-0.00249986984268188,-0.0336930291494747,
-0.0120051756354036));
#28816=CARTESIAN_POINT('Ctrl Pts',(-0.00249999926483312,-0.0337037743898623,
-0.0121739360401313));
#28817=CARTESIAN_POINT('',(-0.00250011285302282,-0.03470351490128,-0.0121767698938277));
#28818=CARTESIAN_POINT('Ctrl Pts',(-0.00249999999988495,-0.0337038946061314,
-0.0121758293018544));
#28819=CARTESIAN_POINT('Ctrl Pts',(-0.00250000466247185,-0.033734778565668,
-0.0126618251857962));
#28820=CARTESIAN_POINT('Ctrl Pts',(-0.00235401049354569,-0.0337656732166077,
-0.0131477676332546));
#28821=CARTESIAN_POINT('Ctrl Pts',(-0.00208637960977751,-0.0337965745867032,
-0.013553176822952));
#28822=CARTESIAN_POINT('Ctrl Pts',(-0.00199358657942657,-0.0338072887155541,
-0.0136937403734454));
#28823=CARTESIAN_POINT('Ctrl Pts',(-0.00188661745613048,-0.0338180036521474,
-0.0138247680260886));
#28824=CARTESIAN_POINT('Ctrl Pts',(-0.00176777967268957,-0.0338287192309164,
-0.0139436075197097));
#28825=CARTESIAN_POINT('Ctrl Pts',(-0.00143185883991029,-0.0338590091441037,
-0.0142795331866852));
#28826=CARTESIAN_POINT('Ctrl Pts',(-0.000995819000972656,-0.0338893041884867,
-0.0145179579746008));
#28827=CARTESIAN_POINT('Ctrl Pts',(-0.00053009486265646,-0.033919615582755,
-0.01461900687088));
#28828=CARTESIAN_POINT('Ctrl Pts',(-0.000355871137815989,-0.0339309548361457,
-0.0146568084655417));
#28829=CARTESIAN_POINT('Ctrl Pts',(-0.000177759162184081,-0.0339422963776195,
-0.0146758524338922));
#28830=CARTESIAN_POINT('Ctrl Pts',(-1.19922745325362E-8,-0.0339536407945005,
-0.0146758532865293));
#28831=CARTESIAN_POINT('Ctrl Pts',(0.000475378078808354,-0.0339839817734889,
-0.0146758555669326));
#28832=CARTESIAN_POINT('Ctrl Pts',(0.000952534340723019,-0.0340143433205773,
-0.014535936885229));
#28833=CARTESIAN_POINT('Ctrl Pts',(0.00135340362296399,-0.0340446842363143,
-0.0142778282229805));
#28834=CARTESIAN_POINT('Ctrl Pts',(0.00150307914058896,-0.0340560128475831,
-0.0141814562899414));
#28835=CARTESIAN_POINT('Ctrl Pts',(0.00164226268650892,-0.0340673385826217,
-0.0140691239039628));
#28836=CARTESIAN_POINT('Ctrl Pts',(0.00176776271306561,-0.0340786592968838,
-0.013943624479415));
#28837=CARTESIAN_POINT('Ctrl Pts',(0.00211667616122357,-0.0341101329910108,
-0.013594712704954));
#28838=CARTESIAN_POINT('Ctrl Pts',(0.0023594874416597,-0.0341415678773693,
-0.0131392469395127));
#28839=CARTESIAN_POINT('Ctrl Pts',(0.00245403057651737,-0.0341731357263291,
-0.0126530680490265));
#28840=CARTESIAN_POINT('Ctrl Pts',(0.0024845703595109,-0.0341833329263505,
-0.0124960201805183));
#28841=CARTESIAN_POINT('Ctrl Pts',(0.0025,-0.0341935440003627,-0.0123359654368259));
#28842=CARTESIAN_POINT('Ctrl Pts',(0.0025,-0.0342037747380661,-0.0121758532865581));
#28843=CARTESIAN_POINT('Ctrl Pts',(0.00250000000000001,-0.034232937675464,
-0.0117194501658555));
#28844=CARTESIAN_POINT('Ctrl Pts',(0.00237063675736665,-0.0342622603896458,
-0.0112584460522841));
#28845=CARTESIAN_POINT('Ctrl Pts',(0.00212976212905734,-0.0342915473991,
-0.0108666117986602));
#28846=CARTESIAN_POINT('Ctrl Pts',(0.00202453898889524,-0.0343043410715692,
-0.0106954437894814));
#28847=CARTESIAN_POINT('Ctrl Pts',(0.00189872674918113,-0.0343171279306032,
-0.0105373403262591));
#28848=CARTESIAN_POINT('Ctrl Pts',(0.00175661849558318,-0.0343298916807547,
-0.0103970077449286));
#28849=CARTESIAN_POINT('Ctrl Pts',(0.0014136044427166,-0.0343607002056529,
-0.0100582797241931));
#28850=CARTESIAN_POINT('Ctrl Pts',(0.000969667592712359,-0.0343913740936313,
-0.00982187960567954));
#28851=CARTESIAN_POINT('Ctrl Pts',(0.000498228384675477,-0.0344219748273925,
-0.00972600258157551));
#28852=CARTESIAN_POINT('Ctrl Pts',(0.000327245261845305,-0.034433073202178,
-0.00969122958707377));
#28853=CARTESIAN_POINT('Ctrl Pts',(0.000152869457994301,-0.0344441619543187,
-0.00967448373110126));
#28854=CARTESIAN_POINT('Ctrl Pts',(-2.09597687845891E-5,-0.0344552440169733,
-0.00967594115048361));
#28855=CARTESIAN_POINT('Ctrl Pts',(-0.000498417069704019,-0.0344856831544058,
-0.0096799442490275));
#28856=CARTESIAN_POINT('Ctrl Pts',(-0.00097515733266665,-0.0345160718238225,
-0.00982503436728499));
#28857=CARTESIAN_POINT('Ctrl Pts',(-0.00137350204111084,-0.0345463934484738,
-0.0100869559355462));
#28858=CARTESIAN_POINT('Ctrl Pts',(-0.00152005468315037,-0.0345575488977853,
-0.0101833179482004));
#28859=CARTESIAN_POINT('Ctrl Pts',(-0.00165616134946322,-0.0345686952723593,
-0.0102949970394808));
#28860=CARTESIAN_POINT('Ctrl Pts',(-0.00177885400776298,-0.034579831746722,
-0.0104192433642744));
#28861=CARTESIAN_POINT('Ctrl Pts',(-0.00211985554664619,-0.0346107835163558,
-0.0107645630316637));
#28862=CARTESIAN_POINT('Ctrl Pts',(-0.0023572611775204,-0.0346416588109018,
-0.0112121927339843));
#28863=CARTESIAN_POINT('Ctrl Pts',(-0.00245193093994344,-0.0346724635377442,
-0.0116879653222178));
#28864=CARTESIAN_POINT('Ctrl Pts',(-0.00248390807885714,-0.034682868623848,
-0.0118486697092986));
#28865=CARTESIAN_POINT('Ctrl Pts',(-0.00250000157580861,-0.0346932656587147,
-0.012012385288373));
#28866=CARTESIAN_POINT('Ctrl Pts',(-0.00249999999988386,-0.0347036548700008,
-0.0121758773844318));
#28867=CARTESIAN_POINT('',(-0.00249999998223552,-0.0357037881422828,-0.0121756466480986));
#28868=CARTESIAN_POINT('Ctrl Pts',(-0.00249999927306645,-0.0347037743898623,
-0.0121777597668807));
#28869=CARTESIAN_POINT('Ctrl Pts',(-0.00249962892818142,-0.0347346957451935,
-0.0126633991581566));
#28870=CARTESIAN_POINT('Ctrl Pts',(-0.00235346674042249,-0.0347656171005246,
-0.0131489030560318));
#28871=CARTESIAN_POINT('Ctrl Pts',(-0.00208589171888402,-0.0347965384558557,
-0.0135539155990429));
#28872=CARTESIAN_POINT('Ctrl Pts',(-0.001992908184325,-0.0348072837671912,
-0.013694659296169));
#28873=CARTESIAN_POINT('Ctrl Pts',(-0.00188571114828099,-0.0348180290785268,
-0.0138258291141247));
#28874=CARTESIAN_POINT('Ctrl Pts',(-0.00176662425626108,-0.0348287743898623,
-0.0139447621980598));
#28875=CARTESIAN_POINT('Ctrl Pts',(-0.00143024572345875,-0.0348591261103602,
-0.0142807062771868));
#28876=CARTESIAN_POINT('Ctrl Pts',(-0.000993674819817364,-0.0348894778308581,
-0.0145189501297577));
#28877=CARTESIAN_POINT('Ctrl Pts',(-0.000527449318288785,-0.034919829551356,
-0.0146195793793591));
#28878=CARTESIAN_POINT('Ctrl Pts',(-0.000353643143028753,-0.0349311444975248,
-0.0146570933826369));
#28879=CARTESIAN_POINT('Ctrl Pts',(-0.000175979907123819,-0.0349424594436935,
-0.0146759468723011));
#28880=CARTESIAN_POINT('Ctrl Pts',(1.32451008204644E-6,-0.0349537743898623,
-0.0146758529356927));
#28881=CARTESIAN_POINT('Ctrl Pts',(0.000478692833169598,-0.0349842383622976,
-0.0146756000239945));
#28882=CARTESIAN_POINT('Ctrl Pts',(0.000957516810351806,-0.0350147023347329,
-0.0145342999583668));
#28883=CARTESIAN_POINT('Ctrl Pts',(0.00135924192416223,-0.0350451663071681,
-0.0142740576120707));
#28884=CARTESIAN_POINT('Ctrl Pts',(0.00150697064288591,-0.0350563690013995,
-0.0141783571764885));
#28885=CARTESIAN_POINT('Ctrl Pts',(0.00164441543894939,-0.0350675716956309,
-0.0140670740874734));
#28886=CARTESIAN_POINT('Ctrl Pts',(0.00176849761439238,-0.0350787743898623,
-0.0139428892759733));
#28887=CARTESIAN_POINT('Ctrl Pts',(0.0021058562184701,-0.0351092326347659,
-0.0136052516216866));
#28888=CARTESIAN_POINT('Ctrl Pts',(0.00234454622479179,-0.0351396908796696,
-0.0131668718932853));
#28889=CARTESIAN_POINT('Ctrl Pts',(0.00244467043999084,-0.0351701491245732,
-0.0126989081974757));
#28890=CARTESIAN_POINT('Ctrl Pts',(0.00248151545309635,-0.0351813575463362,
-0.0125267008201621));
#28891=CARTESIAN_POINT('Ctrl Pts',(0.00250005205495153,-0.0351925659680993,
-0.0123507418187357));
#28892=CARTESIAN_POINT('Ctrl Pts',(0.00249999988972694,-0.0352037743898623,
-0.0121751107467884));
#28893=CARTESIAN_POINT('Ctrl Pts',(0.00249985813371351,-0.0352342326347659,
-0.011697843356682));
#28894=CARTESIAN_POINT('Ctrl Pts',(0.0023587270467928,-0.0352646908796697,
-0.0112190703624375));
#28895=CARTESIAN_POINT('Ctrl Pts',(0.00209866872827452,-0.0352951491245732,
-0.0108173285098379));
#28896=CARTESIAN_POINT('Ctrl Pts',(0.00200296908024305,-0.0353063575463362,
-0.010669490309113));
#28897=CARTESIAN_POINT('Ctrl Pts',(0.00189166702651383,-0.0353175659680993,
-0.0105319415994415));
#28898=CARTESIAN_POINT('Ctrl Pts',(0.00176744762681308,-0.0353287743898623,
-0.0104077670651105));
#28899=CARTESIAN_POINT('Ctrl Pts',(0.00142982503833262,-0.0353592383622976,
-0.010070266418632));
#28900=CARTESIAN_POINT('Ctrl Pts',(0.000991406550564997,-0.0353897023347329,
-0.00983145246976956));
#28901=CARTESIAN_POINT('Ctrl Pts',(0.000523366478542818,-0.0354201663071682,
-0.00973124952947645));
#28902=CARTESIAN_POINT('Ctrl Pts',(0.00035125137352712,-0.0354313690013995,
-0.00969440131791859));
#28903=CARTESIAN_POINT('Ctrl Pts',(0.000175384892034823,-0.0354425716956309,
-0.00967584201682161));
#28904=CARTESIAN_POINT('Ctrl Pts',(-1.60569417170369E-7,-0.0354537743898623,
-0.0096758532917146));
#28905=CARTESIAN_POINT('Ctrl Pts',(-0.000475769978245463,-0.0354841261103602,
-0.0096758838390449));
#28906=CARTESIAN_POINT('Ctrl Pts',(-0.000953049059468749,-0.0355144778308581,
-0.00981595913017058));
#28907=CARTESIAN_POINT('Ctrl Pts',(-0.00135393008443228,-0.0355448295513561,
-0.0100742174174149));
#28908=CARTESIAN_POINT('Ctrl Pts',(-0.00150337621608888,-0.0355561444975248,
-0.0101704946158691));
#28909=CARTESIAN_POINT('Ctrl Pts',(-0.00164234917519774,-0.0355674594436935,
-0.0102826816354944));
#28910=CARTESIAN_POINT('Ctrl Pts',(-0.00176767473268967,-0.0355787743898623,
-0.0104079941181257));
#28911=CARTESIAN_POINT('Ctrl Pts',(-0.00211016298119799,-0.0356096957451935,
-0.0107504466358045));
#28912=CARTESIAN_POINT('Ctrl Pts',(-0.0023508805670986,-0.0356406171005249,
-0.0111962564868814));
#28913=CARTESIAN_POINT('Ctrl Pts',(-0.00244877235014627,-0.0356715384558562,
-0.011672351571408));
#28914=CARTESIAN_POINT('Ctrl Pts',(-0.00248279018910421,-0.0356822837671916,
-0.0118377967743644));
#28915=CARTESIAN_POINT('Ctrl Pts',(-0.00249997151790758,-0.0356930290785269,
-0.0120066699460638));
#28916=CARTESIAN_POINT('Ctrl Pts',(-0.00249999996448425,-0.0357037743898623,
-0.012175431885614));
#28917=CARTESIAN_POINT('',(-0.00249972264876189,-0.0367042860702267,-0.0121749056154874));
#28918=CARTESIAN_POINT('Ctrl Pts',(-0.0024999999999868,-0.0357038018947033,
-0.0121758614105833));
#28919=CARTESIAN_POINT('Ctrl Pts',(-0.00249999842185102,-0.0357347205736624,
-0.0126614999134783));
#28920=CARTESIAN_POINT('Ctrl Pts',(-0.00235420552434013,-0.0357656392526216,
-0.0131471138027068));
#28921=CARTESIAN_POINT('Ctrl Pts',(-0.00208693909926123,-0.0357965579315808,
-0.0135523289296316));
#28922=CARTESIAN_POINT('Ctrl Pts',(-0.00199404153534899,-0.0358073047732533,
-0.0136931752710327));
#28923=CARTESIAN_POINT('Ctrl Pts',(-0.00188691671847274,-0.0358180516149257,
-0.0138244541731427));
#28924=CARTESIAN_POINT('Ctrl Pts',(-0.00176788792603608,-0.0358287984565982,
-0.0139434992581757));
#28925=CARTESIAN_POINT('Ctrl Pts',(-0.00143175116039164,-0.035859147488347,
-0.0142796820340376));
#28926=CARTESIAN_POINT('Ctrl Pts',(-0.000995352781842014,-0.0358894965200957,
-0.0145182374567289));
#28927=CARTESIAN_POINT('Ctrl Pts',(-0.00052920129466083,-0.0359198455518445,
-0.0146192005786411));
#28928=CARTESIAN_POINT('Ctrl Pts',(-0.000355383620143761,-0.0359311620407274,
-0.0146568475143376));
#28929=CARTESIAN_POINT('Ctrl Pts',(-0.000177693789749482,-0.0359424785296102,
-0.0146758284126996));
#28930=CARTESIAN_POINT('Ctrl Pts',(-3.50299244509837E-7,-0.0359537950184931,
-0.0146758532620162));
#28931=CARTESIAN_POINT('Ctrl Pts',(0.000477015957030029,-0.035984256299687,
-0.0146759201504324));
#28932=CARTESIAN_POINT('Ctrl Pts',(0.000955932814372235,-0.0360147175808809,
-0.0145349420902015));
#28933=CARTESIAN_POINT('Ctrl Pts',(0.0013578313376968,-0.0360451788620748,
-0.0142749707340509));
#28934=CARTESIAN_POINT('Ctrl Pts',(0.00150565726978155,-0.0360563831015125,
-0.0141793483174259));
#28935=CARTESIAN_POINT('Ctrl Pts',(0.0016432051534008,-0.0360675873409502,
-0.0140681293640874));
#28936=CARTESIAN_POINT('Ctrl Pts',(0.00176739249258247,-0.0360787915803879,
-0.0139439946206044));
#28937=CARTESIAN_POINT('Ctrl Pts',(0.00210496066223601,-0.0361092471374863,
-0.0136065694174872));
#28938=CARTESIAN_POINT('Ctrl Pts',(0.00234392437601904,-0.0361397026945847,
-0.0131683409811333));
#28939=CARTESIAN_POINT('Ctrl Pts',(0.00244434181137516,-0.0361701582516831,
-0.0127004418006939));
#28940=CARTESIAN_POINT('Ctrl Pts',(0.00248130307216595,-0.0361813682152163,
-0.0125282192820577));
#28941=CARTESIAN_POINT('Ctrl Pts',(0.00249995009903626,-0.0361925781787496,
-0.0123522319776715));
#28942=CARTESIAN_POINT('Ctrl Pts',(0.00249999989954248,-0.0362037881422828,
-0.0121765620090651));
#28943=CARTESIAN_POINT('Ctrl Pts',(0.0025001351990157,-0.0362342436993812,
-0.0116992966956233));
#28944=CARTESIAN_POINT('Ctrl Pts',(0.00235928323479914,-0.0362646992564795,
-0.0112204434845985));
#28945=CARTESIAN_POINT('Ctrl Pts',(0.00209945993261631,-0.0362951548135779,
-0.0108185515546876));
#28946=CARTESIAN_POINT('Ctrl Pts',(0.00200382517758116,-0.0363063647771112,
-0.0106706247292461));
#28947=CARTESIAN_POINT('Ctrl Pts',(0.00189257505294478,-0.0363175747406445,
-0.0105329828990932));
#28948=CARTESIAN_POINT('Ctrl Pts',(0.00176839470571282,-0.0363287847041777,
-0.010408714309339));
#28949=CARTESIAN_POINT('Ctrl Pts',(0.0014309544933013,-0.0363592459853716,
-0.0100710343120011));
#28950=CARTESIAN_POINT('Ctrl Pts',(0.000992666047037264,-0.0363897072665655,
-0.00983198583372535));
#28951=CARTESIAN_POINT('Ctrl Pts',(0.000524681607744771,-0.0364201685477594,
-0.00973153145617357));
#28952=CARTESIAN_POINT('Ctrl Pts',(0.000352548016987815,-0.0364313727871972,
-0.0096945824226942));
#28953=CARTESIAN_POINT('Ctrl Pts',(0.00017665153322615,-0.0364425770266349,
-0.00967592846397843));
#28954=CARTESIAN_POINT('Ctrl Pts',(1.06714575491062E-6,-0.0364537812660726,
-0.00967585351431812));
#28955=CARTESIAN_POINT('Ctrl Pts',(-0.000474539983097998,-0.0364841302978213,
-0.0096756504974482));
#28956=CARTESIAN_POINT('Ctrl Pts',(-0.000951886033433265,-0.0365144793295702,
-0.00981549013244667));
#28957=CARTESIAN_POINT('Ctrl Pts',(-0.00135289294003649,-0.0365448283613189,
-0.0100735496232403));
#28958=CARTESIAN_POINT('Ctrl Pts',(-0.00150241962800714,-0.0365561448502018,
-0.0101697743523469));
#28959=CARTESIAN_POINT('Ctrl Pts',(-0.00164147633810056,-0.0365674613390846,
-0.0102819211394351));
#28960=CARTESIAN_POINT('Ctrl Pts',(-0.00176688542553261,-0.0365787778279675,
-0.0104072052455278));
#28961=CARTESIAN_POINT('Ctrl Pts',(-0.00210952556356602,-0.0366096965069265,
-0.0107495039121076));
#28962=CARTESIAN_POINT('Ctrl Pts',(-0.00235044197743157,-0.0366406151858856,
-0.011195205053263));
#28963=CARTESIAN_POINT('Ctrl Pts',(-0.00244854670136544,-0.0366715338648448,
-0.0116712553761062));
#28964=CARTESIAN_POINT('Ctrl Pts',(-0.0024826463450416,-0.0366822807065173,
-0.0118367229064141));
#28965=CARTESIAN_POINT('Ctrl Pts',(-0.00249990333900219,-0.0366930275481898,
-0.0120056275156314));
#28966=CARTESIAN_POINT('Ctrl Pts',(-0.00249999959355058,-0.0367037743898623,
-0.0121744277175772));
#28967=CARTESIAN_POINT('',(-0.00249992752834032,-0.037703848024675,-0.0121772085200007));
#28968=CARTESIAN_POINT('Ctrl Pts',(-0.00249923804932589,-0.0367051814111975,
-0.0121757418437438));
#28969=CARTESIAN_POINT('Ctrl Pts',(-0.00249855972559852,-0.0367376271573855,
-0.0126675611060721));
#28970=CARTESIAN_POINT('Ctrl Pts',(-0.00235152199160866,-0.0367651264597615,
-0.0131596652408496));
#28971=CARTESIAN_POINT('Ctrl Pts',(-0.00207812613851097,-0.0367966312627343,
-0.0135691277197265));
#28972=CARTESIAN_POINT('Ctrl Pts',(-0.0020685210477245,-0.0367977381064897,
-0.0135835131767066));
#28973=CARTESIAN_POINT('Ctrl Pts',(-0.00205875490051772,-0.0367988448921768,
-0.013597788859014));
#28974=CARTESIAN_POINT('Ctrl Pts',(-0.00204882967407331,-0.0367999522846867,
-0.0136119509893344));
#28975=CARTESIAN_POINT('Ctrl Pts',(-0.00196547955788986,-0.0368092519510344,
-0.0137308817980391));
#28976=CARTESIAN_POINT('Ctrl Pts',(-0.0018709240015511,-0.0368185944124242,
-0.0138417564093648));
#28977=CARTESIAN_POINT('Ctrl Pts',(-0.00176808080539617,-0.0368283734436502,
-0.0139439442940955));
#28978=CARTESIAN_POINT('Ctrl Pts',(-0.00153624688627666,-0.0368504177909582,
-0.0141743009797042));
#28979=CARTESIAN_POINT('Ctrl Pts',(-0.00125868197897531,-0.0368724829537764,
-0.0143590236955169));
#28980=CARTESIAN_POINT('Ctrl Pts',(-0.000956441897266579,-0.0368927141725844,
-0.0144845980144631));
#28981=CARTESIAN_POINT('Ctrl Pts',(-0.000654201815557846,-0.0369129453913923,
-0.0146101723334094));
#28982=CARTESIAN_POINT('Ctrl Pts',(-0.00032735114465414,-0.0369316777830255,
-0.0146769121014811));
#28983=CARTESIAN_POINT('Ctrl Pts',(7.98294045574838E-8,-0.0369526287167429,
-0.0146777668731382));
#28984=CARTESIAN_POINT('Ctrl Pts',(2.47087250033536E-5,-0.0369542046163984,
-0.0146778311678555));
#28985=CARTESIAN_POINT('Ctrl Pts',(4.93327602190462E-5,-0.0369557877516931,
-0.014677514822621));
#28986=CARTESIAN_POINT('Ctrl Pts',(7.39420047343854E-5,-0.0369573773469808,
-0.0146768118236171));
#28987=CARTESIAN_POINT('Ctrl Pts',(0.000376502481255991,-0.0369769207631717,
-0.0146681687418079));
#28988=CARTESIAN_POINT('Ctrl Pts',(0.00067701295653365,-0.0369974406515327,
-0.0146009312101924));
#28989=CARTESIAN_POINT('Ctrl Pts',(0.000956270931532571,-0.0370174955425343,
-0.0144847845969389));
#28990=CARTESIAN_POINT('Ctrl Pts',(0.00125824280448874,-0.0370391816304525,
-0.014359191011503));
#28991=CARTESIAN_POINT('Ctrl Pts',(0.00153575432463791,-0.0370591854105042,
-0.0141743965678716));
#28992=CARTESIAN_POINT('Ctrl Pts',(0.00176771012644472,-0.0370786390032289,
-0.0139435813207743));
#28993=CARTESIAN_POINT('Ctrl Pts',(0.00188368802734813,-0.0370883657995912,
-0.0138281736972256));
#28994=CARTESIAN_POINT('Ctrl Pts',(0.00198878162811406,-0.037098386354272,
-0.0137017201996478));
#28995=CARTESIAN_POINT('Ctrl Pts',(0.00208027048894701,-0.0371088726100384,
-0.013565738145873));
#28996=CARTESIAN_POINT('Ctrl Pts',(0.00209738775771892,-0.0371108345544405,
-0.0135402963451836));
#28997=CARTESIAN_POINT('Ctrl Pts',(0.00211400414750772,-0.0371127972484263,
-0.013514509538353));
#28998=CARTESIAN_POINT('Ctrl Pts',(0.00213009819447958,-0.0371147630535618,
-0.0134884013575589));
#28999=CARTESIAN_POINT('Ctrl Pts',(0.00220002406360927,-0.0371233041391496,
-0.0133749657974033));
#29000=CARTESIAN_POINT('Ctrl Pts',(0.00226003460348998,-0.0371319039555668,
-0.0132554650136785));
#29001=CARTESIAN_POINT('Ctrl Pts',(0.00231026196285467,-0.0371407561975987,
-0.0131327594162781));
#29002=CARTESIAN_POINT('Ctrl Pts',(0.00237204958583781,-0.037151645860128,
-0.012981812058384));
#29003=CARTESIAN_POINT('Ctrl Pts',(0.00241912822389077,-0.0371627376694534,
-0.0128259652542995));
#29004=CARTESIAN_POINT('Ctrl Pts',(0.00245118988178313,-0.0371737434262344,
-0.0126635182536309));
#29005=CARTESIAN_POINT('Ctrl Pts',(0.00246722071072931,-0.0371792463046249,
-0.0125822947532966));
#29006=CARTESIAN_POINT('Ctrl Pts',(0.00247924886171843,-0.037184729174554,
-0.0124993501380759));
#29007=CARTESIAN_POINT('Ctrl Pts',(0.00248695105986065,-0.0371898047233834,
-0.0124209100338158));
#29008=CARTESIAN_POINT('Ctrl Pts',(0.00249080215893176,-0.0371923424977981,
-0.0123816899816858));
#29009=CARTESIAN_POINT('Ctrl Pts',(0.00249374966613724,-0.0371947823017465,
-0.0123436223993365));
#29010=CARTESIAN_POINT('Ctrl Pts',(0.00249597895609703,-0.0371976356976271,
-0.012298583023874));
#29011=CARTESIAN_POINT('Ctrl Pts',(0.00249820824605681,-0.0372004890935078,
-0.0122535436484114));
#29012=CARTESIAN_POINT('Ctrl Pts',(0.00249904761869242,-0.0372037421797348,
-0.0122014924554208));
#29013=CARTESIAN_POINT('Ctrl Pts',(0.00249907294475291,-0.0372053301768058,
-0.0121759520549198));
#29014=CARTESIAN_POINT('Ctrl Pts',(0.00249908560778316,-0.0372061241753414,
-0.0121631818546693));
#29015=CARTESIAN_POINT('Ctrl Pts',(0.00249902385857616,-0.0372065047276103,
-0.0121570379698692));
#29016=CARTESIAN_POINT('Ctrl Pts',(0.00249899372733659,-0.0372067387506886,
-0.0121532622930291));
#29017=CARTESIAN_POINT('Ctrl Pts',(0.00249896359609703,-0.0372069727737668,
-0.0121494866161891));
#29018=CARTESIAN_POINT('Ctrl Pts',(0.00249894915827925,-0.0372070598936226,
-0.012148079571669));
#29019=CARTESIAN_POINT('Ctrl Pts',(0.00249891180836883,-0.0372072637224387,
-0.0121447869733562));
#29020=CARTESIAN_POINT('Ctrl Pts',(0.00249883710854799,-0.037207671380071,
-0.0121382017767306));
#29021=CARTESIAN_POINT('Ctrl Pts',(0.00249862743784474,-0.037208544928947,
-0.0121240749706626));
#29022=CARTESIAN_POINT('Ctrl Pts',(0.00249829606817123,-0.03720936813279,
-0.0121107206095793));
#29023=CARTESIAN_POINT('Ctrl Pts',(0.0024976333288242,-0.0372110145404761,
-0.0120840118874126));
#29024=CARTESIAN_POINT('Ctrl Pts',(0.00249668406465387,-0.0372124639781498,
-0.0120603837583854));
#29025=CARTESIAN_POINT('Ctrl Pts',(0.0024952206104089,-0.0372140812858203,
-0.0120339199927811));
#29026=CARTESIAN_POINT('Ctrl Pts',(0.00249229370191897,-0.0372173159011614,
-0.0119809924615723));
#29027=CARTESIAN_POINT('Ctrl Pts',(0.002487012242735,-0.0372212121210945,
-0.0119167482118306));
#29028=CARTESIAN_POINT('Ctrl Pts',(0.00247777616113699,-0.0372254769490124,
-0.0118461480055289));
#29029=CARTESIAN_POINT('Ctrl Pts',(0.00246854007953898,-0.0372297417769303,
-0.0117755477992272));
#29030=CARTESIAN_POINT('Ctrl Pts',(0.00245548734276733,-0.0372343746526518,
-0.0116985653847269));
#29031=CARTESIAN_POINT('Ctrl Pts',(0.002436394845427,-0.0372394863755516,
-0.0116147295254093));
#29032=CARTESIAN_POINT('Ctrl Pts',(0.00241730234808667,-0.0372445980984513,
-0.0115308936660916));
#29033=CARTESIAN_POINT('Ctrl Pts',(0.00239213549960774,-0.0372501832347442,
-0.01144023087194));
#29034=CARTESIAN_POINT('Ctrl Pts',(0.00235885979455609,-0.0372566368387057,
-0.0113439889242858));
#29035=CARTESIAN_POINT('Ctrl Pts',(0.00233366528118125,-0.037261523148735,
-0.0112711198736187));
#29036=CARTESIAN_POINT('Ctrl Pts',(0.0023035388911288,-0.0372667114623,
-0.011195276533937));
#29037=CARTESIAN_POINT('Ctrl Pts',(0.00226725689186798,-0.0372722367914396,
-0.0111174342408781));
#29038=CARTESIAN_POINT('Ctrl Pts',(0.00220769984171952,-0.037281306641816,
-0.0109896557985147));
#29039=CARTESIAN_POINT('Ctrl Pts',(0.00213143837634023,-0.0372912845926809,
-0.0108564220403585));
#29040=CARTESIAN_POINT('Ctrl Pts',(0.00203506830126738,-0.0373023255054793,
-0.010722635940189));
#29041=CARTESIAN_POINT('Ctrl Pts',(0.00187998982838368,-0.037320092513492,
-0.0105073476975298));
#29042=CARTESIAN_POINT('Ctrl Pts',(0.00167209784656463,-0.0373402307396795,
-0.0102902804756762));
#29043=CARTESIAN_POINT('Ctrl Pts',(0.00140122162816635,-0.0373606613334278,
-0.0101065759256013));
#29044=CARTESIAN_POINT('Ctrl Pts',(0.00113034540976807,-0.0373810919271762,
-0.00992287137552641));
#29045=CARTESIAN_POINT('Ctrl Pts',(0.000795801869857682,-0.0374013980344111,
-0.00977278122525912));
#29046=CARTESIAN_POINT('Ctrl Pts',(0.000411562655167207,-0.0374263325491636,
-0.00970796947441034));
#29047=CARTESIAN_POINT('Ctrl Pts',(0.000394994239586353,-0.0374274077267794,
-0.0097051747882317));
#29048=CARTESIAN_POINT('Ctrl Pts',(0.00037834529328193,-0.0374284912538621,
-0.00970254432404357));
#29049=CARTESIAN_POINT('Ctrl Pts',(0.000361617587882895,-0.0374295827143858,
-0.00970008436041701));
#29050=CARTESIAN_POINT('Ctrl Pts',(-9.58802205126288E-6,-0.0374538033866029,
-0.00964549514589953));
#29051=CARTESIAN_POINT('Ctrl Pts',(-0.000423761120905089,-0.0374819308294292,
-0.00967548372821087));
#29052=CARTESIAN_POINT('Ctrl Pts',(-0.000830943860492442,-0.0375094187748174,
-0.00981905156170969));
#29053=CARTESIAN_POINT('Ctrl Pts',(-0.00120508340729675,-0.0375346760522761,
-0.00995096875499584));
#29054=CARTESIAN_POINT('Ctrl Pts',(-0.00157461097999646,-0.0375587613643777,
-0.0101807716301553));
#29055=CARTESIAN_POINT('Ctrl Pts',(-0.00186972884662011,-0.0375869868999544,
-0.0105132308823403));
#29056=CARTESIAN_POINT('Ctrl Pts',(-0.00188237997769656,-0.0375881968739704,
-0.0105274827662574));
#29057=CARTESIAN_POINT('Ctrl Pts',(-0.00189489004442169,-0.037589414456354,
-0.0105419235332971));
#29058=CARTESIAN_POINT('Ctrl Pts',(-0.00190725605658699,-0.0375906400655857,
-0.0105565503326961));
#29059=CARTESIAN_POINT('Ctrl Pts',(-0.00193451409969029,-0.0375933416405815,
-0.0105887917637372));
#29060=CARTESIAN_POINT('Ctrl Pts',(-0.00196101730123458,-0.037596055918673,
-0.0106219374042091));
#29061=CARTESIAN_POINT('Ctrl Pts',(-0.00198680450692279,-0.0375988418278651,
-0.010655880158455));
#29062=CARTESIAN_POINT('Ctrl Pts',(-0.00224671291071142,-0.0376269209156098,
-0.0109979880697548));
#29063=CARTESIAN_POINT('Ctrl Pts',(-0.00243044774190981,-0.0376584425706656,
-0.0114279639088363));
#29064=CARTESIAN_POINT('Ctrl Pts',(-0.00248377020356829,-0.0376872536324111,
-0.0118982228572852));
#29065=CARTESIAN_POINT('Ctrl Pts',(-0.00249412635367718,-0.0376928492420463,
-0.0119895553297315));
#29066=CARTESIAN_POINT('Ctrl Pts',(-0.00249958564975923,-0.0376984023199869,
-0.0120822814837863));
#29067=CARTESIAN_POINT('Ctrl Pts',(-0.00249980699897089,-0.037703972088345,
-0.0121758498398408));
#29068=CARTESIAN_POINT('',(-0.00249999985275848,-0.0387038137045467,-0.0121752545238663));
#29069=CARTESIAN_POINT('Ctrl Pts',(-0.00249999906545952,-0.0377037743898623,
-0.0121780149297994));
#29070=CARTESIAN_POINT('Ctrl Pts',(-0.00249957915265185,-0.0377346978836163,
-0.012663655486345));
#29071=CARTESIAN_POINT('Ctrl Pts',(-0.00235336672748243,-0.0377656213773703,
-0.0131491454651922));
#29072=CARTESIAN_POINT('Ctrl Pts',(-0.00208574922620988,-0.0377965448711243,
-0.0135541312575657));
#29073=CARTESIAN_POINT('Ctrl Pts',(-0.00199277586707078,-0.037807288044037,
-0.0136948279210557));
#29074=CARTESIAN_POINT('Ctrl Pts',(-0.00188559757212201,-0.0378180312169497,
-0.0138259543605948));
#29075=CARTESIAN_POINT('Ctrl Pts',(-0.00176653632040396,-0.0378287743898624,
-0.0139448500159767));
#29076=CARTESIAN_POINT('Ctrl Pts',(-0.00143013920781834,-0.0378591282816254,
-0.0142807792506547));
#29077=CARTESIAN_POINT('Ctrl Pts',(-0.00099355393580092,-0.0378894821733885,
-0.0145190018168816));
#29078=CARTESIAN_POINT('Ctrl Pts',(-0.000527321111942944,-0.0379198360651516,
-0.0146196070476599));
#29079=CARTESIAN_POINT('Ctrl Pts',(-0.000353557990227819,-0.0379311488400552,
-0.0146571022175972));
#29080=CARTESIAN_POINT('Ctrl Pts',(-0.000175940789421143,-0.0379424616149587,
-0.0146759463829256));
#29081=CARTESIAN_POINT('Ctrl Pts',(1.31790050661161E-6,-0.0379537743898623,
-0.0146758529391857));
#29082=CARTESIAN_POINT('Ctrl Pts',(0.000478688717282434,-0.0379842405328645,
-0.0146756012882542));
#29083=CARTESIAN_POINT('Ctrl Pts',(0.000957515025671042,-0.0380147066758667,
-0.0145343010843038));
#29084=CARTESIAN_POINT('Ctrl Pts',(0.00135924181305373,-0.0380451728188689,
-0.0142740576840481));
#29085=CARTESIAN_POINT('Ctrl Pts',(0.00150693200109036,-0.0380563733425334,
-0.0141783822202099));
#29086=CARTESIAN_POINT('Ctrl Pts',(0.00164434366011201,-0.0380675738661978,
-0.0140671322639597));
#29087=CARTESIAN_POINT('Ctrl Pts',(0.00176840042766013,-0.0380787743898623,
-0.0139429865377453));
#29088=CARTESIAN_POINT('Ctrl Pts',(0.00210577931443683,-0.0381092348014942,
-0.0136053657232093));
#29089=CARTESIAN_POINT('Ctrl Pts',(0.00234449381233911,-0.0381396952131261,
-0.0131669968114185));
#29090=CARTESIAN_POINT('Ctrl Pts',(0.0024446429880769,-0.0381701556247581,
-0.0126990364866386));
#29091=CARTESIAN_POINT('Ctrl Pts',(0.00248148744108023,-0.0381813618797928,
-0.0125268758865462));
#29092=CARTESIAN_POINT('Ctrl Pts',(0.00250003325712235,-0.0381925681348276,
-0.012350964658492));
#29093=CARTESIAN_POINT('Ctrl Pts',(0.00249999995503491,-0.0382037743898623,
-0.0121753791289363));
#29094=CARTESIAN_POINT('Ctrl Pts',(0.00249990943458105,-0.0382342348014941,
-0.0116981092925555));
#29095=CARTESIAN_POINT('Ctrl Pts',(0.00235882837656811,-0.038264695213126,
-0.0112193192424479));
#29096=CARTESIAN_POINT('Ctrl Pts',(0.00209881112704663,-0.0382951556247579,
-0.0108175485147984));
#29097=CARTESIAN_POINT('Ctrl Pts',(0.00200315189411168,-0.0383063618797927,
-0.0106697387841232));
#29098=CARTESIAN_POINT('Ctrl Pts',(0.0018918973356533,-0.0383175681348275,
-0.0105322115233738));
#29099=CARTESIAN_POINT('Ctrl Pts',(0.00176772998068626,-0.0383287743898623,
-0.0104080493620849));
#29100=CARTESIAN_POINT('Ctrl Pts',(0.00143015954516786,-0.0383592405328645,
-0.0100704930464788));
#29101=CARTESIAN_POINT('Ctrl Pts',(0.000991776834235544,-0.0383897066758667,
-0.00983160868598701));
#29102=CARTESIAN_POINT('Ctrl Pts',(0.000523750573447141,-0.0384201728188689,
-0.00973133179211101));
#29103=CARTESIAN_POINT('Ctrl Pts',(0.000351686153964219,-0.0384313733425333,
-0.00969446615661599));
#29104=CARTESIAN_POINT('Ctrl Pts',(0.000175869444756074,-0.0384425738661978,
-0.00967587925874551));
#29105=CARTESIAN_POINT('Ctrl Pts',(3.69585316966004E-7,-0.0384537743898623,
-0.00967585331387676));
#29106=CARTESIAN_POINT('Ctrl Pts',(-0.000475242439390424,-0.0384841282816254,
-0.00967578300218763));
#29107=CARTESIAN_POINT('Ctrl Pts',(-0.000952553277734538,-0.0385144821733884,
-0.00981575854653882));
#29108=CARTESIAN_POINT('Ctrl Pts',(-0.00135349011024409,-0.0385448360651514,
-0.0100739340394243));
#29109=CARTESIAN_POINT('Ctrl Pts',(-0.0015029176753208,-0.038556148840055,
-0.0101701550202279));
#29110=CARTESIAN_POINT('Ctrl Pts',(-0.00164188085258634,-0.0385674616149587,
-0.010282279737598));
#29111=CARTESIAN_POINT('Ctrl Pts',(-0.00176720721992576,-0.0385787743898623,
-0.0104075267777249));
#29112=CARTESIAN_POINT('Ctrl Pts',(-0.00210978710599715,-0.0386096978836163,
-0.0107498898226957));
#29113=CARTESIAN_POINT('Ctrl Pts',(-0.00235062273498652,-0.0386406213773703,
-0.0111956374309725));
#29114=CARTESIAN_POINT('Ctrl Pts',(-0.00244863989484262,-0.0386715448711244,
-0.0116717078061805));
#29115=CARTESIAN_POINT('Ctrl Pts',(-0.00248269216930797,-0.038682288044037,
-0.0118371000610185));
#29116=CARTESIAN_POINT('Ctrl Pts',(-0.00249991782187621,-0.0386930312169497,
-0.0120059228706272));
#29117=CARTESIAN_POINT('Ctrl Pts',(-0.00249999970556691,-0.0387037743898623,
-0.0121746399583445));
#29118=CARTESIAN_POINT('',(-0.00249999994305708,-0.0397037978472385,-0.0121754691093855));
#29119=CARTESIAN_POINT('Ctrl Pts',(-0.00249999999995005,-0.0387038530192311,
-0.0121758690893881));
#29120=CARTESIAN_POINT('Ctrl Pts',(-0.0024999969301698,-0.0387347687629928,
-0.012661506828381));
#29121=CARTESIAN_POINT('Ctrl Pts',(-0.00235420297464426,-0.0387656845067545,
-0.0131471196348283));
#29122=CARTESIAN_POINT('Ctrl Pts',(-0.00208693602911737,-0.0387966002505162,
-0.013552333584409));
#29123=CARTESIAN_POINT('Ctrl Pts',(-0.00199402250511303,-0.0388073478971975,
-0.0136932034400399));
#29124=CARTESIAN_POINT('Ctrl Pts',(-0.00188687694470658,-0.0388180955438787,
-0.0138245025803785));
#29125=CARTESIAN_POINT('Ctrl Pts',(-0.00176782386158655,-0.03882884319056,
-0.0139435633290722));
#29126=CARTESIAN_POINT('Ctrl Pts',(-0.00143167610268005,-0.0388591892954298,
-0.0142797327318146));
#29127=CARTESIAN_POINT('Ctrl Pts',(-0.000995270678790388,-0.0388895354002997,
-0.0145182720734748));
#29128=CARTESIAN_POINT('Ctrl Pts',(-0.000529117003512208,-0.0389198815051695,
-0.0146192188336251));
#29129=CARTESIAN_POINT('Ctrl Pts',(-0.000355269510177465,-0.0389311987907426,
-0.014656865949036));
#29130=CARTESIAN_POINT('Ctrl Pts',(-0.000177549231046672,-0.0389425160763158,
-0.0146758407388477));
#29131=CARTESIAN_POINT('Ctrl Pts',(-1.76767305915852E-7,-0.0389538333618889,
-0.0146758532803088));
#29132=CARTESIAN_POINT('Ctrl Pts',(0.000477187912742321,-0.038984291710906,
-0.0146758870332962));
#29133=CARTESIAN_POINT('Ctrl Pts',(0.000956093742291461,-0.0390147500599231,
-0.0145348766195195));
#29134=CARTESIAN_POINT('Ctrl Pts',(0.00135797359406222,-0.0390452084089402,
-0.0142748787075165));
#29135=CARTESIAN_POINT('Ctrl Pts',(0.00150581747045849,-0.039056413450366,
-0.0141792304708705));
#29136=CARTESIAN_POINT('Ctrl Pts',(0.00164337882623664,-0.039067618491792,
-0.0140679812187286));
#29137=CARTESIAN_POINT('Ctrl Pts',(0.00176757386523736,-0.0390788235332179,
-0.0139438133061654));
#29138=CARTESIAN_POINT('Ctrl Pts',(0.00210510633250146,-0.0391092761608647,
-0.0136063545620827));
#29139=CARTESIAN_POINT('Ctrl Pts',(0.00234402484748426,-0.0391397287885115,
-0.0131681030789221));
#29140=CARTESIAN_POINT('Ctrl Pts',(0.00244439477502579,-0.0391701814161583,
-0.0127001949536289));
#29141=CARTESIAN_POINT('Ctrl Pts',(0.00248134473752436,-0.0391813921789545,
-0.012527940294232));
#29142=CARTESIAN_POINT('Ctrl Pts',(0.00249997401585501,-0.0391926029417506,
-0.012351921455295));
#29143=CARTESIAN_POINT('Ctrl Pts',(0.00249999997271797,-0.0392038137045467,
-0.0121762226239989));
#29144=CARTESIAN_POINT('Ctrl Pts',(0.00250007048127274,-0.0392342663321936,
-0.0116989588387642));
#29145=CARTESIAN_POINT('Ctrl Pts',(0.00235915437950149,-0.0392647189598404,
-0.0112201259624989));
#29146=CARTESIAN_POINT('Ctrl Pts',(0.00209927782671647,-0.0392951715874873,
-0.010818269916648));
#29147=CARTESIAN_POINT('Ctrl Pts',(0.00200360744899664,-0.0393063823502834,
-0.0106703315232702));
#29148=CARTESIAN_POINT('Ctrl Pts',(0.00189231790892485,-0.0393175931130795,
-0.0105326836318434));
#29149=CARTESIAN_POINT('Ctrl Pts',(0.00176809616713814,-0.0393288038758756,
-0.010408415609085));
#29150=CARTESIAN_POINT('Ctrl Pts',(0.00143060002743081,-0.0393592622248927,
-0.0100707937293175));
#29151=CARTESIAN_POINT('Ctrl Pts',(0.000992272707346792,-0.0393897205739098,
-0.00983181954340048));
#29152=CARTESIAN_POINT('Ctrl Pts',(0.000524272698241825,-0.039420178922927,
-0.00973144371820049));
#29153=CARTESIAN_POINT('Ctrl Pts',(0.000352104486288874,-0.0394313839643528,
-0.0096945173805685));
#29154=CARTESIAN_POINT('Ctrl Pts',(0.000176175198052129,-0.0394425890057786,
-0.00967589282108229));
#29155=CARTESIAN_POINT('Ctrl Pts',(5.61907573495769E-7,-0.0394537940472045,
-0.00967585334970612));
#29156=CARTESIAN_POINT('Ctrl Pts',(-0.000475043592385584,-0.0394841401520743,
-0.00967574645117045));
#29157=CARTESIAN_POINT('Ctrl Pts',(-0.000952360064664738,-0.0395144862569442,
-0.00981568162193327));
#29158=CARTESIAN_POINT('Ctrl Pts',(-0.00135331414519892,-0.039544832361814,
-0.0100738207405673));
#29159=CARTESIAN_POINT('Ctrl Pts',(-0.00150284608185382,-0.0395561496473871,
-0.010170091221926));
#29160=CARTESIAN_POINT('Ctrl Pts',(-0.00164190139392532,-0.0395674669329603,
-0.0102822869096362));
#29161=CARTESIAN_POINT('Ctrl Pts',(-0.00176730147922207,-0.0395787842185334,
-0.0104076209823799));
#29162=CARTESIAN_POINT('Ctrl Pts',(-0.00210986037991485,-0.0396096999622953,
-0.0107499995547453));
#29163=CARTESIAN_POINT('Ctrl Pts',(-0.00235067181986224,-0.0396406157060572,
-0.0111957564616439));
#29164=CARTESIAN_POINT('Ctrl Pts',(-0.00244866486404371,-0.0396715314498192,
-0.0116718290970614));
#29165=CARTESIAN_POINT('Ctrl Pts',(-0.00248273147502909,-0.0396822790965002,
-0.0118373324897463));
#29166=CARTESIAN_POINT('Ctrl Pts',(-0.00249994893517625,-0.0396930267431813,
-0.0120062701810751));
#29167=CARTESIAN_POINT('Ctrl Pts',(-0.00249999988615268,-0.0397037743898623,
-0.0121750988088553));
#29168=CARTESIAN_POINT('Ctrl Pts',(-0.00249999999996149,-0.0397038213046146,
-0.0121758394099156));
#29169=CARTESIAN_POINT('Ctrl Pts',(-0.00250000270759189,-0.0397348741491189,
-0.0126636429977115));
#29170=CARTESIAN_POINT('Ctrl Pts',(-0.00235297981442275,-0.0397659269936232,
-0.0131510877618962));
#29171=CARTESIAN_POINT('Ctrl Pts',(-0.00208362329733661,-0.0397969798381275,
-0.0135573430457659));
#29172=CARTESIAN_POINT('Ctrl Pts',(-0.00203675232193105,-0.0398023833721752,
-0.0136280359015566));
#29173=CARTESIAN_POINT('Ctrl Pts',(-0.00198629761776183,-0.0398077869062229,
-0.0136963151048329));
#29174=CARTESIAN_POINT('Ctrl Pts',(-0.00193253383622679,-0.0398131904402706,
-0.0137618271110075));
#29175=CARTESIAN_POINT('Ctrl Pts',(-0.00162797270880739,-0.0398438003857508,
-0.0141329395939904));
#29176=CARTESIAN_POINT('Ctrl Pts',(-0.00121263146935118,-0.0398744103312313,
-0.0144143026950736));
#29177=CARTESIAN_POINT('Ctrl Pts',(-0.000754274313859049,-0.0399050202767117,
-0.0145593528689899));
#29178=CARTESIAN_POINT('Ctrl Pts',(-0.000666729093165872,-0.0399108667097833,
-0.0145870571370152));
#29179=CARTESIAN_POINT('Ctrl Pts',(-0.000577695385311776,-0.0399167131428548,
-0.0146099200360221));
#29180=CARTESIAN_POINT('Ctrl Pts',(-0.000487736012541149,-0.0399225595759265,
-0.0146278144571459));
#29181=CARTESIAN_POINT('Ctrl Pts',(-1.52759145852082E-5,-0.0399532646181766,
-0.014721794658393));
#29182=CARTESIAN_POINT('Ctrl Pts',(0.000485825779097723,-0.0399839696604266,
-0.0146751536575047));
#29183=CARTESIAN_POINT('Ctrl Pts',(0.000933184668445214,-0.0400146747026767,
-0.0144951562798254));
#29184=CARTESIAN_POINT('Ctrl Pts',(0.00101697909541043,-0.0400204260389786,
-0.0144614411185153));
#29185=CARTESIAN_POINT('Ctrl Pts',(0.00109890870822176,-0.0400261773752806,
-0.0144231941637545));
#29186=CARTESIAN_POINT('Ctrl Pts',(0.00117848419324155,-0.0400319287115825,
-0.0143806605357932));
#29187=CARTESIAN_POINT('Ctrl Pts',(0.00160317707498042,-0.0400626234863275,
-0.014153659355402));
#29188=CARTESIAN_POINT('Ctrl Pts',(0.0019608573886363,-0.0400933182610726,
-0.0137998630381147));
#29189=CARTESIAN_POINT('Ctrl Pts',(0.00219248251600564,-0.0401240130358175,
-0.0133771111344033));
#29190=CARTESIAN_POINT('Ctrl Pts',(0.00223596002078373,-0.0401297746396245,
-0.0132977579220713));
#29191=CARTESIAN_POINT('Ctrl Pts',(0.00227510586067259,-0.0401355362434315,
-0.0132160760307234));
#29192=CARTESIAN_POINT('Ctrl Pts',(0.0023096961760887,-0.0401412978472384,
-0.0131325682776402));
#29193=CARTESIAN_POINT('Ctrl Pts',(0.00249397506363996,-0.0401719926219835,
-0.0126876831803244));
#29194=CARTESIAN_POINT('Ctrl Pts',(0.00254602571120722,-0.0402026873967285,
-0.0121872878122934));
#29195=CARTESIAN_POINT('Ctrl Pts',(0.00245688259764042,-0.0402333821714736,
-0.0117135461360492));
#29196=CARTESIAN_POINT('Ctrl Pts',(0.00244014987010768,-0.0402391437752805,
-0.0116246218201674));
#29197=CARTESIAN_POINT('Ctrl Pts',(0.00241859117801914,-0.0402449053790875,
-0.0115366450454989));
#29198=CARTESIAN_POINT('Ctrl Pts',(0.00239235234989162,-0.0402506669828944,
-0.0114501465730932));
#29199=CARTESIAN_POINT('Ctrl Pts',(0.002252519006042,-0.040281372025145,
-0.0109891743613927));
#29200=CARTESIAN_POINT('Ctrl Pts',(0.00197516790000548,-0.0403120770673955,
-0.0105692288056267));
#29201=CARTESIAN_POINT('Ctrl Pts',(0.00160553921447455,-0.040342782109646,
-0.0102595433349103));
#29202=CARTESIAN_POINT('Ctrl Pts',(0.00153630436829489,-0.0403485334459475,
-0.0102015364031747));
#29203=CARTESIAN_POINT('Ctrl Pts',(0.0014639518422826,-0.040354284782249,
-0.010147310350429));
#29204=CARTESIAN_POINT('Ctrl Pts',(0.00138892846704934,-0.0403600361185504,
-0.0100971811831661));
#29205=CARTESIAN_POINT('Ctrl Pts',(0.000989636666800498,-0.0403906460640308,
-0.00983038213048244));
#29206=CARTESIAN_POINT('Ctrl Pts',(0.000510458335853878,-0.0404212560095112,
-0.00968176584124858));
#29207=CARTESIAN_POINT('Ctrl Pts',(2.98264480542069E-5,-0.0404518659549916,
-0.0096760312162906));
#29208=CARTESIAN_POINT('Ctrl Pts',(-6.1973198106119E-5,-0.0404577123880632,
-0.00967493591538493));
#29209=CARTESIAN_POINT('Ctrl Pts',(-0.000153787395074284,-0.0404635588211348,
-0.00967890365590639));
#29210=CARTESIAN_POINT('Ctrl Pts',(-0.000245041124596022,-0.0404694052542064,
-0.0096878912998596));
#29211=CARTESIAN_POINT('Ctrl Pts',(-0.000729727742681694,-0.0405004580987112,
-0.00973562842550997));
#29212=CARTESIAN_POINT('Ctrl Pts',(-0.0012004523423602,-0.0405315109432161,
-0.00992929143953727));
#29213=CARTESIAN_POINT('Ctrl Pts',(-0.0015788116380206,-0.040562563787721,
-0.0102374637974072));
#29214=CARTESIAN_POINT('Ctrl Pts',(-0.00164465028722456,-0.0405679673217681,
-0.0102910891529802));
#29215=CARTESIAN_POINT('Ctrl Pts',(-0.00170774550115013,-0.0405733708558151,
-0.0103480648817755));
#29216=CARTESIAN_POINT('Ctrl Pts',(-0.00176776695296642,-0.0405787743898623,
-0.0104080863335918));
#29217=CARTESIAN_POINT('Ctrl Pts',(-0.00249999922097496,-0.0405787743898623,
-0.012173879679554));
#29218=CARTESIAN_POINT('Ctrl Pts',(-0.00249961583479718,-0.0405478495637463,
-0.0116882383417466));
#29219=CARTESIAN_POINT('Ctrl Pts',(-0.00235343949917405,-0.0405169247376302,
-0.0112027367429832));
#29220=CARTESIAN_POINT('Ctrl Pts',(-0.00208585174715449,-0.0404859999115143,
-0.0107977304731294));
#29221=CARTESIAN_POINT('Ctrl Pts',(-0.00199290425717607,-0.0404752580709636,
-0.0106570502068455));
#29222=CARTESIAN_POINT('Ctrl Pts',(-0.00188575583833928,-0.0404645162304129,
-0.0105259359162076));
#29223=CARTESIAN_POINT('Ctrl Pts',(-0.00176672706272141,-0.0404537743898623,
-0.0104070470547035));
#29224=CARTESIAN_POINT('Ctrl Pts',(-0.00143036500450258,-0.0404234191452761,
-0.0100710803781813));
#29225=CARTESIAN_POINT('Ctrl Pts',(-0.000993803849420159,-0.0403930639006899,
-0.0098328104764883));
#29226=CARTESIAN_POINT('Ctrl Pts',(-0.000527580430923165,-0.0403627086561037,
-0.00973215549654663));
#29227=CARTESIAN_POINT('Ctrl Pts',(-0.000353849336270321,-0.0403513972340232,
-0.00969464794297092));
#29228=CARTESIAN_POINT('Ctrl Pts',(-0.000176263431322318,-0.0403400858119428,
-0.00967578493628572));
#29229=CARTESIAN_POINT('Ctrl Pts',(9.66782122917552E-7,-0.0403287743898623,
-0.00967585347349164));
#29230=CARTESIAN_POINT('Ctrl Pts',(0.000478339182571104,-0.0402983068944727,
-0.00967603807954653));
#29231=CARTESIAN_POINT('Ctrl Pts',(0.000957186551135902,-0.0402678393990832,
-0.00981727190682606));
#29232=CARTESIAN_POINT('Ctrl Pts',(0.00135895049920568,-0.0402373719036936,
-0.0100774602011929));
#29233=CARTESIAN_POINT('Ctrl Pts',(0.00150662995922923,-0.0402261727324165,
-0.010173099610854));
#29234=CARTESIAN_POINT('Ctrl Pts',(0.00164403641083569,-0.0402149735611394,
-0.0102843098558379));
#29235=CARTESIAN_POINT('Ctrl Pts',(0.00176809457439739,-0.0402037743898623,
-0.0104084140157523));
#29236=CARTESIAN_POINT('Ctrl Pts',(0.00210553295380404,-0.0401733126282341,
-0.0107459775053031));
#29237=CARTESIAN_POINT('Ctrl Pts',(0.00234432355200967,-0.0401428508666059,
-0.0111843065377002));
#29238=CARTESIAN_POINT('Ctrl Pts',(0.00244455322970797,-0.0401123891049778,
-0.0116522508542449));
#29239=CARTESIAN_POINT('Ctrl Pts',(0.00248142122291065,-0.0401011841999393,
-0.0118243771972382));
#29240=CARTESIAN_POINT('Ctrl Pts',(0.00249999718775118,-0.0400899792949008,
-0.0120002560863263));
#29241=CARTESIAN_POINT('Ctrl Pts',(0.00249999999967931,-0.0400787743898623,
-0.012175813243643));
#29242=CARTESIAN_POINT('Ctrl Pts',(0.00250000764421395,-0.0400483126282342,
-0.0126530846047037));
#29243=CARTESIAN_POINT('Ctrl Pts',(0.0023590242138907,-0.0400178508666063,
-0.0131319048509345));
#29244=CARTESIAN_POINT('Ctrl Pts',(0.0020990883225621,-0.0399873891049782,
-0.0135337296484127));
#29245=CARTESIAN_POINT('Ctrl Pts',(0.00200347477880099,-0.0399761841999396,
-0.013681534911709));
#29246=CARTESIAN_POINT('Ctrl Pts',(0.00189226889350245,-0.0399649792949009,
-0.0138190642417662));
#29247=CARTESIAN_POINT('Ctrl Pts',(0.00176815119222662,-0.0399537743898623,
-0.0139432359167284));
#29248=CARTESIAN_POINT('Ctrl Pts',(0.00143066011324305,-0.0399233068944727,
-0.0142808737567094));
#29249=CARTESIAN_POINT('Ctrl Pts',(0.000992332864294848,-0.0398928393990831,
-0.0145198628226008));
#29250=CARTESIAN_POINT('Ctrl Pts',(0.000524329143107271,-0.0398623719036935,
-0.0146202507480378));
#29251=CARTESIAN_POINT('Ctrl Pts',(0.000352301420944516,-0.0398511727324164,
-0.0146571511087908));
#29252=CARTESIAN_POINT('Ctrl Pts',(0.000176518305235053,-0.0398399735611394,
-0.0146757795891959));
#29253=CARTESIAN_POINT('Ctrl Pts',(1.04686794656891E-6,-0.0398287743898623,
-0.0146758530673716));
#29254=CARTESIAN_POINT('Ctrl Pts',(-0.000474566752473521,-0.0397984191452761,
-0.0146760522292507));
#29255=CARTESIAN_POINT('Ctrl Pts',(-0.000951916780078385,-0.0397680639006899,
-0.0145362050849411));
#29256=CARTESIAN_POINT('Ctrl Pts',(-0.00135292419538027,-0.0397377086561037,
-0.0142781368358337));
#29257=CARTESIAN_POINT('Ctrl Pts',(-0.00150235353432011,-0.0397263972340233,
-0.014181971611965));
#29258=CARTESIAN_POINT('Ctrl Pts',(-0.00164132616302582,-0.0397150858119428,
-0.0140699049910283));
#29259=CARTESIAN_POINT('Ctrl Pts',(-0.00176667039928876,-0.0397037743898623,
-0.0139447161134265));
#29260=CARTESIAN_POINT('Ctrl Pts',(-0.00210935487198405,-0.0396728495637463,
-0.0136024563830445));
#29261=CARTESIAN_POINT('Ctrl Pts',(-0.00235032589488465,-0.0396419247376303,
-0.01315678100991));
#29262=CARTESIAN_POINT('Ctrl Pts',(-0.00244848723592954,-0.0396109999115143,
-0.0126807396653505));
#29263=CARTESIAN_POINT('Ctrl Pts',(-0.00248258390214153,-0.0396002580709636,
-0.0125153851311136));
#29264=CARTESIAN_POINT('Ctrl Pts',(-0.00249986058216984,-0.039589516230413,
-0.0123465960986312));
#29265=CARTESIAN_POINT('Ctrl Pts',(-0.00249999915646903,-0.0395787743898623,
-0.0121779069793664));
#29266=CARTESIAN_POINT('Origin',(0.,-0.0405787743898723,-0.0121758532865581));
#29267=CARTESIAN_POINT('',(0.00257042566803073,-0.0405782384986467,-0.0106271515585321));
#29268=CARTESIAN_POINT('',(0.0007218555435634,-0.0405787743898678,-0.0150877125850593));
#29269=CARTESIAN_POINT('Origin',(1.00006808390063E-14,-0.0405787743898623,
-0.0121758532865681));
#29270=CARTESIAN_POINT('Ctrl Pts',(0.000721855543558197,-0.0405787743898723,
-0.0150877125850536));
#29271=CARTESIAN_POINT('Ctrl Pts',(0.00012268413029149,-0.0405787743898723,
-0.0151791096272557));
#29272=CARTESIAN_POINT('Ctrl Pts',(-0.000503677158141744,-0.0405787743898723,
-0.0150739619320304));
#29273=CARTESIAN_POINT('Ctrl Pts',(-0.00104449598105803,-0.0405787743898723,
-0.0148006456629191));
#29274=CARTESIAN_POINT('Ctrl Pts',(-0.00134936358119689,-0.0405787743898723,
-0.0146465732240318));
#29275=CARTESIAN_POINT('Ctrl Pts',(-0.001626067145542,-0.0405787743898723,
-0.0144398053336723));
#29276=CARTESIAN_POINT('Ctrl Pts',(-0.0018533658809598,-0.0405787743898723,
-0.014182243962393));
#29277=CARTESIAN_POINT('Ctrl Pts',(-0.0019941234239128,-0.0405787743898723,
-0.0140227459092506));
#29278=CARTESIAN_POINT('Ctrl Pts',(-0.00211781727968312,-0.0405787743898723,
-0.0138421912823585));
#29279=CARTESIAN_POINT('Ctrl Pts',(-0.00222177552425318,-0.0405787743898723,
-0.0136368054667619));
#29280=CARTESIAN_POINT('Ctrl Pts',(-0.00231573504664697,-0.0405787743898723,
-0.013451173694893));
#29281=CARTESIAN_POINT('Ctrl Pts',(-0.00238865409568575,-0.0405787743898723,
-0.013253473685689));
#29282=CARTESIAN_POINT('Ctrl Pts',(-0.00243804199053378,-0.0405787743898723,
-0.0130507592809956));
#29283=CARTESIAN_POINT('Ctrl Pts',(-0.00250778716150712,-0.0405787743898723,
-0.0127644876985035));
#29284=CARTESIAN_POINT('Ctrl Pts',(-0.00253129823554409,-0.0405787743898723,
-0.0124667360306207));
#29285=CARTESIAN_POINT('Ctrl Pts',(-0.00250173218769294,-0.0405787743898723,
-0.0121740091469983));
#29286=CARTESIAN_POINT('Ctrl Pts',(-0.00176776695296641,-0.0405787743898723,
-0.0104080863335918));
#29287=CARTESIAN_POINT('Ctrl Pts',(-0.00149473584801468,-0.0405787743898723,
-0.0100673811147438));
#29288=CARTESIAN_POINT('Ctrl Pts',(-0.00112754673188857,-0.0405787743898723,
-0.00980644043751801));
#29289=CARTESIAN_POINT('Ctrl Pts',(-0.000722280104342335,-0.0405787743898723,
-0.00964250969240816));
#29290=CARTESIAN_POINT('Ctrl Pts',(-0.000462635152748786,-0.0405787743898723,
-0.00953748305689057));
#29291=CARTESIAN_POINT('Ctrl Pts',(-0.000187046045747263,-0.0405787743898723,
-0.00947201344856637));
#29292=CARTESIAN_POINT('Ctrl Pts',(9.20188708201852E-5,-0.0405787743898723,
-0.00945044526887669));
#29293=CARTESIAN_POINT('Ctrl Pts',(0.000248532219532483,-0.0405787743898723,
-0.00943834877150833));
#29294=CARTESIAN_POINT('Ctrl Pts',(0.00040854209693118,-0.0405787743898723,
-0.00944044634427772));
#29295=CARTESIAN_POINT('Ctrl Pts',(0.000560837419894266,-0.0405787743898723,
-0.00945634420536109));
#29296=CARTESIAN_POINT('Ctrl Pts',(0.000864786366481517,-0.0405787743898723,
-0.00948807294157746));
#29297=CARTESIAN_POINT('Ctrl Pts',(0.00113113360580538,-0.0405787743898723,
-0.00957065365736988));
#29298=CARTESIAN_POINT('Ctrl Pts',(0.00135440211750958,-0.0405787743898723,
-0.00966712856289749));
#29299=CARTESIAN_POINT('Ctrl Pts',(0.00147242656286442,-0.0405787743898723,
-0.00971812723319204));
#29300=CARTESIAN_POINT('Ctrl Pts',(0.00158170838481421,-0.0405787743898723,
-0.00977423237411966));
#29301=CARTESIAN_POINT('Ctrl Pts',(0.0016894090238867,-0.0405787743898723,
-0.00983801248702863));
#29302=CARTESIAN_POINT('Ctrl Pts',(0.00203095285777748,-0.0405787743898723,
-0.0100402740936126));
#29303=CARTESIAN_POINT('Ctrl Pts',(0.00233296277669372,-0.0405787743898723,
-0.0103094920811301));
#29304=CARTESIAN_POINT('Ctrl Pts',(0.00257120062921594,-0.0405787743898723,
-0.0106266352500323));
#29305=CARTESIAN_POINT('Origin',(0.006,-0.0408432743898723,-0.0121758532865581));
#29306=CARTESIAN_POINT('Ctrl Pts',(0.0066708408081868,-0.0408432743898723,
-0.0135653933579743));
#29307=CARTESIAN_POINT('Ctrl Pts',(0.00644291256165282,-0.0408432743898723,
-0.0136513645485826));
#29308=CARTESIAN_POINT('Ctrl Pts',(0.0061939241669469,-0.0408432743898723,
-0.0136786575412909));
#29309=CARTESIAN_POINT('Ctrl Pts',(0.00595206629017699,-0.0408432743898723,
-0.0136486405340303));
#29310=CARTESIAN_POINT('Ctrl Pts',(0.0057959164633947,-0.0408432743898723,
-0.0136292607621292));
#29311=CARTESIAN_POINT('Ctrl Pts',(0.00564276939617046,-0.0408432743898723,
-0.0135859598764373));
#29312=CARTESIAN_POINT('Ctrl Pts',(0.00550095178366503,-0.0408432743898723,
-0.0135187810726581));
#29313=CARTESIAN_POINT('Ctrl Pts',(0.00542311044837692,-0.0408432743898723,
-0.0134819077415052));
#29314=CARTESIAN_POINT('Ctrl Pts',(0.00534758693333899,-0.0408432743898723,
-0.0134369783461034));
#29315=CARTESIAN_POINT('Ctrl Pts',(0.00527959366954842,-0.0408432743898723,
-0.0133868303201724));
#29316=CARTESIAN_POINT('Ctrl Pts',(0.00518003238464839,-0.0408432743898723,
-0.0133133994886672));
#29317=CARTESIAN_POINT('Ctrl Pts',(0.0051027042655517,-0.0408432743898723,
-0.0132342662983514));
#29318=CARTESIAN_POINT('Ctrl Pts',(0.00504408437945305,-0.0408432743898723,
-0.0131635163957752));
#29319=CARTESIAN_POINT('Ctrl Pts',(0.00500661674994715,-0.0408432743898723,
-0.0131182957153248));
#29320=CARTESIAN_POINT('Ctrl Pts',(0.00497754696327898,-0.0408432743898723,
-0.0130777006059599));
#29321=CARTESIAN_POINT('Ctrl Pts',(0.00495287577896128,-0.0408432743898723,
-0.0130402400194263));
#29322=CARTESIAN_POINT('Ctrl Pts',(0.0048661367091343,-0.0408432743898723,
-0.0129085359070798));
#29323=CARTESIAN_POINT('Ctrl Pts',(0.00480112740676211,-0.0408432743898723,
-0.0127617780100069));
#29324=CARTESIAN_POINT('Ctrl Pts',(0.00476339054481838,-0.0408432743898723,
-0.012608747868102));
#29325=CARTESIAN_POINT('Ctrl Pts',(0.00473186775269151,-0.0408432743898723,
-0.0124809169594376));
#29326=CARTESIAN_POINT('Ctrl Pts',(0.00472093115928062,-0.0408432743898723,
-0.0123552969347836));
#29327=CARTESIAN_POINT('Ctrl Pts',(0.00472819748833167,-0.0408432743898723,
-0.0122359809577845));
#29328=CARTESIAN_POINT('Ctrl Pts',(0.00472941863046114,-0.0408432743898723,
-0.0122159293243933));
#29329=CARTESIAN_POINT('Ctrl Pts',(0.00473115808435559,-0.0408432743898723,
-0.0121959887117323));
#29330=CARTESIAN_POINT('Ctrl Pts',(0.00473339895604038,-0.0408432743898723,
-0.0121761426976128));
#29331=CARTESIAN_POINT('Ctrl Pts',(0.00510586347518963,-0.0408432743898723,
-0.0112817167617477));
#29332=CARTESIAN_POINT('Ctrl Pts',(0.00523985302939051,-0.0408432743898723,
-0.0111149436690097));
#29333=CARTESIAN_POINT('Ctrl Pts',(0.00541836403085339,-0.0408432743898723,
-0.010986190403829));
#29334=CARTESIAN_POINT('Ctrl Pts',(0.00561597474088275,-0.0408432743898723,
-0.0109031332635979));
#29335=CARTESIAN_POINT('Ctrl Pts',(0.0057127184838363,-0.0408432743898723,
-0.0108624712032076));
#29336=CARTESIAN_POINT('Ctrl Pts',(0.00581188031817111,-0.0408432743898723,
-0.010833090617441));
#29337=CARTESIAN_POINT('Ctrl Pts',(0.00591786028704338,-0.0408432743898723,
-0.0108147439575407));
#29338=CARTESIAN_POINT('Ctrl Pts',(0.00602835712854006,-0.0408432743898723,
-0.0107956153618959));
#29339=CARTESIAN_POINT('Ctrl Pts',(0.00615352503003078,-0.0408432743898723,
-0.0107875324977288));
#29340=CARTESIAN_POINT('Ctrl Pts',(0.00628985470781804,-0.0408432743898723,
-0.0108025493456774));
#29341=CARTESIAN_POINT('Ctrl Pts',(0.00640764562415654,-0.0408432743898723,
-0.0108155241308385));
#29342=CARTESIAN_POINT('Ctrl Pts',(0.00653154785488207,-0.0408432743898723,
-0.0108469563098139));
#29343=CARTESIAN_POINT('Ctrl Pts',(0.00664639836621562,-0.0408432743898723,
-0.0108929699340679));
#29344=CARTESIAN_POINT('Ctrl Pts',(0.00684726066682443,-0.0408432743898723,
-0.0109734432582151));
#29345=CARTESIAN_POINT('Ctrl Pts',(0.00703025890384745,-0.0408432743898723,
-0.011098646305903));
#29346=CARTESIAN_POINT('Ctrl Pts',(0.00718006637589825,-0.0408432743898723,
-0.0112550411609207));
#29347=CARTESIAN_POINT('Ctrl Pts',(0.00728593172218851,-0.0408432743898723,
-0.011365561652708));
#29348=CARTESIAN_POINT('Ctrl Pts',(0.00737184727087407,-0.0408432743898723,
-0.0114874543259832));
#29349=CARTESIAN_POINT('Ctrl Pts',(0.00743748127739367,-0.0408432743898723,
-0.0116201260411841));
#29350=CARTESIAN_POINT('Ctrl Pts',(0.00744482695207721,-0.0408432743898723,
-0.0116349744911151));
#29351=CARTESIAN_POINT('Ctrl Pts',(0.00745192010089368,-0.0408432743898723,
-0.0116499769291171));
#29352=CARTESIAN_POINT('Ctrl Pts',(0.0074587645768567,-0.0408432743898723,
-0.0116651389210321));
#29353=CARTESIAN_POINT('Origin',(0.0076,-0.0412787743898723,-0.00457585328655813));
#29354=CARTESIAN_POINT('Origin',(0.008,-0.0412787743898723,-0.00417585328655813));
#29355=CARTESIAN_POINT('',(0.00800000000001,-0.0301787743898623,-0.00817585328656812));
#29356=CARTESIAN_POINT('Origin',(0.0076,-0.0412787743898723,-0.0197758532865581));
#29357=CARTESIAN_POINT('Origin',(0.0076,-0.0301787743898723,-0.0201758532865581));
#29358=CARTESIAN_POINT('',(0.00800000000001,-0.0301787743898623,-0.0197758532865681));
#29359=CARTESIAN_POINT('Origin',(-0.0035,-0.0297787743898723,-0.0121758532865581));
#29360=CARTESIAN_POINT('',(0.00760000000001,-0.0297787743898623,-0.00817585328656812));
#29361=CARTESIAN_POINT('',(-0.01459999999999,-0.0297787743898623,-0.0161758532865681));
#29362=CARTESIAN_POINT('',(-0.00320000000001762,-0.0297787743898547,-0.0121758532865581));
#29363=CARTESIAN_POINT('Origin',(1.00024155624823E-14,-0.0297787743898623,
-0.0121758532865681));
#29364=CARTESIAN_POINT('',(-0.0142000000000176,-0.0297787743898547,-0.0121758532865581));
#29365=CARTESIAN_POINT('Origin',(-0.01249999999999,-0.0297787743898623,
-0.0121758532865681));
#29366=CARTESIAN_POINT('Origin',(-0.015,-0.0301787743898723,-0.0197758532865581));
#29367=CARTESIAN_POINT('',(-0.01459999999999,-0.0297787743898623,-0.0197758532865681));
#29368=CARTESIAN_POINT('Origin',(-0.015,-0.0412787743898723,-0.0201758532865581));
#29369=CARTESIAN_POINT('',(-0.015,-0.0301787743898623,-0.0161758532865681));
#29370=CARTESIAN_POINT('Origin',(-0.0125,-0.0375520664398416,-0.0121758532865581));
#29371=CARTESIAN_POINT('',(-0.0140429999982064,-0.0363035190698315,-0.0121757788889842));
#29372=CARTESIAN_POINT('Ctrl Pts',(-0.014043,-0.0363035228772662,-0.012175853286558));
#29373=CARTESIAN_POINT('Ctrl Pts',(-0.014043,-0.0363035216081401,-0.0121758284873666));
#29374=CARTESIAN_POINT('Ctrl Pts',(-0.0140429999994021,-0.0363035203389952,
-0.0121758036881753));
#29375=CARTESIAN_POINT('Ctrl Pts',(-0.0140429999982064,-0.0363035190698315,
-0.0121757788889841));
#29376=CARTESIAN_POINT('Ctrl Pts',(-0.0140429999982064,-0.0363035190698315,
-0.0121757788889842));
#29377=CARTESIAN_POINT('Ctrl Pts',(-0.0140429995987208,-0.03630309504786,
-0.0121674935888125));
#29378=CARTESIAN_POINT('Ctrl Pts',(-0.0140429325737997,-0.0363026694551463,
-0.0121592185236324));
#29379=CARTESIAN_POINT('Ctrl Pts',(-0.0140426306945938,-0.0363017033307592,
-0.0121405282383409));
#29380=CARTESIAN_POINT('Ctrl Pts',(-0.0140423573365181,-0.0363011621194678,
-0.0121301241024859));
#29381=CARTESIAN_POINT('Ctrl Pts',(-0.0140411875071023,-0.0362994795614532,
-0.0120979868273761));
#29382=CARTESIAN_POINT('Ctrl Pts',(-0.0140399367540347,-0.036298327231832,
-0.0120762699238923));
#29383=CARTESIAN_POINT('Ctrl Pts',(-0.0140299305721976,-0.0362915005031093,
-0.0119493439846875));
#29384=CARTESIAN_POINT('Ctrl Pts',(-0.0140108559444092,-0.0362855032348445,
-0.011845244152624));
#29385=CARTESIAN_POINT('Ctrl Pts',(-0.0139628756321997,-0.0362756526337917,
-0.0116806953806947));
#29386=CARTESIAN_POINT('Ctrl Pts',(-0.0139404098438068,-0.0362718583152341,
-0.0116187118331264));
#29387=CARTESIAN_POINT('Ctrl Pts',(-0.0139013033997271,-0.036266405575857,
-0.0115291598057157));
#29388=CARTESIAN_POINT('Ctrl Pts',(-0.0138876538029265,-0.0362646578194073,
-0.0115003676365055));
#29389=CARTESIAN_POINT('Ctrl Pts',(-0.0138691932555083,-0.036262497376662,
-0.0114643527577709));
#29390=CARTESIAN_POINT('Ctrl Pts',(-0.0138652005395636,-0.03626204110314,
-0.0114567214023763));
#29391=CARTESIAN_POINT('Ctrl Pts',(-0.0138586660477047,-0.0362613122907672,
-0.011444482483014));
#29392=CARTESIAN_POINT('Ctrl Pts',(-0.0138561642881782,-0.0362610373492196,
-0.0114398538935162));
#29393=CARTESIAN_POINT('Ctrl Pts',(-0.0138512935016634,-0.0362605100001696,
-0.0114309514482718));
#29394=CARTESIAN_POINT('Ctrl Pts',(-0.0138489277927363,-0.0362602574052702,
-0.0114266759466823));
#29395=CARTESIAN_POINT('Ctrl Pts',(-0.0138430736484742,-0.0362596407828723,
-0.0114162134897503));
#29396=CARTESIAN_POINT('Ctrl Pts',(-0.0138395626813316,-0.0362592781736722,
-0.0114100391624586));
#29397=CARTESIAN_POINT('Ctrl Pts',(-0.0138273285772317,-0.0362580383913607,
-0.0113888660601725));
#29398=CARTESIAN_POINT('Ctrl Pts',(-0.0138183948907351,-0.0362571737259045,
-0.0113739898283539));
#29399=CARTESIAN_POINT('Ctrl Pts',(-0.0137322308887414,-0.036249174949193,
-0.0112358453145593));
#29400=CARTESIAN_POINT('Ctrl Pts',(-0.0136381774313634,-0.0362428638621241,
-0.0111239166007904));
#29401=CARTESIAN_POINT('Ctrl Pts',(-0.0135017800160587,-0.0362342750410312,
-0.0110016708600523));
#29402=CARTESIAN_POINT('Ctrl Pts',(-0.0134728226373155,-0.0362324821888421,
-0.0109775697401679));
#29403=CARTESIAN_POINT('Ctrl Pts',(-0.0134218449267673,-0.0362293496275276,
-0.0109382078555016));
#29404=CARTESIAN_POINT('Ctrl Pts',(-0.0134002556650593,-0.0362280298575219,
-0.0109224164460669));
#29405=CARTESIAN_POINT('Ctrl Pts',(-0.0133687119399263,-0.0362261055605039,
-0.0109005793397179));
#29406=CARTESIAN_POINT('Ctrl Pts',(-0.0133590819284627,-0.036225518625291,
-0.0108940723751991));
#29407=CARTESIAN_POINT('Ctrl Pts',(-0.0133421521230947,-0.0362244872862137,
-0.0108829094570772));
#29408=CARTESIAN_POINT('Ctrl Pts',(-0.0133348848759541,-0.0362240447375029,
-0.0108782049580479));
#29409=CARTESIAN_POINT('Ctrl Pts',(-0.0133197761820495,-0.0362231248393869,
-0.0108686037037348));
#29410=CARTESIAN_POINT('Ctrl Pts',(-0.0133119295597613,-0.0362226471858507,
-0.0108637157764484));
#29411=CARTESIAN_POINT('Ctrl Pts',(-0.0132915687334052,-0.0362214077789512,
-0.0108512848914695));
#29412=CARTESIAN_POINT('Ctrl Pts',(-0.0132789906524162,-0.0362206421499758,
-0.0108438487683383));
#29413=CARTESIAN_POINT('Ctrl Pts',(-0.0132261471095531,-0.0362174248421312,
-0.0108136123180992));
#29414=CARTESIAN_POINT('Ctrl Pts',(-0.013184974933425,-0.0362149154202119,
-0.0107924521084515));
#29415=CARTESIAN_POINT('Ctrl Pts',(-0.0130495141989045,-0.0362066586971812,
-0.0107303637406961));
#29416=CARTESIAN_POINT('Ctrl Pts',(-0.0129520745200486,-0.0362006991898911,
-0.0106969919173001));
#29417=CARTESIAN_POINT('Ctrl Pts',(-0.0127936055887318,-0.036191375902033,
-0.0106598556981046));
#29418=CARTESIAN_POINT('Ctrl Pts',(-0.0127344017609904,-0.0361879763827394,
-0.0106495800797282));
#29419=CARTESIAN_POINT('Ctrl Pts',(-0.0126611378304009,-0.036183982981313,
-0.0106412291701596));
#29420=CARTESIAN_POINT('Ctrl Pts',(-0.0126475094785747,-0.0361832492079286,
-0.010639859289788));
#29421=CARTESIAN_POINT('Ctrl Pts',(-0.0126276017009878,-0.0361821923412473,
-0.0106381256374585));
#29422=CARTESIAN_POINT('Ctrl Pts',(-0.012621335773148,-0.0361818618585971,
-0.0106376185353679));
#29423=CARTESIAN_POINT('Ctrl Pts',(-0.0126102740648317,-0.0361812824627403,
-0.0106367913223943));
#29424=CARTESIAN_POINT('Ctrl Pts',(-0.0126054796538431,-0.0361810326829888,
-0.0106364553056877));
#29425=CARTESIAN_POINT('Ctrl Pts',(-0.0125950543010995,-0.036180492503163,
-0.0106357735795657));
#29426=CARTESIAN_POINT('Ctrl Pts',(-0.01258942297963,-0.0361802025727367,
-0.0106354363440624));
#29427=CARTESIAN_POINT('Ctrl Pts',(-0.0125736493454721,-0.0361793953341253,
-0.0106345785194115));
#29428=CARTESIAN_POINT('Ctrl Pts',(-0.012563503387812,-0.0361788817364137,
-0.0106341271552065));
#29429=CARTESIAN_POINT('Ctrl Pts',(-0.0124975830130454,-0.0361755771902464,
-0.0106318464134615));
#29430=CARTESIAN_POINT('Ctrl Pts',(-0.0124417436970142,-0.03617292787673,
-0.0106329435746703));
#29431=CARTESIAN_POINT('Ctrl Pts',(-0.0123603292422337,-0.0361691335567524,
-0.010638970749754));
#29432=CARTESIAN_POINT('Ctrl Pts',(-0.0123346277314895,-0.0361679459048419,
-0.010641523495776));
#29433=CARTESIAN_POINT('Ctrl Pts',(-0.0122451012455231,-0.0361638121181602,
-0.0106526912869685));
#29434=CARTESIAN_POINT('Ctrl Pts',(-0.0121817623607875,-0.0361608904467523,
-0.0106646549167043));
#29435=CARTESIAN_POINT('Ctrl Pts',(-0.012076874194689,-0.0361558565449464,
-0.0106913549392201));
#29436=CARTESIAN_POINT('Ctrl Pts',(-0.0120348730263031,-0.0361537867317166,
-0.0107039744334159));
#29437=CARTESIAN_POINT('Ctrl Pts',(-0.0119652722616709,-0.0361502203473588,
-0.0107281633143499));
#29438=CARTESIAN_POINT('Ctrl Pts',(-0.0119373682843611,-0.0361487525382031,
-0.0107387779869717));
#29439=CARTESIAN_POINT('Ctrl Pts',(-0.0118986011461219,-0.036146651323729,
-0.010754827218869));
#29440=CARTESIAN_POINT('Ctrl Pts',(-0.0118874666740248,-0.0361460405059185,
-0.0107595911002697));
#29441=CARTESIAN_POINT('Ctrl Pts',(-0.0118684049991676,-0.0361449816844189,
-0.0107680134675328));
#29442=CARTESIAN_POINT('Ctrl Pts',(-0.0118604505613438,-0.0361445358540261,
-0.0107716091081905));
#29443=CARTESIAN_POINT('Ctrl Pts',(-0.0118443022031949,-0.0361436224505098,
-0.0107790743108959));
#29444=CARTESIAN_POINT('Ctrl Pts',(-0.0118361110137875,-0.0361431547138178,
-0.0107829489406442));
#29445=CARTESIAN_POINT('Ctrl Pts',(-0.011815539604574,-0.0361419686657032,
-0.010792902390383));
#29446=CARTESIAN_POINT('Ctrl Pts',(-0.011803206049612,-0.0361412470777422,
-0.0107990753857635));
#29447=CARTESIAN_POINT('Ctrl Pts',(-0.0117562952369704,-0.0361384613876635,
-0.0108233462496241));
#29448=CARTESIAN_POINT('Ctrl Pts',(-0.0117223285073193,-0.0361363572825881,
-0.0108425870932123));
#29449=CARTESIAN_POINT('Ctrl Pts',(-0.0115868358228125,-0.0361276040364828,
-0.0109262787436451));
#29450=CARTESIAN_POINT('Ctrl Pts',(-0.0114922853091864,-0.0361205972335303,
-0.0110012000843454));
#29451=CARTESIAN_POINT('Ctrl Pts',(-0.0113702319632128,-0.0361107339349849,
-0.0111235963987869));
#29452=CARTESIAN_POINT('Ctrl Pts',(-0.0113349883521476,-0.0361077717449535,
-0.0111627545188793));
#29453=CARTESIAN_POINT('Ctrl Pts',(-0.0112937047977956,-0.0361042303693944,
-0.0112136337190421));
#29454=CARTESIAN_POINT('Ctrl Pts',(-0.0112857213799507,-0.036103541949859,
-0.0112237282605686));
#29455=CARTESIAN_POINT('Ctrl Pts',(-0.0112741240199205,-0.0361025380222728,
-0.0112387755763679));
#29456=CARTESIAN_POINT('Ctrl Pts',(-0.011270411985179,-0.036102216085183,
-0.0112436516614767));
#29457=CARTESIAN_POINT('Ctrl Pts',(-0.011264124086186,-0.0361016699009137,
-0.0112520142778883));
#29458=CARTESIAN_POINT('Ctrl Pts',(-0.0112615337433139,-0.0361014446541618,
-0.0112554897058278));
#29459=CARTESIAN_POINT('Ctrl Pts',(-0.0112556520156969,-0.036100932670152,
-0.0112634509371026));
#29460=CARTESIAN_POINT('Ctrl Pts',(-0.0112523702214137,-0.0361006465946965,
-0.0112679436595548));
#29461=CARTESIAN_POINT('Ctrl Pts',(-0.0112433780333029,-0.0360998613178757,
-0.011280394648733));
#29462=CARTESIAN_POINT('Ctrl Pts',(-0.0112377189156356,-0.0360993655033892,
-0.0112883898153702));
#29463=CARTESIAN_POINT('Ctrl Pts',(-0.0112056838884276,-0.0360965461215234,
-0.0113345751350492));
#29464=CARTESIAN_POINT('Ctrl Pts',(-0.0111809635622188,-0.0360943198979953,
-0.0113738890186394));
#29465=CARTESIAN_POINT('Ctrl Pts',(-0.0111186096703849,-0.0360883944281096,
-0.0114837583639859));
#29466=CARTESIAN_POINT('Ctrl Pts',(-0.011084624935768,-0.0360847953911461,
-0.0115562171575177));
#29467=CARTESIAN_POINT('Ctrl Pts',(-0.0110290236848174,-0.0360775554291241,
-0.0117035290877667));
#29468=CARTESIAN_POINT('Ctrl Pts',(-0.0110071517273209,-0.0360739282113978,
-0.0117780292647345));
#29469=CARTESIAN_POINT('Ctrl Pts',(-0.0109866243092998,-0.0360690960564971,
-0.0118742291234214));
#29470=CARTESIAN_POINT('Ctrl Pts',(-0.0109826895721706,-0.0360680604689365,
-0.0118946911793152));
#29471=CARTESIAN_POINT('Ctrl Pts',(-0.0109773892129962,-0.03606648090869,
-0.0119256201905137));
#29472=CARTESIAN_POINT('Ctrl Pts',(-0.0109757145858098,-0.0360659467598764,
-0.0119360321449306));
#29473=CARTESIAN_POINT('Ctrl Pts',(-0.0109728790368387,-0.036064974501252,
-0.0119548933625149));
#29474=CARTESIAN_POINT('Ctrl Pts',(-0.0109716811795748,-0.0360645375862603,
-0.0119633366909382));
#29475=CARTESIAN_POINT('Ctrl Pts',(-0.0109692547598527,-0.0360635927634442,
-0.011981522561878));
#29476=CARTESIAN_POINT('Ctrl Pts',(-0.0109680490903508,-0.0360630841489514,
-0.0119912677367114));
#29477=CARTESIAN_POINT('Ctrl Pts',(-0.0109650285093156,-0.0360616952299219,
-0.0120177549009252));
#29478=CARTESIAN_POINT('Ctrl Pts',(-0.0109633945624542,-0.0360608092650984,
-0.0120345158333276));
#29479=CARTESIAN_POINT('Ctrl Pts',(-0.0109545266090645,-0.0360549735842397,
-0.0121440157010463));
#29480=CARTESIAN_POINT('Ctrl Pts',(-0.0109554182214037,-0.0360497672504841,
-0.0122372073786588));
#29481=CARTESIAN_POINT('Ctrl Pts',(-0.0109713658684127,-0.0360406147123997,
-0.0123963155300473));
#29482=CARTESIAN_POINT('Ctrl Pts',(-0.0109823622024224,-0.0360367391193339,
-0.0124623868104888));
#29483=CARTESIAN_POINT('Ctrl Pts',(-0.0110091177740337,-0.0360300702925261,
-0.0125766866408892));
#29484=CARTESIAN_POINT('Ctrl Pts',(-0.011023029248533,-0.0360272500713398,
-0.0126252478299691));
#29485=CARTESIAN_POINT('Ctrl Pts',(-0.0110424454972302,-0.0360240207758172,
-0.0126822911458022));
#29486=CARTESIAN_POINT('Ctrl Pts',(-0.0110456811354356,-0.0360235016189537,
-0.0126915092606584));
#29487=CARTESIAN_POINT('Ctrl Pts',(-0.0110508756971738,-0.0360226977427472,
-0.0127058702940551));
#29488=CARTESIAN_POINT('Ctrl Pts',(-0.0110527749018212,-0.0360224096804733,
-0.0127110343683717));
#29489=CARTESIAN_POINT('Ctrl Pts',(-0.0110563954798538,-0.0360218715075487,
-0.0127207187596324));
#29490=CARTESIAN_POINT('Ctrl Pts',(-0.01105811048303,-0.0360216210530846,
-0.0127252411418428));
#29491=CARTESIAN_POINT('Ctrl Pts',(-0.0110621502130185,-0.0360210412683744,
-0.0127357444931532));
#29492=CARTESIAN_POINT('Ctrl Pts',(-0.0110644910138327,-0.03602071289796,
-0.0127417191068715));
#29493=CARTESIAN_POINT('Ctrl Pts',(-0.0110721430617942,-0.0360196629484713,
-0.0127608969534907));
#29494=CARTESIAN_POINT('Ctrl Pts',(-0.0110775998570417,-0.0360189495545451,
-0.0127740417088676));
#29495=CARTESIAN_POINT('Ctrl Pts',(-0.0111138261826433,-0.0360144216590649,
-0.0128580066357587));
#29496=CARTESIAN_POINT('Ctrl Pts',(-0.011149696181361,-0.0360108577377136,
-0.0129265149499834));
#29497=CARTESIAN_POINT('Ctrl Pts',(-0.0112271598202884,-0.0360041510072435,
-0.0130507917643758));
#29498=CARTESIAN_POINT('Ctrl Pts',(-0.0112676818787368,-0.0360010098393769,
-0.0131069984197846));
#29499=CARTESIAN_POINT('Ctrl Pts',(-0.0113500409910983,-0.0359949745492503,
-0.0132064009933315));
#29500=CARTESIAN_POINT('Ctrl Pts',(-0.0113908911369384,-0.0359921099933848,
-0.0132502418920114));
#29501=CARTESIAN_POINT('Ctrl Pts',(-0.0114452528738829,-0.0359883753994694,
-0.0133021711261851));
#29502=CARTESIAN_POINT('Ctrl Pts',(-0.0114564795577272,-0.0359876081218057,
-0.0133125803607398));
#29503=CARTESIAN_POINT('Ctrl Pts',(-0.01147484010386,-0.0359863586370829,
-0.0133291027776311));
#29504=CARTESIAN_POINT('Ctrl Pts',(-0.0114818782892177,-0.0359858809038878,
-0.013335320999878));
#29505=CARTESIAN_POINT('Ctrl Pts',(-0.0114954693582739,-0.0359849605092637,
-0.0133471095137818));
#29506=CARTESIAN_POINT('Ctrl Pts',(-0.0115020129210706,-0.0359845183011864,
-0.0133526900408555));
#29507=CARTESIAN_POINT('Ctrl Pts',(-0.0115170844901004,-0.0359835017207827,
-0.0133653273803864));
#29508=CARTESIAN_POINT('Ctrl Pts',(-0.0115256423996949,-0.0359829258838647,
-0.0133723476566219));
#29509=CARTESIAN_POINT('Ctrl Pts',(-0.0115487225954577,-0.0359813762900012,
-0.0133908691113019));
#29510=CARTESIAN_POINT('Ctrl Pts',(-0.0115633774001219,-0.0359803958916534,
-0.0134022016138494));
#29511=CARTESIAN_POINT('Ctrl Pts',(-0.0116750923253533,-0.0359729465043413,
-0.0134854196959764));
#29512=CARTESIAN_POINT('Ctrl Pts',(-0.0117800754417224,-0.0359660328372556,
-0.0135459396171147));
#29513=CARTESIAN_POINT('Ctrl Pts',(-0.0119435297002618,-0.0359558018743863,
-0.0136161505507782));
#29514=CARTESIAN_POINT('Ctrl Pts',(-0.0119972577903227,-0.0359525246206751,
-0.0136357732434587));
#29515=CARTESIAN_POINT('Ctrl Pts',(-0.01208002868533,-0.0359477114662054,
-0.0136608899638922));
#29516=CARTESIAN_POINT('Ctrl Pts',(-0.0121083436564838,-0.0359461056270923,
-0.0136686075730028));
#29517=CARTESIAN_POINT('Ctrl Pts',(-0.0121449907778423,-0.0359440940928235,
-0.0136774815309303));
#29518=CARTESIAN_POINT('Ctrl Pts',(-0.012153134478864,-0.0359436512919703,
-0.013679383548484));
#29519=CARTESIAN_POINT('Ctrl Pts',(-0.0121663586259715,-0.0359429395053464,
-0.0136823589748054));
#29520=CARTESIAN_POINT('Ctrl Pts',(-0.0121714296287183,-0.0359426682819566,
-0.0136834730887209));
#29521=CARTESIAN_POINT('Ctrl Pts',(-0.0121812992090917,-0.0359421438836818,
-0.0136855893014541));
#29522=CARTESIAN_POINT('Ctrl Pts',(-0.0121860970720809,-0.0359418905632593,
-0.0136865941581665));
#29523=CARTESIAN_POINT('Ctrl Pts',(-0.0121968466705296,-0.0359413264305017,
-0.0136887921168352));
#29524=CARTESIAN_POINT('Ctrl Pts',(-0.0122028008832575,-0.0359410163031011,
-0.0136899730086087));
#29525=CARTESIAN_POINT('Ctrl Pts',(-0.0122235754086168,-0.0359399419415139,
-0.0136939659268531));
#29526=CARTESIAN_POINT('Ctrl Pts',(-0.0122384302894439,-0.0359391873207996,
-0.013696595822847));
#29527=CARTESIAN_POINT('Ctrl Pts',(-0.0123998461531614,-0.0359311117314028,
-0.0137227374729462));
#29528=CARTESIAN_POINT('Ctrl Pts',(-0.0125490438585983,-0.035924687387436,
-0.0137252042013086));
#29529=CARTESIAN_POINT('Ctrl Pts',(-0.0127338478242501,-0.0359159540341034,
-0.013701499497371));
#29530=CARTESIAN_POINT('Ctrl Pts',(-0.0127711927113669,-0.035914153245928,
-0.0136953056371316));
#29531=CARTESIAN_POINT('Ctrl Pts',(-0.0128345677915181,-0.0359110081064292,
-0.0136823836313994));
#29532=CARTESIAN_POINT('Ctrl Pts',(-0.0128607194264732,-0.0359096839505254,
-0.0136763367669058));
#29533=CARTESIAN_POINT('Ctrl Pts',(-0.0128979612624479,-0.0359077545917146,
-0.0136666957224692));
#29534=CARTESIAN_POINT('Ctrl Pts',(-0.0129091898275224,-0.0359071671388194,
-0.0136636530078299));
#29535=CARTESIAN_POINT('Ctrl Pts',(-0.0129287096730245,-0.0359061354412712,
-0.0136581258369899));
#29536=CARTESIAN_POINT('Ctrl Pts',(-0.0129370165256779,-0.03590569306243,
-0.0136556980249516));
#29537=CARTESIAN_POINT('Ctrl Pts',(-0.0129530712650107,-0.0359048314494076,
-0.013650858800963));
#29538=CARTESIAN_POINT('Ctrl Pts',(-0.012960821430074,-0.0359044125073906,
-0.0136484558958556));
#29539=CARTESIAN_POINT('Ctrl Pts',(-0.0129814569729196,-0.0359032888339924,
-0.0136418790820071));
#29540=CARTESIAN_POINT('Ctrl Pts',(-0.0129943067553862,-0.0359025805331877,
-0.0136375965148469));
#29541=CARTESIAN_POINT('Ctrl Pts',(-0.0130421280175331,-0.0358999116794568,
-0.0136209560098568));
#29542=CARTESIAN_POINT('Ctrl Pts',(-0.0130767046633142,-0.0358979153612362,
-0.0136075083022656));
#29543=CARTESIAN_POINT('Ctrl Pts',(-0.0132230101712836,-0.0358891796574392,
-0.0135444459813325));
#29544=CARTESIAN_POINT('Ctrl Pts',(-0.013329103801223,-0.0358820586361552,
-0.0134828994582018));
#29545=CARTESIAN_POINT('Ctrl Pts',(-0.013469156271715,-0.0358720619017414,
-0.0133776814048846));
#29546=CARTESIAN_POINT('Ctrl Pts',(-0.0135098426280364,-0.0358690807626917,
-0.0133437032170579));
#29547=CARTESIAN_POINT('Ctrl Pts',(-0.0135581741855435,-0.0358655192881218,
-0.013298921892953));
#29548=CARTESIAN_POINT('Ctrl Pts',(-0.013567534863224,-0.0358648285682008,
-0.0132900278863636));
#29549=CARTESIAN_POINT('Ctrl Pts',(-0.0135811805094935,-0.0358638217688148,
-0.0132767326623448));
#29550=CARTESIAN_POINT('Ctrl Pts',(-0.0135855523902188,-0.0358634992208278,
-0.013272421891237));
#29551=CARTESIAN_POINT('Ctrl Pts',(-0.0135929690097306,-0.0358629522602076,
-0.01326502111551));
#29552=CARTESIAN_POINT('Ctrl Pts',(-0.0135960265954076,-0.0358627268422441,
-0.0132619442217293));
#29553=CARTESIAN_POINT('Ctrl Pts',(-0.0136029734890203,-0.0358622148854447,
-0.013254894246076));
#29554=CARTESIAN_POINT('Ctrl Pts',(-0.0136068543304453,-0.0358619290044352,
-0.0132509130071594));
#29555=CARTESIAN_POINT('Ctrl Pts',(-0.0136175014635884,-0.0358611447291482,
-0.0132398716620225));
#29556=CARTESIAN_POINT('Ctrl Pts',(-0.0136242223966772,-0.0358606497083555,
-0.0132327679645763));
#29557=CARTESIAN_POINT('Ctrl Pts',(-0.0136622344212292,-0.0358578469754445,
-0.0131918182392619));
#29558=CARTESIAN_POINT('Ctrl Pts',(-0.0136920664185269,-0.0358556352636389,
-0.0131566447847472));
#29559=CARTESIAN_POINT('Ctrl Pts',(-0.0137693193746737,-0.0358497125445119,
-0.0130568173425352));
#29560=CARTESIAN_POINT('Ctrl Pts',(-0.0138133489278706,-0.035846103934367,
-0.0129897235680702));
#29561=CARTESIAN_POINT('Ctrl Pts',(-0.0138929012330122,-0.035838514677895,
-0.0128450976560723));
#29562=CARTESIAN_POINT('Ctrl Pts',(-0.013927616219135,-0.0358345345281592,
-0.0127674373678192));
#29563=CARTESIAN_POINT('Ctrl Pts',(-0.0139612583895272,-0.0358295068755572,
-0.0126716835632191));
#29564=CARTESIAN_POINT('Ctrl Pts',(-0.0139665002655861,-0.0358286779049506,
-0.0126559581588717));
#29565=CARTESIAN_POINT('Ctrl Pts',(-0.0139743956968318,-0.0358273523746311,
-0.0126309353962905));
#29566=CARTESIAN_POINT('Ctrl Pts',(-0.013977217030481,-0.0358268613558079,
-0.0126216920878426));
#29567=CARTESIAN_POINT('Ctrl Pts',(-0.0139823682783781,-0.0358259309073835,
-0.012604229594541));
#29568=CARTESIAN_POINT('Ctrl Pts',(-0.0139847171341991,-0.035825492120375,
-0.0125960163519055));
#29569=CARTESIAN_POINT('Ctrl Pts',(-0.0139898706629757,-0.0358244954699947,
-0.0125774130229305));
#29570=CARTESIAN_POINT('Ctrl Pts',(-0.0139926350580568,-0.03582393631605,
-0.0125670123204707));
#29571=CARTESIAN_POINT('Ctrl Pts',(-0.0140005286689846,-0.0358222635479209,
-0.0125360107526621));
#29572=CARTESIAN_POINT('Ctrl Pts',(-0.0140053416275327,-0.0358211398215695,
-0.0125153326093378));
#29573=CARTESIAN_POINT('Ctrl Pts',(-0.0140318429248073,-0.0358142675351953,
-0.012389795869212));
#29574=CARTESIAN_POINT('Ctrl Pts',(-0.014042991191137,-0.0358081827035411,
-0.0122830263609671));
#29575=CARTESIAN_POINT('Ctrl Pts',(-0.014043,-0.035802018678757,-0.012175853286457));
#29576=CARTESIAN_POINT('Ctrl Pts',(-0.014043,-0.0359172995678105,-0.0121758532865631));
#29577=CARTESIAN_POINT('Ctrl Pts',(-0.014043,-0.0359173084265614,-0.0121760097131553));
#29578=CARTESIAN_POINT('Ctrl Pts',(-0.0140429999762123,-0.0359173172857548,
-0.0121761661401342));
#29579=CARTESIAN_POINT('Ctrl Pts',(-0.0140429684641662,-0.0359231855911133,
-0.0122797780343122));
#29580=CARTESIAN_POINT('Ctrl Pts',(-0.0140325327356852,-0.0359292371515285,
-0.0123829630213215));
#29581=CARTESIAN_POINT('Ctrl Pts',(-0.0140045001279798,-0.0359371137793574,
-0.0125203535658078));
#29582=CARTESIAN_POINT('Ctrl Pts',(-0.0139958629864661,-0.0359391439549073,
-0.0125561102895848));
#29583=CARTESIAN_POINT('Ctrl Pts',(-0.0139834355650421,-0.0359416130535868,
-0.0126005360473383));
#29584=CARTESIAN_POINT('Ctrl Pts',(-0.0139808333466751,-0.0359421097241874,
-0.0126095226661828));
#29585=CARTESIAN_POINT('Ctrl Pts',(-0.0139765932965655,-0.0359428872444756,
-0.0126236821215912));
#29586=CARTESIAN_POINT('Ctrl Pts',(-0.013975009681435,-0.0359431710880598,
-0.0126288708032211));
#29587=CARTESIAN_POINT('Ctrl Pts',(-0.0139719495018691,-0.0359437072071874,
-0.0126387112355998));
#29588=CARTESIAN_POINT('Ctrl Pts',(-0.0139704782037362,-0.0359439597641907,
-0.0126433644304188));
#29589=CARTESIAN_POINT('Ctrl Pts',(-0.0139669203884198,-0.0359445583993516,
-0.0126544335726152));
#29590=CARTESIAN_POINT('Ctrl Pts',(-0.0139648138017627,-0.0359449033124146,
-0.012660843024175));
#29591=CARTESIAN_POINT('Ctrl Pts',(-0.0139574804935722,-0.0359460727355704,
-0.0126826714654573));
#29592=CARTESIAN_POINT('Ctrl Pts',(-0.0139520516555066,-0.0359468861625328,
-0.0126980219231832));
#29593=CARTESIAN_POINT('Ctrl Pts',(-0.0139380598086627,-0.0359488659028139,
-0.0127356779987292));
#29594=CARTESIAN_POINT('Ctrl Pts',(-0.0139292196291492,-0.0359500192383533,
-0.0127578765402717));
#29595=CARTESIAN_POINT('Ctrl Pts',(-0.0138881927526948,-0.0359550051373991,
-0.0128543200874838));
#29596=CARTESIAN_POINT('Ctrl Pts',(-0.0138507088334025,-0.0359586598786273,
-0.0129261754747037));
#29597=CARTESIAN_POINT('Ctrl Pts',(-0.0137568784338933,-0.0359667549029487,
-0.0130760183253592));
#29598=CARTESIAN_POINT('Ctrl Pts',(-0.013698538097385,-0.035971206151278,
-0.0131523492646557));
#29599=CARTESIAN_POINT('Ctrl Pts',(-0.0136221214083504,-0.0359767804573778,
-0.0132350858910033));
#29600=CARTESIAN_POINT('Ctrl Pts',(-0.0136105447111052,-0.0359776184010784,
-0.0132472171753907));
#29601=CARTESIAN_POINT('Ctrl Pts',(-0.0135918779662547,-0.0359789606820361,
-0.0132661504726461));
#29602=CARTESIAN_POINT('Ctrl Pts',(-0.013584916547098,-0.0359794593730415,
-0.0132730777518259));
#29603=CARTESIAN_POINT('Ctrl Pts',(-0.013571767802077,-0.0359803980496948,
-0.0132859145341878));
#29604=CARTESIAN_POINT('Ctrl Pts',(-0.0135655965113048,-0.0359808373052295,
-0.0132918399648914));
#29605=CARTESIAN_POINT('Ctrl Pts',(-0.0135516589585818,-0.0359818265948423,
-0.0133050012402238));
#29606=CARTESIAN_POINT('Ctrl Pts',(-0.0135438667168005,-0.0359823778180092,
-0.0133122088367204));
#29607=CARTESIAN_POINT('Ctrl Pts',(-0.0135203697653379,-0.0359840347598457,
-0.0133334972003947));
#29608=CARTESIAN_POINT('Ctrl Pts',(-0.0135044504946735,-0.0359851505275389,
-0.0133473365486772));
#29609=CARTESIAN_POINT('Ctrl Pts',(-0.0134272610448144,-0.0359905305136053,
-0.0134117106047961));
#29610=CARTESIAN_POINT('Ctrl Pts',(-0.0133624404701795,-0.0359949690584087,
-0.0134577854510251));
#29611=CARTESIAN_POINT('Ctrl Pts',(-0.0132223108652746,-0.0360043012555447,
-0.013541935631443));
#29612=CARTESIAN_POINT('Ctrl Pts',(-0.0131468377728911,-0.0360091907997271,
-0.0135792473344017));
#29613=CARTESIAN_POINT('Ctrl Pts',(-0.0130310415736704,-0.0360162145157066,
-0.0136251583234202));
#29614=CARTESIAN_POINT('Ctrl Pts',(-0.0129928049128773,-0.0360184595105425,
-0.0136386020881521));
#29615=CARTESIAN_POINT('Ctrl Pts',(-0.0129449067758753,-0.0360211441686762,
-0.0136533508679007));
#29616=CARTESIAN_POINT('Ctrl Pts',(-0.0129357063838397,-0.0360216541102725,
-0.0136560901251581));
#29617=CARTESIAN_POINT('Ctrl Pts',(-0.012921219468802,-0.0360224474124532,
-0.0136602565775855));
#29618=CARTESIAN_POINT('Ctrl Pts',(-0.0129159500376674,-0.0360227339724926,
-0.0136617417545478));
#29619=CARTESIAN_POINT('Ctrl Pts',(-0.0129059823901048,-0.0360232721173483,
-0.0136644939333971));
#29620=CARTESIAN_POINT('Ctrl Pts',(-0.0129012859861638,-0.0360235240205948,
-0.0136657667854144));
#29621=CARTESIAN_POINT('Ctrl Pts',(-0.0128901669822468,-0.0360241166336277,
-0.0136687239476847));
#29622=CARTESIAN_POINT('Ctrl Pts',(-0.0128837393290513,-0.036024456247394,
-0.0136703890724609));
#29623=CARTESIAN_POINT('Ctrl Pts',(-0.0128621621749092,-0.0360255869958932,
-0.013675830392529));
#29624=CARTESIAN_POINT('Ctrl Pts',(-0.0128469657106298,-0.0360263680332772,
-0.0136794182470108));
#29625=CARTESIAN_POINT('Ctrl Pts',(-0.0128096772733231,-0.0360282528572942,
-0.0136876265062317));
#29626=CARTESIAN_POINT('Ctrl Pts',(-0.0127875329909992,-0.0360293452530651,
-0.0136919941579886));
#29627=CARTESIAN_POINT('Ctrl Pts',(-0.0126939422214461,-0.0360338783876603,
-0.0137083292136836));
#29628=CARTESIAN_POINT('Ctrl Pts',(-0.0126217919625651,-0.0360371722565894,
-0.0137157441696818));
#29629=CARTESIAN_POINT('Ctrl Pts',(-0.0124507582954497,-0.0360449942503845,
-0.0137212209970137));
#29630=CARTESIAN_POINT('Ctrl Pts',(-0.012352061981371,-0.0360495310743024,
-0.0137149108726152));
#29631=CARTESIAN_POINT('Ctrl Pts',(-0.0122331556746266,-0.0360554375865097,
-0.0136957602466473));
#29632=CARTESIAN_POINT('Ctrl Pts',(-0.012211736147531,-0.0360565184461448,
-0.013691843706578));
#29633=CARTESIAN_POINT('Ctrl Pts',(-0.0121798698374775,-0.0360581547263099,
-0.0136853172227601));
#29634=CARTESIAN_POINT('Ctrl Pts',(-0.0121693554150916,-0.0360586992507125,
-0.0136830489760829));
#29635=CARTESIAN_POINT('Ctrl Pts',(-0.0121504996779944,-0.0360596844194159,
-0.0136787744796693));
#29636=CARTESIAN_POINT('Ctrl Pts',(-0.0121421496976041,-0.0360601237580958,
-0.0136768082308897));
#29637=CARTESIAN_POINT('Ctrl Pts',(-0.0121243464727108,-0.0360610672182272,
-0.0136724589341255));
#29638=CARTESIAN_POINT('Ctrl Pts',(-0.0121148985784008,-0.0360615719774445,
-0.0136700557246864));
#29639=CARTESIAN_POINT('Ctrl Pts',(-0.0120891986319751,-0.0360629563944502,
-0.0136632586315875));
#29640=CARTESIAN_POINT('Ctrl Pts',(-0.0120729950306185,-0.0360638417506793,
-0.0136586881223282));
#29641=CARTESIAN_POINT('Ctrl Pts',(-0.011968443115175,-0.0360696374109848,
-0.0136273416432165));
#29642=CARTESIAN_POINT('Ctrl Pts',(-0.0118825866640175,-0.0360748002806229,
-0.0135929515872037));
#29643=CARTESIAN_POINT('Ctrl Pts',(-0.0117171428438136,-0.0360854202819952,
-0.0135087803732864));
#29644=CARTESIAN_POINT('Ctrl Pts',(-0.0116379679362567,-0.0360908561655726,
-0.0134589983884585));
#29645=CARTESIAN_POINT('Ctrl Pts',(-0.0115418963141715,-0.0360975688297569,
-0.0133856648372971));
#29646=CARTESIAN_POINT('Ctrl Pts',(-0.0115204659908521,-0.0360990734352142,
-0.0133683800004309));
#29647=CARTESIAN_POINT('Ctrl Pts',(-0.0114930342625622,-0.0361009964526935,
-0.0133450159460462));
#29648=CARTESIAN_POINT('Ctrl Pts',(-0.0114866056476683,-0.0361014468862943,
-0.0133394482392113));
#29649=CARTESIAN_POINT('Ctrl Pts',(-0.01147628904584,-0.0361021688930658,
-0.0133303628639657));
#29650=CARTESIAN_POINT('Ctrl Pts',(-0.0114723724641684,-0.0361024427943175,
-0.0133268781043655));
#29651=CARTESIAN_POINT('Ctrl Pts',(-0.0114647613371767,-0.0361029745382788,
-0.0133200363262922));
#29652=CARTESIAN_POINT('Ctrl Pts',(-0.0114610652096871,-0.0361032325074985,
-0.01331668124008));
#29653=CARTESIAN_POINT('Ctrl Pts',(-0.0114520152452579,-0.0361038636917491,
-0.0133083858566633));
#29654=CARTESIAN_POINT('Ctrl Pts',(-0.011446679915248,-0.0361042354087775,
-0.0133034254002689));
#29655=CARTESIAN_POINT('Ctrl Pts',(-0.0114270579278263,-0.0361056019086352,
-0.0132849212904151));
#29656=CARTESIAN_POINT('Ctrl Pts',(-0.0114129951886707,-0.0361065801071223,
-0.0132711418945278));
#29657=CARTESIAN_POINT('Ctrl Pts',(-0.0113774380711826,-0.0361090624512274,
-0.0132349416272559));
#29658=CARTESIAN_POINT('Ctrl Pts',(-0.0113563494801813,-0.0361105436271254,
-0.013212133686451));
#29659=CARTESIAN_POINT('Ctrl Pts',(-0.0112900665192613,-0.0361152866218025,
-0.0131359567629314));
#29660=CARTESIAN_POINT('Ctrl Pts',(-0.0112478071716245,-0.0361184548574191,
-0.0130801494253951));
#29661=CARTESIAN_POINT('Ctrl Pts',(-0.0111579070747159,-0.0361259751813615,
-0.0129429819507985));
#29662=CARTESIAN_POINT('Ctrl Pts',(-0.0111136448225688,-0.0361303516688328,
-0.0128597514510496));
#29663=CARTESIAN_POINT('Ctrl Pts',(-0.0110707494608318,-0.0361358385312744,
-0.0127575517994717));
#29664=CARTESIAN_POINT('Ctrl Pts',(-0.0110645116010986,-0.0361366767583283,
-0.0127419833887681));
#29665=CARTESIAN_POINT('Ctrl Pts',(-0.0110550176752123,-0.036138020435348,
-0.0127171221209778));
#29666=CARTESIAN_POINT('Ctrl Pts',(-0.0110515945700138,-0.036138520272365,
-0.012707894238553));
#29667=CARTESIAN_POINT('Ctrl Pts',(-0.0110453506252458,-0.0361394617623763,
-0.0126905550800128));
#29668=CARTESIAN_POINT('Ctrl Pts',(-0.0110425087540463,-0.0361399026915109,
-0.0126824517504928));
#29669=CARTESIAN_POINT('Ctrl Pts',(-0.0110362871562949,-0.0361408966748177,
-0.0126642256829963));
#29670=CARTESIAN_POINT('Ctrl Pts',(-0.0110329445342361,-0.0361414509341665,
-0.0126540908207389));
#29671=CARTESIAN_POINT('Ctrl Pts',(-0.011023254600046,-0.0361431204423895,
-0.0126236529164242));
#29672=CARTESIAN_POINT('Ctrl Pts',(-0.0110172219038535,-0.0361442458995248,
-0.0126032530308853));
#29673=CARTESIAN_POINT('Ctrl Pts',(-0.0109903594074654,-0.0361496999765438,
-0.0125049892653878));
#29674=CARTESIAN_POINT('Ctrl Pts',(-0.0109752325960801,-0.0361542079032663,
-0.0124257067467117));
#29675=CARTESIAN_POINT('Ctrl Pts',(-0.010956872869965,-0.0361637402501552,
-0.0122598437510436));
#29676=CARTESIAN_POINT('Ctrl Pts',(-0.0109545906758734,-0.0361687620808592,
-0.012173428538151));
#29677=CARTESIAN_POINT('Ctrl Pts',(-0.0109616935662868,-0.0361757171680143,
-0.0120499020085666));
#29678=CARTESIAN_POINT('Ctrl Pts',(-0.0109652021514898,-0.0361777853871252,
-0.0120126161084856));
#29679=CARTESIAN_POINT('Ctrl Pts',(-0.0109712850658341,-0.036180293065164,
-0.0119661675885122));
#29680=CARTESIAN_POINT('Ctrl Pts',(-0.0109725914901125,-0.0361807923935559,
-0.0119568539841126));
#29681=CARTESIAN_POINT('Ctrl Pts',(-0.0109747873383674,-0.0361815731404391,
-0.0119421763981681));
#29682=CARTESIAN_POINT('Ctrl Pts',(-0.0109756200786809,-0.0361818575921791,
-0.0119368043195178));
#29683=CARTESIAN_POINT('Ctrl Pts',(-0.0109772496437129,-0.0361823928124027,
-0.0119266467736726));
#29684=CARTESIAN_POINT('Ctrl Pts',(-0.0109780406434466,-0.0361826438783202,
-0.0119218606663769));
#29685=CARTESIAN_POINT('Ctrl Pts',(-0.0109799727951164,-0.0361832370917533,
-0.0119105029883949));
#29686=CARTESIAN_POINT('Ctrl Pts',(-0.0109811339975104,-0.0361835781021954,
-0.0119039350010676));
#29687=CARTESIAN_POINT('Ctrl Pts',(-0.0109852226464653,-0.036184728706596,
-0.011881652546014));
#29688=CARTESIAN_POINT('Ctrl Pts',(-0.0109883517628177,-0.0361855275504684,
-0.0118659756468744));
#29689=CARTESIAN_POINT('Ctrl Pts',(-0.0109966474911758,-0.0361874661730907,
-0.0118275359933416));
#29690=CARTESIAN_POINT('Ctrl Pts',(-0.0110020881238203,-0.0361885935066934,
-0.0118048360314069));
#29691=CARTESIAN_POINT('Ctrl Pts',(-0.0110277809518416,-0.0361933875263122,
-0.0117074427553644));
#29692=CARTESIAN_POINT('Ctrl Pts',(-0.0110531220492531,-0.0361968875931943,
-0.0116342049881169));
#29693=CARTESIAN_POINT('Ctrl Pts',(-0.0111207497586246,-0.0362046666688781,
-0.0114778900941258));
#29694=CARTESIAN_POINT('Ctrl Pts',(-0.011165273332873,-0.0362089525329183,
-0.0113961183978989));
#29695=CARTESIAN_POINT('Ctrl Pts',(-0.0112290480928655,-0.0362145792624668,
-0.0113006330997497));
#29696=CARTESIAN_POINT('Ctrl Pts',(-0.0112416044612554,-0.0362156663512808,
-0.0112826737228367));
#29697=CARTESIAN_POINT('Ctrl Pts',(-0.011260875188243,-0.0362173078300366,
-0.0112563241015212));
#29698=CARTESIAN_POINT('Ctrl Pts',(-0.0112673018895231,-0.0362178510364836,
-0.0112477263652471));
#29699=CARTESIAN_POINT('Ctrl Pts',(-0.0112789882452256,-0.0362188316703332,
-0.0112324276951326));
#29700=CARTESIAN_POINT('Ctrl Pts',(-0.0112842147079078,-0.0362192677649649,
-0.0112257018925722));
#29701=CARTESIAN_POINT('Ctrl Pts',(-0.0112954697055776,-0.0362202018240542,
-0.0112114630370418));
#29702=CARTESIAN_POINT('Ctrl Pts',(-0.0113015134252252,-0.0362207003944266,
-0.0112039624964365));
#29703=CARTESIAN_POINT('Ctrl Pts',(-0.0113181050903677,-0.0362220612798321,
-0.0111837615714883));
#29704=CARTESIAN_POINT('Ctrl Pts',(-0.0113287870721487,-0.0362229290765472,
-0.0111711733388549));
#29705=CARTESIAN_POINT('Ctrl Pts',(-0.0113949512804052,-0.0362282558166161,
-0.0110956912317522));
#29706=CARTESIAN_POINT('Ctrl Pts',(-0.0114552760775991,-0.0362329222290524,
-0.011037243908343));
#29707=CARTESIAN_POINT('Ctrl Pts',(-0.0115615607828297,-0.0362407695512787,
-0.0109498557629705));
#29708=CARTESIAN_POINT('Ctrl Pts',(-0.0116048339847863,-0.0362438741970801,
-0.0109179122296245));
#29709=CARTESIAN_POINT('Ctrl Pts',(-0.0117101602480476,-0.036251124689397,
-0.0108483539185482));
#29710=CARTESIAN_POINT('Ctrl Pts',(-0.011773380539475,-0.0362552491934912,
-0.0108127217884991));
#29711=CARTESIAN_POINT('Ctrl Pts',(-0.0118482771097153,-0.0362597030087172,
-0.0107772058977001));
#29712=CARTESIAN_POINT('Ctrl Pts',(-0.0118577228629406,-0.0362602571113017,
-0.0107728431886333));
#29713=CARTESIAN_POINT('Ctrl Pts',(-0.0118724056986486,-0.0362611058785067,
-0.010766240993051));
#29714=CARTESIAN_POINT('Ctrl Pts',(-0.0118776120989624,-0.0362614044250356,
-0.0107639344759347));
#29715=CARTESIAN_POINT('Ctrl Pts',(-0.0118872463652017,-0.0362619522534782,
-0.0107597299907103));
#29716=CARTESIAN_POINT('Ctrl Pts',(-0.0118916703675122,-0.0362622020076609,
-0.0107578239269718));
#29717=CARTESIAN_POINT('Ctrl Pts',(-0.0119018501396967,-0.0362627726519869,
-0.0107534944206526));
#29718=CARTESIAN_POINT('Ctrl Pts',(-0.01190761176663,-0.0362630926873127,
-0.0107510851712563));
#29719=CARTESIAN_POINT('Ctrl Pts',(-0.0119257375343961,-0.0362640907588852,
-0.0107436347626959));
#29720=CARTESIAN_POINT('Ctrl Pts',(-0.011938152874298,-0.0362647616911954,
-0.010738718947152));
#29721=CARTESIAN_POINT('Ctrl Pts',(-0.0120034351687105,-0.0362682310749773,
-0.0107138459573434));
#29722=CARTESIAN_POINT('Ctrl Pts',(-0.0120573094421694,-0.0362708957164369,
-0.0106966412695876));
#29723=CARTESIAN_POINT('Ctrl Pts',(-0.0122073705300166,-0.036278072884494,
-0.0106576555457311));
#29724=CARTESIAN_POINT('Ctrl Pts',(-0.0123048831318662,-0.0362824830479426,
-0.0106420716389651));
#29725=CARTESIAN_POINT('Ctrl Pts',(-0.0124570484530169,-0.0362896466107501,
-0.0106325083995513));
#29726=CARTESIAN_POINT('Ctrl Pts',(-0.0125110161422331,-0.0362922379838347,
-0.010631950376522));
#29727=CARTESIAN_POINT('Ctrl Pts',(-0.0125803369323508,-0.0362956848547156,
-0.0106348686282824));
#29728=CARTESIAN_POINT('Ctrl Pts',(-0.0125957634583471,-0.036296459329547,
-0.010635750342602));
#29729=CARTESIAN_POINT('Ctrl Pts',(-0.0126206305493715,-0.0362977207308511,
-0.010637546695755));
#29730=CARTESIAN_POINT('Ctrl Pts',(-0.0126300806566654,-0.0362982031216088,
-0.0106383169734026));
#29731=CARTESIAN_POINT('Ctrl Pts',(-0.0126481729081534,-0.0362991326803021,
-0.0106399596612617));
#29732=CARTESIAN_POINT('Ctrl Pts',(-0.0126568159794567,-0.036299579390021,
-0.0106408180480625));
#29733=CARTESIAN_POINT('Ctrl Pts',(-0.012676762745127,-0.0363006165826884,
-0.0106429692822722));
#29734=CARTESIAN_POINT('Ctrl Pts',(-0.0126880602121421,-0.0363012086857701,
-0.0106443142612758));
#29735=CARTESIAN_POINT('Ctrl Pts',(-0.0127240947681315,-0.0363031125234025,
-0.0106490089410044));
#29736=CARTESIAN_POINT('Ctrl Pts',(-0.0127487650067397,-0.0363044390462012,
-0.0106528339187856));
#29737=CARTESIAN_POINT('Ctrl Pts',(-0.0128560992610033,-0.0363103133987427,
-0.0106721528892649));
#29738=CARTESIAN_POINT('Ctrl Pts',(-0.0129375016848264,-0.0363150478948562,
-0.0106937902533563));
#29739=CARTESIAN_POINT('Ctrl Pts',(-0.0131133414203478,-0.0363257331868827,
-0.0107562848289119));
#29740=CARTESIAN_POINT('Ctrl Pts',(-0.0132062956559183,-0.0363317003266798,
-0.0108001677884493));
#29741=CARTESIAN_POINT('Ctrl Pts',(-0.0133079152805953,-0.0363381526332863,
-0.0108611756241289));
#29742=CARTESIAN_POINT('Ctrl Pts',(-0.0133214903328683,-0.0363390125569821,
-0.0108696151274333));
#29743=CARTESIAN_POINT('Ctrl Pts',(-0.0133402175855677,-0.0363401933428642,
-0.0108816651593054));
#29744=CARTESIAN_POINT('Ctrl Pts',(-0.0133454821363869,-0.0363405246638285,
-0.0108850982906306));
#29745=CARTESIAN_POINT('Ctrl Pts',(-0.0133549177036505,-0.0363411171537095,
-0.0108913339335234));
#29746=CARTESIAN_POINT('Ctrl Pts',(-0.0133590962612432,-0.0363413790577134,
-0.0108941248188989));
#29747=CARTESIAN_POINT('Ctrl Pts',(-0.0133676818595878,-0.0363419161088174,
-0.0108999200454453));
#29748=CARTESIAN_POINT('Ctrl Pts',(-0.0133720870231281,-0.0363421910941396,
-0.010902926866466));
#29749=CARTESIAN_POINT('Ctrl Pts',(-0.0133834704633554,-0.0363429004487006,
-0.0109107836614822));
#29750=CARTESIAN_POINT('Ctrl Pts',(-0.0133904245067542,-0.0363433325704652,
-0.0109156686096983));
#29751=CARTESIAN_POINT('Ctrl Pts',(-0.0134209629100696,-0.0363452264748472,
-0.0109374996669656));
#29752=CARTESIAN_POINT('Ctrl Pts',(-0.013444107697458,-0.0363466519362665,
-0.0109550530511747));
#29753=CARTESIAN_POINT('Ctrl Pts',(-0.0135104271492173,-0.0363507502054419,
-0.0110083657052845));
#29754=CARTESIAN_POINT('Ctrl Pts',(-0.0135521665369769,-0.0363533483823784,
-0.0110458371295945));
#29755=CARTESIAN_POINT('Ctrl Pts',(-0.0136737002918405,-0.0363612738800246,
-0.0111675293003274));
#29756=CARTESIAN_POINT('Ctrl Pts',(-0.0137461116636287,-0.0363665559123479,
-0.0112585237994112));
#29757=CARTESIAN_POINT('Ctrl Pts',(-0.0138174488374334,-0.0363731688119264,
-0.0113724117269202));
#29758=CARTESIAN_POINT('Ctrl Pts',(-0.0138269664372651,-0.0363740864268147,
-0.0113882303957387));
#29759=CARTESIAN_POINT('Ctrl Pts',(-0.0138418413518704,-0.0363755811969191,
-0.011413988374745));
#29760=CARTESIAN_POINT('Ctrl Pts',(-0.0138473775129398,-0.036376152018528,
-0.0114238225780818));
#29761=CARTESIAN_POINT('Ctrl Pts',(-0.0138570156772217,-0.0363771724288197,
-0.0114413915201597));
#29762=CARTESIAN_POINT('Ctrl Pts',(-0.013861160693953,-0.0363776204767645,
-0.0114491021629619));
#29763=CARTESIAN_POINT('Ctrl Pts',(-0.0138697595828043,-0.0363785698534938,
-0.0114654296343553));
#29764=CARTESIAN_POINT('Ctrl Pts',(-0.0138741982534943,-0.0363790716882443,
-0.0114740540027902));
#29765=CARTESIAN_POINT('Ctrl Pts',(-0.0138858107905818,-0.0363804167990027,
-0.0114971498678827));
#29766=CARTESIAN_POINT('Ctrl Pts',(-0.0138928391087077,-0.0363812650498414,
-0.0115116928627213));
#29767=CARTESIAN_POINT('Ctrl Pts',(-0.013929096430443,-0.0363858303468814,
-0.0115898242272903));
#29768=CARTESIAN_POINT('Ctrl Pts',(-0.0139541988972364,-0.0363896858341416,
-0.0116552284130325));
#29769=CARTESIAN_POINT('Ctrl Pts',(-0.0140028366343276,-0.0363990330694428,
-0.0118133106121293));
#29770=CARTESIAN_POINT('Ctrl Pts',(-0.0140223757454965,-0.0364045969860129,
-0.0119069184214881));
#29771=CARTESIAN_POINT('Ctrl Pts',(-0.0140380045422238,-0.0364124568433655,
-0.0120445276131966));
#29772=CARTESIAN_POINT('Ctrl Pts',(-0.0140410714644329,-0.036414864931502,
-0.0120875148762122));
#29773=CARTESIAN_POINT('Ctrl Pts',(-0.0140426067239643,-0.0364176950862156,
-0.0121398133030783));
#29774=CARTESIAN_POINT('Ctrl Pts',(-0.0140427948970806,-0.0364181912692948,
-0.0121490521962625));
#29775=CARTESIAN_POINT('Ctrl Pts',(-0.014042966764963,-0.0364189954516571,
-0.0121641525360454));
#29776=CARTESIAN_POINT('Ctrl Pts',(-0.0140430000775132,-0.0364193058872427,
-0.0121700130663469));
#29777=CARTESIAN_POINT('Ctrl Pts',(-0.0140429999998646,-0.0364196145604726,
-0.0121758737299574));
#29778=CARTESIAN_POINT('Ctrl Pts',(-0.0133928340876084,-0.0365776381485745,
-0.0112832194050649));
#29779=CARTESIAN_POINT('Ctrl Pts',(-0.0130952609160143,-0.0365511095967742,
-0.0109855742143942));
#29780=CARTESIAN_POINT('Ctrl Pts',(-0.0121841523466751,-0.0364980554675351,
-0.010716645344559));
#29781=CARTESIAN_POINT('Ctrl Pts',(-0.0110992562595946,-0.036418475760857,
-0.0116550159846514));
#29782=CARTESIAN_POINT('Ctrl Pts',(-0.0113060193050241,-0.0363388990285403,
-0.013072272818964));
#29783=CARTESIAN_POINT('Ctrl Pts',(-0.0126086058506385,-0.0362593222962236,
-0.0136653243656934));
#29784=CARTESIAN_POINT('Ctrl Pts',(-0.0138123222557375,-0.0361797455639069,
-0.0128890170219797));
#29785=CARTESIAN_POINT('Ctrl Pts',(-0.0138090066083574,-0.0361001688315902,
-0.0114570252002803));
#29786=CARTESIAN_POINT('Ctrl Pts',(-0.0126024821547228,-0.0360205920992735,
-0.0106859178189944));
#29787=CARTESIAN_POINT('Ctrl Pts',(-0.0113015994342994,-0.0359410153669568,
-0.0112846225371221));
#29788=CARTESIAN_POINT('Ctrl Pts',(-0.0111025739600164,-0.0358614386346401,
-0.0127027090585796));
#29789=CARTESIAN_POINT('Ctrl Pts',(-0.0121882761682891,-0.0357818619023234,
-0.0136364138535612));
#29790=CARTESIAN_POINT('Ctrl Pts',(-0.0135605905087235,-0.0357022851700067,
-0.0132273094558074));
#29791=CARTESIAN_POINT('Ctrl Pts',(-0.0139578092204135,-0.03562270843769,
-0.0118515172183842));
#29792=CARTESIAN_POINT('Ctrl Pts',(-0.0130147529561138,-0.0355431317053733,
-0.0107739131649265));
#29793=CARTESIAN_POINT('Ctrl Pts',(-0.0115984404799773,-0.0354635549730566,
-0.0109852243885246));
#29794=CARTESIAN_POINT('Ctrl Pts',(-0.0110110050149965,-0.0353839782407399,
-0.0122911757623016));
#29795=CARTESIAN_POINT('Ctrl Pts',(-0.0117925206434878,-0.0353044015084232,
-0.0134911019626899));
#29796=CARTESIAN_POINT('Ctrl Pts',(-0.0132244788603522,-0.0352248247761065,
-0.0134818151702574));
#29797=CARTESIAN_POINT('Ctrl Pts',(-0.0139903656765037,-0.0351452480437898,
-0.0122718534549942));
#29798=CARTESIAN_POINT('Ctrl Pts',(-0.0133860405686823,-0.0350656713114731,
-0.0109736311318028));
#29799=CARTESIAN_POINT('Ctrl Pts',(-0.0119671076448217,-0.0349860945791564,
-0.0107807075166315));
#29800=CARTESIAN_POINT('Ctrl Pts',(-0.0110381051925874,-0.0349065178468397,
-0.0118704526781616));
#29801=CARTESIAN_POINT('Ctrl Pts',(-0.0114531392148339,-0.034826941114523,
-0.0132409769756585));
#29802=CARTESIAN_POINT('Ctrl Pts',(-0.0128306358568174,-0.0347473643822063,
-0.0136322481173509));
#29803=CARTESIAN_POINT('Ctrl Pts',(-0.0139041525817756,-0.0346677876498896,
-0.0126845393365732));
#29804=CARTESIAN_POINT('Ctrl Pts',(-0.0136867198526057,-0.0345882109175729,
-0.0112691548999602));
#29805=CARTESIAN_POINT('Ctrl Pts',(-0.0123782409152947,-0.0345086341852562,
-0.0106873706036063));
#29806=CARTESIAN_POINT('Ctrl Pts',(-0.0111817048159939,-0.0344290574529395,
-0.0114740671512591));
#29807=CARTESIAN_POINT('Ctrl Pts',(-0.0111971826193403,-0.0343494807206229,
-0.0129059716638541));
#29808=CARTESIAN_POINT('Ctrl Pts',(-0.0124104443467463,-0.0342699039883061,
-0.0136666201218039));
#29809=CARTESIAN_POINT('Ctrl Pts',(-0.0137060417285948,-0.0341903272559894,
-0.013056687732387));
#29810=CARTESIAN_POINT('Ctrl Pts',(-0.013892828761843,-0.0341107505236727,
-0.0116369339861979));
#29811=CARTESIAN_POINT('Ctrl Pts',(-0.0127990772296097,-0.034031173791356,
-0.0107126517341985));
#29812=CARTESIAN_POINT('Ctrl Pts',(-0.0114303601473809,-0.0339515970590393,
-0.0111336073665443));
#29813=CARTESIAN_POINT('Ctrl Pts',(-0.0110450482905081,-0.0338720203267226,
-0.0125127827972119));
#29814=CARTESIAN_POINT('Ctrl Pts',(-0.011997389579471,-0.0337924435944059,
-0.0135821920570098));
#29815=CARTESIAN_POINT('Ctrl Pts',(-0.0134118207135884,-0.0337128668620893,
-0.0133586419229471));
#29816=CARTESIAN_POINT('Ctrl Pts',(-0.0139879423436801,-0.0336332901297725,
-0.0120476598624509));
#29817=CARTESIAN_POINT('Ctrl Pts',(-0.0131960799067701,-0.0335537133974558,
-0.0108545362407697));
#29818=CARTESIAN_POINT('Ctrl Pts',(-0.011764255695894,-0.0334741366651392,
-0.0108762047605805));
#29819=CARTESIAN_POINT('Ctrl Pts',(-0.0110088599028788,-0.0333945599328224,
-0.012092743823454));
#29820=CARTESIAN_POINT('Ctrl Pts',(-0.0116243881266391,-0.0333149832005057,
-0.0133856920441328));
#29821=CARTESIAN_POINT('Ctrl Pts',(-0.0130449361797783,-0.0332354064681891,
-0.0135663390045967));
#29822=CARTESIAN_POINT('Ctrl Pts',(-0.0139644809416035,-0.0331558297358723,
-0.0124686015466394));
#29823=CARTESIAN_POINT('Ctrl Pts',(-0.0135376115745145,-0.0330762530035557,
-0.011101717265128));
#29824=CARTESIAN_POINT('Ctrl Pts',(-0.012156783132532,-0.0329966762712389,
-0.0107223718955571));
#29825=CARTESIAN_POINT('Ctrl Pts',(-0.0110915013299854,-0.0329170995389223,
-0.0116793278907656));
#29826=CARTESIAN_POINT('Ctrl Pts',(-0.0113211646892293,-0.0328375228066056,
-0.0130927792825796));
#29827=CARTESIAN_POINT('Ctrl Pts',(-0.01263462536737,-0.0327579460742888,
-0.0136632274770574));
#29828=CARTESIAN_POINT('Ctrl Pts',(-0.0138243142082752,-0.0326783693419721,
-0.012866213953063));
#29829=CARTESIAN_POINT('Ctrl Pts',(-0.0137964553771785,-0.0325987926096555,
-0.0114344968088202));
#29830=CARTESIAN_POINT('Ctrl Pts',(-0.0125766617193749,-0.0325192158773387,
-0.0106843678012449));
#29831=CARTESIAN_POINT('Ctrl Pts',(-0.0112863868288221,-0.032439639145022,
-0.0113054803533772));
#29832=CARTESIAN_POINT('Ctrl Pts',(-0.0111118833179225,-0.0323600624127054,
-0.0127267961593106));
#29833=CARTESIAN_POINT('Ctrl Pts',(-0.0122135861817712,-0.0322804856803887,
-0.0136415862420932));
#29834=CARTESIAN_POINT('Ctrl Pts',(-0.0135786121115237,-0.032200908948072,
-0.0132088111195533));
#29835=CARTESIAN_POINT('Ctrl Pts',(-0.0139519839028259,-0.0321213322157552,
-0.0118263554781389));
#29836=CARTESIAN_POINT('Ctrl Pts',(-0.0129904310894627,-0.0320417554834385,
-0.0107652210455696));
#29837=CARTESIAN_POINT('Ctrl Pts',(-0.0115779858617312,-0.0319621787511219,
-0.01100099333779));
#29838=CARTESIAN_POINT('Ctrl Pts',(-0.0110132217655809,-0.0318826020188051,
-0.0123169080795676));
#29839=CARTESIAN_POINT('Ctrl Pts',(-0.0118153714793421,-0.0318030252864884,
-0.0135031399041744));
#29840=CARTESIAN_POINT('Ctrl Pts',(-0.0132469547918328,-0.0317234485541717,
-0.0134690912764528));
#29841=CARTESIAN_POINT('Ctrl Pts',(-0.0139918029961525,-0.0316438718218551,
-0.0122460658368738));
#29842=CARTESIAN_POINT('Ctrl Pts',(-0.0133651177178693,-0.0315642950895384,
-0.0109584883729171));
#29843=CARTESIAN_POINT('Ctrl Pts',(-0.0119430607432697,-0.0314847183572217,
-0.0107901316166862));
#29844=CARTESIAN_POINT('Ctrl Pts',(-0.011033042409537,-0.0314051416249049,
-0.0118957792096504));
#29845=CARTESIAN_POINT('Ctrl Pts',(-0.0114717152553868,-0.0313255648925883,
-0.0132589214302837));
#29846=CARTESIAN_POINT('Ctrl Pts',(-0.0128557721434822,-0.0312459881602716,
-0.0136263123589553));
#29847=CARTESIAN_POINT('Ctrl Pts',(-0.0139127395828671,-0.0311664114279549,
-0.0126601812869636));
#29848=CARTESIAN_POINT('Ctrl Pts',(-0.013670862357182,-0.0310868346956382,
-0.0112487675025001));
#29849=CARTESIAN_POINT('Ctrl Pts',(-0.0123525189326018,-0.0310072579633215,
-0.0106897002180619));
#29850=CARTESIAN_POINT('Ctrl Pts',(-0.0111697647962804,-0.0309276812310048,
-0.011496966988396));
#29851=CARTESIAN_POINT('Ctrl Pts',(-0.0112100054671832,-0.0308481044986881,
-0.0129283976523225));
#29852=CARTESIAN_POINT('Ctrl Pts',(-0.0124362342931823,-0.0307685277663714,
-0.0136679358835917));
#29853=CARTESIAN_POINT('Ctrl Pts',(-0.0137211008826827,-0.0306889510340547,
-0.013035718856821));
#29854=CARTESIAN_POINT('Ctrl Pts',(-0.0138832873524999,-0.030609374301738,
-0.0116128911297885));
#29855=CARTESIAN_POINT('Ctrl Pts',(-0.01277375482353,-0.0305297975694213,
-0.0107077693601632));
#29856=CARTESIAN_POINT('Ctrl Pts',(-0.0114124466955457,-0.0304502208371046,
-0.0111521247940392));
#29857=CARTESIAN_POINT('Ctrl Pts',(-0.011051187659041,-0.0303706441047879,
-0.0125381544417569));
#29858=CARTESIAN_POINT('Ctrl Pts',(-0.0120216020104472,-0.0302910673724712,
-0.0135901705217094));
#29859=CARTESIAN_POINT('Ctrl Pts',(-0.0134324915261294,-0.0302114906401545,
-0.0133436777917981));
#29860=CARTESIAN_POINT('Ctrl Pts',(-0.0139848228738421,-0.0301319118250522,
-0.0120198866613579));
#29861=CARTESIAN_POINT('Ctrl Pts',(-0.013444661127689,-0.0300788585873889,
-0.011238463163598));
#29862=CARTESIAN_POINT('Ctrl Pts',(-0.0130689497297049,-0.0300523309271644,
-0.0110488021962071));
#29863=CARTESIAN_POINT('Ctrl Pts',(-0.0134596600795358,-0.0366321952253369,
-0.0112164083979732));
#29864=CARTESIAN_POINT('Ctrl Pts',(-0.0131398144357782,-0.0366056666735365,
-0.0108964853447243));
#29865=CARTESIAN_POINT('Ctrl Pts',(-0.0121605120835799,-0.0365526125442975,
-0.0106074279440297));
#29866=CARTESIAN_POINT('Ctrl Pts',(-0.0109944147317139,-0.0364730328376194,
-0.011616032852381));
#29867=CARTESIAN_POINT('Ctrl Pts',(-0.0112166533798299,-0.0363934561053027,
-0.0131393671708349));
#29868=CARTESIAN_POINT('Ctrl Pts',(-0.0126167346774819,-0.036313879372986,
-0.013776806872569));
#29869=CARTESIAN_POINT('Ctrl Pts',(-0.0139105456968955,-0.0362343026406694,
-0.0129423952192144));
#29870=CARTESIAN_POINT('Ctrl Pts',(-0.0139069818831113,-0.0361547259083527,
-0.0114032230431297));
#29871=CARTESIAN_POINT('Ctrl Pts',(-0.0126101526410306,-0.0360751491760359,
-0.010574400554018));
#29872=CARTESIAN_POINT('Ctrl Pts',(-0.0112119026948481,-0.0359955724437193,
-0.0112179165503167));
#29873=CARTESIAN_POINT('Ctrl Pts',(-0.0109979807522041,-0.0359159957114026,
-0.0127421426555453));
#29874=CARTESIAN_POINT('Ctrl Pts',(-0.0121649445610503,-0.0358364189790859,
-0.0137457324940732));
#29875=CARTESIAN_POINT('Ctrl Pts',(-0.0136399725728248,-0.0357568422467691,
-0.0133060078416033));
#29876=CARTESIAN_POINT('Ctrl Pts',(-0.0140669219307673,-0.0356772655144525,
-0.0118272416225322));
#29877=CARTESIAN_POINT('Ctrl Pts',(-0.0130532806930891,-0.0355976887821358,
-0.010668982091448));
#29878=CARTESIAN_POINT('Ctrl Pts',(-0.0115309614152291,-0.0355181120498191,
-0.0108961093354223));
#29879=CARTESIAN_POINT('Ctrl Pts',(-0.0108995581423592,-0.0354385353175024,
-0.0122998073086775));
#29880=CARTESIAN_POINT('Ctrl Pts',(-0.0117395679052095,-0.0353589585851857,
-0.013589544437763));
#29881=CARTESIAN_POINT('Ctrl Pts',(-0.0132787039612366,-0.035279381852869,
-0.0135795625563719));
#29882=CARTESIAN_POINT('Ctrl Pts',(-0.0141019151413475,-0.0351998051205523,
-0.0122790387837916));
#29883=CARTESIAN_POINT('Ctrl Pts',(-0.0134523580858022,-0.0351202283882355,
-0.0108836483577088));
#29884=CARTESIAN_POINT('Ctrl Pts',(-0.011927222227453,-0.0350406516559189,
-0.0106762849802916));
#29885=CARTESIAN_POINT('Ctrl Pts',(-0.0109286866881252,-0.0349610749236022,
-0.0118475943454942));
#29886=CARTESIAN_POINT('Ctrl Pts',(-0.0113747847799511,-0.0348814981912855,
-0.0133206983349094));
#29887=CARTESIAN_POINT('Ctrl Pts',(-0.0128553829732249,-0.0348019214589688,
-0.013741254964823));
#29888=CARTESIAN_POINT('Ctrl Pts',(-0.0140092492513551,-0.0347223447266521,
-0.0127226129835629));
#29889=CARTESIAN_POINT('Ctrl Pts',(-0.0137755423252142,-0.0346427679943354,
-0.0112012912062412));
#29890=CARTESIAN_POINT('Ctrl Pts',(-0.012369127607767,-0.0345631912620187,
-0.0105759620752631));
#29891=CARTESIAN_POINT('Ctrl Pts',(-0.0110830343188129,-0.034483614529702,
-0.0114215405337574));
#29892=CARTESIAN_POINT('Ctrl Pts',(-0.0110996705899822,-0.0344040377973853,
-0.0129606188659093));
#29893=CARTESIAN_POINT('Ctrl Pts',(-0.0124037413708582,-0.0343244610650686,
-0.0137781996121936));
#29894=CARTESIAN_POINT('Ctrl Pts',(-0.0137963103864987,-0.0342448843327519,
-0.0131226155866023));
#29895=CARTESIAN_POINT('Ctrl Pts',(-0.0139970778769776,-0.0341653076004352,
-0.0115965974698001));
#29896=CARTESIAN_POINT('Ctrl Pts',(-0.0128214622760691,-0.0340857308681185,
-0.0106031354237402));
#29897=CARTESIAN_POINT('Ctrl Pts',(-0.011350300766642,-0.0340061541358018,
-0.0110555983406749));
#29898=CARTESIAN_POINT('Ctrl Pts',(-0.010936149456399,-0.0339265774034851,
-0.0125380009750028));
#29899=CARTESIAN_POINT('Ctrl Pts',(-0.0119597706753867,-0.0338470006711684,
-0.0136874523563485));
#29900=CARTESIAN_POINT('Ctrl Pts',(-0.0134800677983394,-0.0337674239388517,
-0.0134471701556437));
#29901=CARTESIAN_POINT('Ctrl Pts',(-0.0140993104292263,-0.033687847206535,
-0.0120380649636411));
#29902=CARTESIAN_POINT('Ctrl Pts',(-0.0132481794299362,-0.0336082704742183,
-0.010755639566168));
#29903=CARTESIAN_POINT('Ctrl Pts',(-0.0117091874098493,-0.0335286937419016,
-0.0107789299106268));
#29904=CARTESIAN_POINT('Ctrl Pts',(-0.0108972524749411,-0.0334491170095849,
-0.0120865233258413));
#29905=CARTESIAN_POINT('Ctrl Pts',(-0.0115588511665332,-0.0333695402772682,
-0.0134762448984304));
#29906=CARTESIAN_POINT('Ctrl Pts',(-0.0130857230418127,-0.0332899635449515,
-0.0136704127498293));
#29907=CARTESIAN_POINT('Ctrl Pts',(-0.0140740930105643,-0.0332103868126348,
-0.0124905128884402));
#29908=CARTESIAN_POINT('Ctrl Pts',(-0.0136152737333239,-0.0331308100803181,
-0.011021321359446));
#29909=CARTESIAN_POINT('Ctrl Pts',(-0.0121310943646713,-0.0330512333480014,
-0.0106135831104403));
#29910=CARTESIAN_POINT('Ctrl Pts',(-0.0109860793685498,-0.0329716566156847,
-0.0116421644327933));
#29911=CARTESIAN_POINT('Ctrl Pts',(-0.0112329323512678,-0.032892079883368,
-0.0131614084826278));
#29912=CARTESIAN_POINT('Ctrl Pts',(-0.012644701678118,-0.0328125031510513,
-0.0137745530380177));
#29913=CARTESIAN_POINT('Ctrl Pts',(-0.0139234352116284,-0.0327329264187346,
-0.0129178854080032));
#29914=CARTESIAN_POINT('Ctrl Pts',(-0.0138934912293844,-0.0326533496864179,
-0.0113790084681708));
#29915=CARTESIAN_POINT('Ctrl Pts',(-0.0125823996224312,-0.0325737729541012,
-0.0105727345220222));
#29916=CARTESIAN_POINT('Ctrl Pts',(-0.0111955514708247,-0.0324941962217845,
-0.0112403355124556));
#29917=CARTESIAN_POINT('Ctrl Pts',(-0.0110079868880278,-0.0324146194894678,
-0.0127680326045561));
#29918=CARTESIAN_POINT('Ctrl Pts',(-0.0121921489542162,-0.0323350427571511,
-0.0137512920205955));
#29919=CARTESIAN_POINT('Ctrl Pts',(-0.0136593430393164,-0.0322554660248344,
-0.013286124959568));
#29920=CARTESIAN_POINT('Ctrl Pts',(-0.01406066060538,-0.0321758892925177,
-0.0118001966004165));
#29921=CARTESIAN_POINT('Ctrl Pts',(-0.0130271384066231,-0.0320963125602011,
-0.0106596393926541));
#29922=CARTESIAN_POINT('Ctrl Pts',(-0.0115089758292782,-0.0320167358278843,
-0.0109130585439219));
#29923=CARTESIAN_POINT('Ctrl Pts',(-0.0109019408101714,-0.0319371590955676,
-0.0123274656138171));
#29924=CARTESIAN_POINT('Ctrl Pts',(-0.0117641290585723,-0.0318575823632509,
-0.0136024833835792));
#29925=CARTESIAN_POINT('Ctrl Pts',(-0.0133028621497417,-0.0317780056309342,
-0.0135658863167324));
#29926=CARTESIAN_POINT('Ctrl Pts',(-0.0141034600401229,-0.0316984288986175,
-0.0122513210386921));
#29927=CARTESIAN_POINT('Ctrl Pts',(-0.0134298692214611,-0.0316188521663008,
-0.0108673722080879));
#29928=CARTESIAN_POINT('Ctrl Pts',(-0.0119013754864109,-0.0315392754339842,
-0.0106864144463745));
#29929=CARTESIAN_POINT('Ctrl Pts',(-0.0109232449707309,-0.0314596987016675,
-0.0118748164929907));
#29930=CARTESIAN_POINT('Ctrl Pts',(-0.0113947511822221,-0.0313801219693508,
-0.0133399858789131));
#29931=CARTESIAN_POINT('Ctrl Pts',(-0.0128824006366349,-0.031300545237034,
-0.0137348749324596));
#29932=CARTESIAN_POINT('Ctrl Pts',(-0.0140184789640921,-0.0312209685047174,
-0.0126964318059509));
#29933=CARTESIAN_POINT('Ctrl Pts',(-0.0137584979431382,-0.0311413917724006,
-0.0111793778723534));
#29934=CARTESIAN_POINT('Ctrl Pts',(-0.0123414804107126,-0.031061815040084,
-0.0105784660544736));
#29935=CARTESIAN_POINT('Ctrl Pts',(-0.0110702006239228,-0.0309822383077672,
-0.0114461543560042));
#29936=CARTESIAN_POINT('Ctrl Pts',(-0.0111134531900773,-0.0309026615754506,
-0.0129847233733154));
#29937=CARTESIAN_POINT('Ctrl Pts',(-0.0124314616185408,-0.0308230848431338,
-0.0137796138548614));
#29938=CARTESIAN_POINT('Ctrl Pts',(-0.0138124966737499,-0.0307435081108172,
-0.0131000772526917));
#29939=CARTESIAN_POINT('Ctrl Pts',(-0.013986822321353,-0.0306639313785005,
-0.0115707550766674));
#29940=CARTESIAN_POINT('Ctrl Pts',(-0.0127942445627561,-0.0305843546461837,
-0.0105978876184423));
#29941=CARTESIAN_POINT('Ctrl Pts',(-0.0113310465458955,-0.0305047779138671,
-0.011075501742874));
#29942=CARTESIAN_POINT('Ctrl Pts',(-0.0109427483385165,-0.0304252011815503,
-0.0125652716121345));
#29943=CARTESIAN_POINT('Ctrl Pts',(-0.0119857953352411,-0.0303456244492337,
-0.0136960279855438));
#29944=CARTESIAN_POINT('Ctrl Pts',(-0.013502285760089,-0.0302660477169169,
-0.0134310860035175));
#29945=CARTESIAN_POINT('Ctrl Pts',(-0.014095957476293,-0.0301864689018147,
-0.0120082130205535));
#29946=CARTESIAN_POINT('Ctrl Pts',(-0.0135153662203476,-0.0301334156641513,
-0.0111683022841477));
#29947=CARTESIAN_POINT('Ctrl Pts',(-0.0131115339349587,-0.0301068880039268,
-0.0109644457540518));
#29948=CARTESIAN_POINT('Ctrl Pts',(-0.0135264860714633,-0.0366867523020992,
-0.0111495973908816));
#29949=CARTESIAN_POINT('Ctrl Pts',(-0.0131843679555423,-0.0366602237502991,
-0.0108073964750543));
#29950=CARTESIAN_POINT('Ctrl Pts',(-0.0121368718204848,-0.0366071696210597,
-0.0104982105435003));
#29951=CARTESIAN_POINT('Ctrl Pts',(-0.0108895732038333,-0.0365275899143818,
-0.0115770497201106));
#29952=CARTESIAN_POINT('Ctrl Pts',(-0.0111272874546357,-0.036448013182065,
-0.0132064615227055));
#29953=CARTESIAN_POINT('Ctrl Pts',(-0.0126248635043253,-0.0363684364497484,
-0.0138882893794445));
#29954=CARTESIAN_POINT('Ctrl Pts',(-0.0140087691380537,-0.0362888597174317,
-0.012995773416449));
#29955=CARTESIAN_POINT('Ctrl Pts',(-0.0140049571578653,-0.036209282985115,
-0.0113494208859793));
#29956=CARTESIAN_POINT('Ctrl Pts',(-0.0126178231273385,-0.0361297062527983,
-0.0104628832890415));
#29957=CARTESIAN_POINT('Ctrl Pts',(-0.011122205955397,-0.0360501295204815,
-0.0111512105635114));
#29958=CARTESIAN_POINT('Ctrl Pts',(-0.0108933875443916,-0.0359705527881648,
-0.0127815762525112));
#29959=CARTESIAN_POINT('Ctrl Pts',(-0.0121416129538115,-0.0358909760558482,
-0.0138550511345852));
#29960=CARTESIAN_POINT('Ctrl Pts',(-0.0137193546369261,-0.0358113993235314,
-0.0133847062273992));
#29961=CARTESIAN_POINT('Ctrl Pts',(-0.014176034641121,-0.0357318225912147,
-0.0118029660266803));
#29962=CARTESIAN_POINT('Ctrl Pts',(-0.0130918084300643,-0.035652245858898,
-0.0105640510179696));
#29963=CARTESIAN_POINT('Ctrl Pts',(-0.0114634823504808,-0.0355726691265813,
-0.0108069942823203));
#29964=CARTESIAN_POINT('Ctrl Pts',(-0.010788111269722,-0.0354930923942647,
-0.0123084388550532));
#29965=CARTESIAN_POINT('Ctrl Pts',(-0.011686615166931,-0.035413515661948,
-0.0136879869128362));
#29966=CARTESIAN_POINT('Ctrl Pts',(-0.0133329290621209,-0.0353339389296312,
-0.0136773099424865));
#29967=CARTESIAN_POINT('Ctrl Pts',(-0.0142134646061913,-0.0352543621973146,
-0.0122862241125889));
#29968=CARTESIAN_POINT('Ctrl Pts',(-0.013518675602922,-0.0351747854649978,
-0.0107936655836147));
#29969=CARTESIAN_POINT('Ctrl Pts',(-0.0118873368100842,-0.0350952087326811,
-0.0105718624439518));
#29970=CARTESIAN_POINT('Ctrl Pts',(-0.0108192681836631,-0.0350156320003644,
-0.0118247360128269));
#29971=CARTESIAN_POINT('Ctrl Pts',(-0.0112964303450682,-0.0349360552680477,
-0.0134004196941601));
#29972=CARTESIAN_POINT('Ctrl Pts',(-0.0128801300896323,-0.034856478535731,
-0.013850261812295));
#29973=CARTESIAN_POINT('Ctrl Pts',(-0.0141143459209346,-0.0347769018034143,
-0.0127606866305524));
#29974=CARTESIAN_POINT('Ctrl Pts',(-0.0138643647978225,-0.0346973250710977,
-0.011133427512522));
#29975=CARTESIAN_POINT('Ctrl Pts',(-0.0123600143002392,-0.034617748338781,
-0.0104645535469199));
#29976=CARTESIAN_POINT('Ctrl Pts',(-0.010984363821632,-0.0345381716064643,
-0.0113690139162556));
#29977=CARTESIAN_POINT('Ctrl Pts',(-0.0110021585606239,-0.0344585948741475,
-0.0130152660679645));
#29978=CARTESIAN_POINT('Ctrl Pts',(-0.01239703839497,-0.0343790181418309,
-0.0138897791025832));
#29979=CARTESIAN_POINT('Ctrl Pts',(-0.0138865790444026,-0.0342994414095142,
-0.0131885434408178));
#29980=CARTESIAN_POINT('Ctrl Pts',(-0.0141013269921123,-0.0342198646771974,
-0.0115562609534022));
#29981=CARTESIAN_POINT('Ctrl Pts',(-0.0128438473225283,-0.0341402879448807,
-0.010493619113282));
#29982=CARTESIAN_POINT('Ctrl Pts',(-0.0112702413859032,-0.034060711212564,
-0.0109775893148056));
#29983=CARTESIAN_POINT('Ctrl Pts',(-0.0108272506222901,-0.0339811344802474,
-0.0125632191527937));
#29984=CARTESIAN_POINT('Ctrl Pts',(-0.0119221517713024,-0.0339015577479307,
-0.0137927126556872));
#29985=CARTESIAN_POINT('Ctrl Pts',(-0.0135483148830904,-0.0338219810156139,
-0.0135356983883403));
#29986=CARTESIAN_POINT('Ctrl Pts',(-0.0142106785147725,-0.0337424042832973,
-0.0120284700648312));
#29987=CARTESIAN_POINT('Ctrl Pts',(-0.0133002789531021,-0.0336628275509806,
-0.0106567428915664));
#29988=CARTESIAN_POINT('Ctrl Pts',(-0.0116541191238046,-0.0335832508186639,
-0.0106816550606734));
#29989=CARTESIAN_POINT('Ctrl Pts',(-0.0107856450470035,-0.0335036740863471,
-0.0120803028282286));
#29990=CARTESIAN_POINT('Ctrl Pts',(-0.0114933142064273,-0.0334240973540305,
-0.0135667977527282));
#29991=CARTESIAN_POINT('Ctrl Pts',(-0.0131265099038471,-0.0333445206217137,
-0.0137744864950621));
#29992=CARTESIAN_POINT('Ctrl Pts',(-0.0141837050795251,-0.0332649438893971,
-0.012512424230241));
#29993=CARTESIAN_POINT('Ctrl Pts',(-0.0136929358921335,-0.0331853671570804,
-0.0109409254537638));
#29994=CARTESIAN_POINT('Ctrl Pts',(-0.0121054055968104,-0.0331057904247637,
-0.0105047943253235));
#29995=CARTESIAN_POINT('Ctrl Pts',(-0.0108806574071141,-0.033026213692447,
-0.0116050009748212));
#29996=CARTESIAN_POINT('Ctrl Pts',(-0.0111447000133064,-0.0329466369601303,
-0.0132300376826758));
#29997=CARTESIAN_POINT('Ctrl Pts',(-0.012654777988866,-0.0328670602278136,
-0.013885878598978));
#29998=CARTESIAN_POINT('Ctrl Pts',(-0.0140225562149815,-0.0327874834954969,
-0.0129695568629433));
#29999=CARTESIAN_POINT('Ctrl Pts',(-0.0139905270815905,-0.0327079067631802,
-0.0113235201275212));
#30000=CARTESIAN_POINT('Ctrl Pts',(-0.0125881375254875,-0.0326283300308635,
-0.0104611012427995));
#30001=CARTESIAN_POINT('Ctrl Pts',(-0.0111047161128272,-0.0325487532985468,
-0.011175190671534));
#30002=CARTESIAN_POINT('Ctrl Pts',(-0.010904090458133,-0.0324691765662301,
-0.0128092690498018));
#30003=CARTESIAN_POINT('Ctrl Pts',(-0.0121707117266613,-0.0323895998339134,
-0.0138609977990977));
#30004=CARTESIAN_POINT('Ctrl Pts',(-0.013740073967109,-0.0323100231015967,
-0.0133634387995829));
#30005=CARTESIAN_POINT('Ctrl Pts',(-0.0141693373079339,-0.03223044636928,
-0.0117740377226941));
#30006=CARTESIAN_POINT('Ctrl Pts',(-0.0130638457237835,-0.0321508696369633,
-0.0105540577397387));
#30007=CARTESIAN_POINT('Ctrl Pts',(-0.0114399657968253,-0.0320712929046466,
-0.0108251237500537));
#30008=CARTESIAN_POINT('Ctrl Pts',(-0.0107906598547619,-0.0319917161723299,
-0.0123380231480665));
#30009=CARTESIAN_POINT('Ctrl Pts',(-0.0117128866378026,-0.0319121394400132,
-0.0137018268629841));
#30010=CARTESIAN_POINT('Ctrl Pts',(-0.0133587695076506,-0.0318325627076965,
-0.0136626813570119));
#30011=CARTESIAN_POINT('Ctrl Pts',(-0.0142151170840931,-0.0317529859753798,
-0.0122565762405104));
#30012=CARTESIAN_POINT('Ctrl Pts',(-0.0134946207250529,-0.0316734092430631,
-0.0107762560432585));
#30013=CARTESIAN_POINT('Ctrl Pts',(-0.0118596902295519,-0.0315938325107464,
-0.0105826972760627));
#30014=CARTESIAN_POINT('Ctrl Pts',(-0.0108134475319248,-0.0315142557784297,
-0.0118538537763313));
#30015=CARTESIAN_POINT('Ctrl Pts',(-0.0113177871090574,-0.031434679046113,
-0.0134210503275425));
#30016=CARTESIAN_POINT('Ctrl Pts',(-0.0129090291297876,-0.0313551023137963,
-0.013843437505964));
#30017=CARTESIAN_POINT('Ctrl Pts',(-0.0141242183453171,-0.0312755255814796,
-0.0127326823249381));
#30018=CARTESIAN_POINT('Ctrl Pts',(-0.0138461335290945,-0.0311959488491629,
-0.0111099882422067));
#30019=CARTESIAN_POINT('Ctrl Pts',(-0.0123304418888237,-0.0311163721168462,
-0.0104672318908852));
#30020=CARTESIAN_POINT('Ctrl Pts',(-0.0109706364515652,-0.0310367953845295,
-0.0113953417236122));
#30021=CARTESIAN_POINT('Ctrl Pts',(-0.0110169009129712,-0.0309572186522128,
-0.0130410490943084));
#30022=CARTESIAN_POINT('Ctrl Pts',(-0.0124266889438992,-0.0308776419198961,
-0.0138912918261311));
#30023=CARTESIAN_POINT('Ctrl Pts',(-0.0139038924648172,-0.0307980651875794,
-0.0131644356485622));
#30024=CARTESIAN_POINT('Ctrl Pts',(-0.0140903572902061,-0.0307184884552627,
-0.0115286190235464));
#30025=CARTESIAN_POINT('Ctrl Pts',(-0.0128147343019823,-0.030638911722946,
-0.0104880058767215));
#30026=CARTESIAN_POINT('Ctrl Pts',(-0.0112496463962452,-0.0305593349906293,
-0.0109988786917086));
#30027=CARTESIAN_POINT('Ctrl Pts',(-0.0108343090179921,-0.0304797582583126,
-0.0125923887825122));
#30028=CARTESIAN_POINT('Ctrl Pts',(-0.0119499886600349,-0.0304001815259959,
-0.0138018854493781));
#30029=CARTESIAN_POINT('Ctrl Pts',(-0.0135720799940484,-0.0303206047936792,
-0.0135184942152367));
#30030=CARTESIAN_POINT('Ctrl Pts',(-0.0142070920787441,-0.0302410259785769,
-0.0119965393797492));
#30031=CARTESIAN_POINT('Ctrl Pts',(-0.0135860713130062,-0.0301879727409135,
-0.0110981414046974));
#30032=CARTESIAN_POINT('Ctrl Pts',(-0.0131541181402127,-0.0301614450806891,
-0.0108800893118964));
#30033=CARTESIAN_POINT('Ctrl Pts',(-0.0135933120633907,-0.0367413093788616,
-0.01108278638379));
#30034=CARTESIAN_POINT('Ctrl Pts',(-0.0132289214753065,-0.0367147808270613,
-0.0107183076053843));
#30035=CARTESIAN_POINT('Ctrl Pts',(-0.0121132315573896,-0.0366617266978222,
-0.0103889931429711));
#30036=CARTESIAN_POINT('Ctrl Pts',(-0.0107847316759526,-0.0365821469911441,
-0.0115380665878402));
#30037=CARTESIAN_POINT('Ctrl Pts',(-0.0110379215294415,-0.0365025702588274,
-0.0132735558745762));
#30038=CARTESIAN_POINT('Ctrl Pts',(-0.0126329923311686,-0.0364229935265107,
-0.0139997718863199));
#30039=CARTESIAN_POINT('Ctrl Pts',(-0.0141069925792118,-0.036343416794194,
-0.0130491516136838));
#30040=CARTESIAN_POINT('Ctrl Pts',(-0.0141029324326193,-0.0362638400618773,
-0.0112956187288288));
#30041=CARTESIAN_POINT('Ctrl Pts',(-0.0126254936136463,-0.0361842633295606,
-0.010351366024065));
#30042=CARTESIAN_POINT('Ctrl Pts',(-0.0110325092159457,-0.0361046865972439,
-0.0110845045767061));
#30043=CARTESIAN_POINT('Ctrl Pts',(-0.0107887943365794,-0.0360251098649272,
-0.0128210098494769));
#30044=CARTESIAN_POINT('Ctrl Pts',(-0.0121182813465727,-0.0359455331326105,
-0.0139643697750972));
#30045=CARTESIAN_POINT('Ctrl Pts',(-0.0137987367010273,-0.0358659564002938,
-0.0134634046131951));
#30046=CARTESIAN_POINT('Ctrl Pts',(-0.0142851473514748,-0.0357863796679771,
-0.0117786904308283));
#30047=CARTESIAN_POINT('Ctrl Pts',(-0.0131303361670396,-0.0357068029356604,
-0.010459119944491));
#30048=CARTESIAN_POINT('Ctrl Pts',(-0.0113960032857326,-0.0356272262033437,
-0.0107178792292181));
#30049=CARTESIAN_POINT('Ctrl Pts',(-0.0106766643970847,-0.035547649471027,
-0.0123170704014292));
#30050=CARTESIAN_POINT('Ctrl Pts',(-0.0116336624286527,-0.0354680727387103,
-0.0137864293879092));
#30051=CARTESIAN_POINT('Ctrl Pts',(-0.0133871541630052,-0.0353884960063937,
-0.013775057328601));
#30052=CARTESIAN_POINT('Ctrl Pts',(-0.0143250140710351,-0.0353089192740769,
-0.0122934094413862));
#30053=CARTESIAN_POINT('Ctrl Pts',(-0.0135849931200419,-0.0352293425417602,
-0.0107036828095206));
#30054=CARTESIAN_POINT('Ctrl Pts',(-0.0118474513927153,-0.0351497658094436,
-0.0104674399076118));
#30055=CARTESIAN_POINT('Ctrl Pts',(-0.0107098496792009,-0.0350701890771268,
-0.0118018776801594));
#30056=CARTESIAN_POINT('Ctrl Pts',(-0.0112180759101854,-0.0349906123448101,
-0.0134801410534109));
#30057=CARTESIAN_POINT('Ctrl Pts',(-0.0129048772060397,-0.0349110356124935,
-0.0139592686597671));
#30058=CARTESIAN_POINT('Ctrl Pts',(-0.014219442590514,-0.0348314588801767,
-0.0127987602775421));
#30059=CARTESIAN_POINT('Ctrl Pts',(-0.0139531872704309,-0.0347518821478601,
-0.0110655638188028));
#30060=CARTESIAN_POINT('Ctrl Pts',(-0.0123509009927115,-0.0346723054155433,
-0.0103531450185766));
#30061=CARTESIAN_POINT('Ctrl Pts',(-0.0108856933244511,-0.0345927286832267,
-0.0113164872987539));
#30062=CARTESIAN_POINT('Ctrl Pts',(-0.0109046465312656,-0.03451315195091,
-0.0130699132700196));
#30063=CARTESIAN_POINT('Ctrl Pts',(-0.0123903354190819,-0.0344335752185932,
-0.014001358592973));
#30064=CARTESIAN_POINT('Ctrl Pts',(-0.0139768477023065,-0.0343539984862765,
-0.0132544712950332));
#30065=CARTESIAN_POINT('Ctrl Pts',(-0.014205576107247,-0.0342744217539599,
-0.0115159244370042));
#30066=CARTESIAN_POINT('Ctrl Pts',(-0.0128662323689877,-0.0341948450216431,
-0.0103841028028237));
#30067=CARTESIAN_POINT('Ctrl Pts',(-0.0111901820051644,-0.0341152682893264,
-0.0108995802889362));
#30068=CARTESIAN_POINT('Ctrl Pts',(-0.0107183517881809,-0.0340356915570098,
-0.0125884373305846));
#30069=CARTESIAN_POINT('Ctrl Pts',(-0.0118845328672181,-0.0339561148246931,
-0.0138979729550261));
#30070=CARTESIAN_POINT('Ctrl Pts',(-0.0136165619678413,-0.0338765380923764,
-0.0136242266210369));
#30071=CARTESIAN_POINT('Ctrl Pts',(-0.0143220466003186,-0.0337969613600597,
-0.0120188751660214));
#30072=CARTESIAN_POINT('Ctrl Pts',(-0.013352378476268,-0.0337173846277429,
-0.0105578462169646));
#30073=CARTESIAN_POINT('Ctrl Pts',(-0.0115990508377599,-0.0336378078954263,
-0.0105843802107197));
#30074=CARTESIAN_POINT('Ctrl Pts',(-0.010674037619066,-0.0335582311631095,
-0.0120740823306159));
#30075=CARTESIAN_POINT('Ctrl Pts',(-0.0114277772463213,-0.0334786544307928,
-0.0136573506070259));
#30076=CARTESIAN_POINT('Ctrl Pts',(-0.0131672967658813,-0.0333990776984761,
-0.013878560240295));
#30077=CARTESIAN_POINT('Ctrl Pts',(-0.014293317148486,-0.0333195009661594,
-0.0125343355720417));
#30078=CARTESIAN_POINT('Ctrl Pts',(-0.013770598050943,-0.0332399242338428,
-0.0108605295480818));
#30079=CARTESIAN_POINT('Ctrl Pts',(-0.0120797168289496,-0.0331603475015261,
-0.0103960055402067));
#30080=CARTESIAN_POINT('Ctrl Pts',(-0.0107752354456785,-0.0330807707692093,
-0.0115678375168489));
#30081=CARTESIAN_POINT('Ctrl Pts',(-0.0110564676753449,-0.0330011940368927,
-0.013298666882724));
#30082=CARTESIAN_POINT('Ctrl Pts',(-0.012664854299614,-0.0329216173045759,
-0.0139972041599381));
#30083=CARTESIAN_POINT('Ctrl Pts',(-0.0141216772183346,-0.0328420405722592,
-0.0130212283178836));
#30084=CARTESIAN_POINT('Ctrl Pts',(-0.0140875629337964,-0.0327624638399425,
-0.0112680317868718));
#30085=CARTESIAN_POINT('Ctrl Pts',(-0.0125938754285439,-0.0326828871076258,
-0.0103494679635769));
#30086=CARTESIAN_POINT('Ctrl Pts',(-0.0110138807548298,-0.0326033103753091,
-0.0111100458306123));
#30087=CARTESIAN_POINT('Ctrl Pts',(-0.0108001940282382,-0.0325237336429924,
-0.0128505054950474));
#30088=CARTESIAN_POINT('Ctrl Pts',(-0.0121492744991063,-0.0324441569106758,
-0.0139707035775999));
#30089=CARTESIAN_POINT('Ctrl Pts',(-0.0138208048949018,-0.0323645801783591,
-0.0134407526395977));
#30090=CARTESIAN_POINT('Ctrl Pts',(-0.014278014010488,-0.0322850034460424,
-0.0117478788449718));
#30091=CARTESIAN_POINT('Ctrl Pts',(-0.0131005530409439,-0.0322054267137256,
-0.0104484760868233));
#30092=CARTESIAN_POINT('Ctrl Pts',(-0.0113709557643723,-0.032125849981409,
-0.0107371889561855));
#30093=CARTESIAN_POINT('Ctrl Pts',(-0.0106793788993524,-0.0320462732490923,
-0.0123485806823159));
#30094=CARTESIAN_POINT('Ctrl Pts',(-0.0116616442170328,-0.0319666965167755,
-0.0138011703423888));
#30095=CARTESIAN_POINT('Ctrl Pts',(-0.0134146768655595,-0.0318871197844589,
-0.0137594763972914));
#30096=CARTESIAN_POINT('Ctrl Pts',(-0.0143267741280635,-0.0318075430521422,
-0.0122618314423287));
#30097=CARTESIAN_POINT('Ctrl Pts',(-0.0135593722286447,-0.0317279663198255,
-0.0106851398784292));
#30098=CARTESIAN_POINT('Ctrl Pts',(-0.011818004972693,-0.0316483895875088,
-0.010478980105751));
#30099=CARTESIAN_POINT('Ctrl Pts',(-0.0107036500931186,-0.031568812855192,
-0.0118328910596716));
#30100=CARTESIAN_POINT('Ctrl Pts',(-0.0112408230358926,-0.0314892361228754,
-0.0135021147761719));
#30101=CARTESIAN_POINT('Ctrl Pts',(-0.0129356576229402,-0.0314096593905587,
-0.0139520000794683));
#30102=CARTESIAN_POINT('Ctrl Pts',(-0.0142299577265421,-0.031330082658242,
-0.0127689328439255));
#30103=CARTESIAN_POINT('Ctrl Pts',(-0.0139337691150506,-0.0312505059259253,
-0.01104059861206));
#30104=CARTESIAN_POINT('Ctrl Pts',(-0.0123194033669345,-0.0311709291936086,
-0.0103559977272969));
#30105=CARTESIAN_POINT('Ctrl Pts',(-0.0108710722792076,-0.0310913524612919,
-0.0113445290912203));
#30106=CARTESIAN_POINT('Ctrl Pts',(-0.0109203486358651,-0.0310117757289752,
-0.0130973748153013));
#30107=CARTESIAN_POINT('Ctrl Pts',(-0.0124219162692576,-0.0309321989966585,
-0.0140029697974007));
#30108=CARTESIAN_POINT('Ctrl Pts',(-0.0139952882558845,-0.0308526222643418,
-0.0132287940444329));
#30109=CARTESIAN_POINT('Ctrl Pts',(-0.0141938922590592,-0.0307730455320251,
-0.0114864829704253));
#30110=CARTESIAN_POINT('Ctrl Pts',(-0.0128352240412084,-0.0306934687997084,
-0.0103781241350006));
#30111=CARTESIAN_POINT('Ctrl Pts',(-0.011168246246595,-0.0306138920673917,
-0.0109222556405432));
#30112=CARTESIAN_POINT('Ctrl Pts',(-0.0107258696974676,-0.030534315335075,
-0.0126195059528898));
#30113=CARTESIAN_POINT('Ctrl Pts',(-0.0119141819848288,-0.0304547386027583,
-0.0139077429132125));
#30114=CARTESIAN_POINT('Ctrl Pts',(-0.013641874228008,-0.0303751618704416,
-0.013605902426956));
#30115=CARTESIAN_POINT('Ctrl Pts',(-0.0143182266811951,-0.0302955830553393,
-0.0119848657389449));
#30116=CARTESIAN_POINT('Ctrl Pts',(-0.0136567764056649,-0.030242529817676,
-0.011027980525247));
#30117=CARTESIAN_POINT('Ctrl Pts',(-0.0131967023454666,-0.0302160021574515,
-0.0107957328697411));
#30118=CARTESIAN_POINT('Ctrl Pts',(-0.0131954570230152,-0.0302142743898723,
-0.0107984686165627));
#30119=CARTESIAN_POINT('Ctrl Pts',(-0.0133260842763136,-0.0302142743898723,
-0.0108797587666653));
#30120=CARTESIAN_POINT('Ctrl Pts',(-0.0134431964764062,-0.0302142743898653,
-0.0109820158739861));
#30121=CARTESIAN_POINT('Ctrl Pts',(-0.0135427737583255,-0.0302142743898653,
-0.0110992550752643));
#30122=CARTESIAN_POINT('Ctrl Pts',(-0.0136693246268282,-0.0302142743898653,
-0.0112482521402409));
#30123=CARTESIAN_POINT('Ctrl Pts',(-0.0137677960716114,-0.0302142743898653,
-0.0114216612142502));
#30124=CARTESIAN_POINT('Ctrl Pts',(-0.0138291125118522,-0.0302142743898653,
-0.0116070749220759));
#30125=CARTESIAN_POINT('Ctrl Pts',(-0.0138679675928177,-0.0302142743898653,
-0.0117245681196817));
#30126=CARTESIAN_POINT('Ctrl Pts',(-0.0138918683604881,-0.0302142743898653,
-0.0118468920339111));
#30127=CARTESIAN_POINT('Ctrl Pts',(-0.0138981744272313,-0.0302142743898653,
-0.0119704513331141));
#30128=CARTESIAN_POINT('Ctrl Pts',(-0.0138992054768938,-0.0302142743898653,
-0.0119906534303858));
#30129=CARTESIAN_POINT('Ctrl Pts',(-0.0138997541990176,-0.0302142743898653,
-0.012010717926216));
#30130=CARTESIAN_POINT('Ctrl Pts',(-0.0138998410206969,-0.0302142743898653,
-0.0120304353897606));
#30131=CARTESIAN_POINT('Ctrl Pts',(-0.0139004085534207,-0.0302142743898653,
-0.0121593237721184));
#30132=CARTESIAN_POINT('Ctrl Pts',(-0.0138816703521106,-0.0302142743898653,
-0.0122755108733013));
#30133=CARTESIAN_POINT('Ctrl Pts',(-0.0138553750738999,-0.0302142743898653,
-0.0123756473142824));
#30134=CARTESIAN_POINT('Ctrl Pts',(-0.0138312935973491,-0.0302142743898653,
-0.0124673532599672));
#30135=CARTESIAN_POINT('Ctrl Pts',(-0.0138018158230822,-0.0302142743898653,
-0.0125455369110881));
#30136=CARTESIAN_POINT('Ctrl Pts',(-0.0137643803753388,-0.0302142743898653,
-0.0126240412720506));
#30137=CARTESIAN_POINT('Ctrl Pts',(-0.0137113315160428,-0.0302142743898653,
-0.0127352878858845));
#30138=CARTESIAN_POINT('Ctrl Pts',(-0.0136436767058198,-0.0302142743898653,
-0.0128397240745112));
#30139=CARTESIAN_POINT('Ctrl Pts',(-0.0135632704999152,-0.0302142743898653,
-0.0129326775871141));
#30140=CARTESIAN_POINT('Ctrl Pts',(-0.013482385375445,-0.0302142743898653,
-0.0130261847530378));
#30141=CARTESIAN_POINT('Ctrl Pts',(-0.0133921506665608,-0.0302142743898714,
-0.0131045911547339));
#30142=CARTESIAN_POINT('Ctrl Pts',(-0.0132924108208383,-0.0302142743898722,
-0.0131679081118086));
#30143=CARTESIAN_POINT('Ctrl Pts',(-0.0132850639690017,-0.0302142743898722,
-0.0131725720482625));
#30144=CARTESIAN_POINT('Ctrl Pts',(-0.0132776640935926,-0.0302142743898723,
-0.0131771523321702));
#30145=CARTESIAN_POINT('Ctrl Pts',(-0.0132702116598217,-0.0302142743898723,
-0.0131816495199757));
#30146=CARTESIAN_POINT('Ctrl Pts',(-0.0118276163558221,-0.0365771045634534,
-0.0135678901963669));
#30147=CARTESIAN_POINT('Ctrl Pts',(-0.0122917136632024,-0.0365505737722603,
-0.0137920680337233));
#30148=CARTESIAN_POINT('Ctrl Pts',(-0.0134536276171895,-0.0364975174036282,
-0.0137355881186744));
#30149=CARTESIAN_POINT('Ctrl Pts',(-0.0143295251580393,-0.0364179354575572,
-0.0122131193629488));
#30150=CARTESIAN_POINT('Ctrl Pts',(-0.0135189123462146,-0.0363383587252405,
-0.0106579330577131));
#30151=CARTESIAN_POINT('Ctrl Pts',(-0.0117737475226801,-0.0362587819929238,
-0.0104975924690421));
#30152=CARTESIAN_POINT('Ctrl Pts',(-0.0106951402918064,-0.0361792052606071,
-0.0118805694294325));
#30153=CARTESIAN_POINT('Ctrl Pts',(-0.0112764794961299,-0.0360996285282904,
-0.0135348382648464));
#30154=CARTESIAN_POINT('Ctrl Pts',(-0.0129823888886079,-0.0360200517959737,
-0.0139397807062913));
#30155=CARTESIAN_POINT('Ctrl Pts',(-0.0142449610580027,-0.035940475063657,
-0.0127229535318522));
#30156=CARTESIAN_POINT('Ctrl Pts',(-0.0139031673111846,-0.0358608983313403,
-0.0110031597499392));
#30157=CARTESIAN_POINT('Ctrl Pts',(-0.0122713737247802,-0.0357813215990236,
-0.0103615029742666));
#30158=CARTESIAN_POINT('Ctrl Pts',(-0.0108497517033239,-0.0357017448667069,
-0.0113879302746));
#30159=CARTESIAN_POINT('Ctrl Pts',(-0.010945346434419,-0.0356221681343902,
-0.0131387543260284));
#30160=CARTESIAN_POINT('Ctrl Pts',(-0.012470251992075,-0.0355425914020735,
-0.0140043085907352));
#30161=CARTESIAN_POINT('Ctrl Pts',(-0.0140225104888412,-0.0354630146697568,
-0.0131888170585244));
#30162=CARTESIAN_POINT('Ctrl Pts',(-0.0141750019870238,-0.0353834379374401,
-0.0114420276670381));
#30163=CARTESIAN_POINT('Ctrl Pts',(-0.0127875314436345,-0.0353038612051234,
-0.0103699024202048));
#30164=CARTESIAN_POINT('Ctrl Pts',(-0.0111357098566257,-0.0352242844728067,
-0.0109581319803875));
#30165=CARTESIAN_POINT('Ctrl Pts',(-0.0107381892442877,-0.03514470774049,
-0.0126659097821878));
#30166=CARTESIAN_POINT('Ctrl Pts',(-0.0119604416488503,-0.0350651310081733,
-0.0139231396018729));
#30167=CARTESIAN_POINT('Ctrl Pts',(-0.0136787531423359,-0.0349855542758566,
-0.0135739497373915));
#30168=CARTESIAN_POINT('Ctrl Pts',(-0.0143133428273887,-0.0349059775435399,
-0.0119393783113244));
#30169=CARTESIAN_POINT('Ctrl Pts',(-0.0132807818460022,-0.0348264008112232,
-0.0105222171845282));
#30170=CARTESIAN_POINT('Ctrl Pts',(-0.0115303858334339,-0.0347468240789065,
-0.010625375614492));
#30171=CARTESIAN_POINT('Ctrl Pts',(-0.0106714334602556,-0.0346672473465898,
-0.0121540118248493));
#30172=CARTESIAN_POINT('Ctrl Pts',(-0.0114936281414464,-0.0345876706142731,
-0.0137027286336875));
#30173=CARTESIAN_POINT('Ctrl Pts',(-0.0132410607364181,-0.0345080938819564,
-0.0138476671599599));
#30174=CARTESIAN_POINT('Ctrl Pts',(-0.0143071770926239,-0.0344285171496397,
-0.0124555738575412));
#30175=CARTESIAN_POINT('Ctrl Pts',(-0.0137118114169886,-0.0343489404173231,
-0.010806311125067));
#30176=CARTESIAN_POINT('Ctrl Pts',(-0.0120023308578284,-0.0342693636850063,
-0.0104161777291886));
#30177=CARTESIAN_POINT('Ctrl Pts',(-0.0107503972326347,-0.0341897869526896,
-0.0116438544156386));
#30178=CARTESIAN_POINT('Ctrl Pts',(-0.011107012970546,-0.0341102102203729,
-0.0133606400935724));
#30179=CARTESIAN_POINT('Ctrl Pts',(-0.0127443127819797,-0.0340306334880562,
-0.0139881567674452));
#30180=CARTESIAN_POINT('Ctrl Pts',(-0.0141569963678234,-0.0339510567557395,
-0.0129494783115481));
#30181=CARTESIAN_POINT('Ctrl Pts',(-0.0140462710394181,-0.0338714800234228,
-0.0111995446699121));
#30182=CARTESIAN_POINT('Ctrl Pts',(-0.012513935422026,-0.0337919032911062,
-0.0103472094048007));
#30183=CARTESIAN_POINT('Ctrl Pts',(-0.0109687878597513,-0.0337123265587894,
-0.0111760923032072));
#30184=CARTESIAN_POINT('Ctrl Pts',(-0.0108314057394338,-0.0336327498264727,
-0.0129241352092867));
#30185=CARTESIAN_POINT('Ctrl Pts',(-0.0122280954011582,-0.033553173094156,
-0.0139842228647708));
#30186=CARTESIAN_POINT('Ctrl Pts',(-0.0138747686462785,-0.0334735963618394,
-0.0133817321409568));
#30187=CARTESIAN_POINT('Ctrl Pts',(-0.0142575074305579,-0.0333940196295226,
-0.0116705808117385));
#30188=CARTESIAN_POINT('Ctrl Pts',(-0.0130244294643756,-0.0333144428972059,
-0.0104239667664972));
#30189=CARTESIAN_POINT('Ctrl Pts',(-0.0113092016658568,-0.0332348661648893,
-0.0107880017204034));
#30190=CARTESIAN_POINT('Ctrl Pts',(-0.0106887697477285,-0.0331552894325725,
-0.0124279993068177));
#30191=CARTESIAN_POINT('Ctrl Pts',(-0.0117335462547127,-0.0330757127002559,
-0.0138361789469668));
#30192=CARTESIAN_POINT('Ctrl Pts',(-0.0134829848180596,-0.0329961359679391,
-0.0137178887886596));
#30193=CARTESIAN_POINT('Ctrl Pts',(-0.0143286870404645,-0.0329165592356225,
-0.0121818824086282));
#30194=CARTESIAN_POINT('Ctrl Pts',(-0.0134931314201099,-0.0328369825033058,
-0.0106403329758275));
#30195=CARTESIAN_POINT('Ctrl Pts',(-0.0117445108783079,-0.032757405770989,
-0.0105105098297045));
#30196=CARTESIAN_POINT('Ctrl Pts',(-0.010690471739919,-0.0326778290386723,
-0.0119117697425059));
#30197=CARTESIAN_POINT('Ctrl Pts',(-0.0113000762494755,-0.0325982523063557,
-0.0135558227192634));
#30198=CARTESIAN_POINT('Ctrl Pts',(-0.0130128663625058,-0.0325186755740389,
-0.0139311597374413));
#30199=CARTESIAN_POINT('Ctrl Pts',(-0.0142541375249437,-0.0324390988417222,
-0.0126927035412902));
#30200=CARTESIAN_POINT('Ctrl Pts',(-0.0138826901599497,-0.0323595221094056,
-0.0109790656847457));
#30201=CARTESIAN_POINT('Ctrl Pts',(-0.0122400254547557,-0.0322799453770889,
-0.0103657301199557));
#30202=CARTESIAN_POINT('Ctrl Pts',(-0.010836376083328,-0.0322003686447722,
-0.0114165851482747));
#30203=CARTESIAN_POINT('Ctrl Pts',(-0.0109622288601596,-0.0321207919124554,
-0.0131654959310685));
#30204=CARTESIAN_POINT('Ctrl Pts',(-0.01250187729083,-0.0320412151801387,
-0.0140045493026142));
#30205=CARTESIAN_POINT('Ctrl Pts',(-0.014039799777464,-0.0319616384478221,
-0.0131623365783801));
#30206=CARTESIAN_POINT('Ctrl Pts',(-0.0141620615239816,-0.0318820617155053,
-0.0114131710892561));
#30207=CARTESIAN_POINT('Ctrl Pts',(-0.0127562575510713,-0.0318024849831886,
-0.0103652001677907));
#30208=CARTESIAN_POINT('Ctrl Pts',(-0.0111148555797449,-0.0317229082508719,
-0.0109819070739547));
#30209=CARTESIAN_POINT('Ctrl Pts',(-0.010746927334201,-0.0316433315185553,
-0.0126963039420751));
#30210=CARTESIAN_POINT('Ctrl Pts',(-0.0119907386284374,-0.0315637547862386,
-0.0139322090413572));
#30211=CARTESIAN_POINT('Ctrl Pts',(-0.0137027544748348,-0.0314841780539219,
-0.0135533561653636));
#30212=CARTESIAN_POINT('Ctrl Pts',(-0.0143089822891687,-0.0314046013216051,
-0.0119080551306944));
#30213=CARTESIAN_POINT('Ctrl Pts',(-0.0132520682526874,-0.0313250245892885,
-0.0105089621065284));
#30214=CARTESIAN_POINT('Ctrl Pts',(-0.0115037181928097,-0.0312454478569718,
-0.0106423754559198));
#30215=CARTESIAN_POINT('Ctrl Pts',(-0.0106713288761103,-0.0311658711246551,
-0.0121856365681985));
#30216=CARTESIAN_POINT('Ctrl Pts',(-0.0115201838829843,-0.0310862943923384,
-0.0137199044904323));
#30217=CARTESIAN_POINT('Ctrl Pts',(-0.0132698598521949,-0.0310067176600217,
-0.0138346003826415));
#30218=CARTESIAN_POINT('Ctrl Pts',(-0.0143117463657834,-0.030927140927705,
-0.0124242827927081));
#30219=CARTESIAN_POINT('Ctrl Pts',(-0.0136879420663563,-0.0308475641953883,
-0.0107855545142021));
#30220=CARTESIAN_POINT('Ctrl Pts',(-0.0119719830161943,-0.0307679874630716,
-0.0104250572679376));
#30221=CARTESIAN_POINT('Ctrl Pts',(-0.0107414430352204,-0.0306884107307549,
-0.0116741709428668));
#30222=CARTESIAN_POINT('Ctrl Pts',(-0.0111277405067114,-0.0306088339984382,
-0.0133845893474986));
#30223=CARTESIAN_POINT('Ctrl Pts',(-0.0127755584842204,-0.0305292572661215,
-0.0139835894720614));
#30224=CARTESIAN_POINT('Ctrl Pts',(-0.0141702391738808,-0.0304496805338048,
-0.0129208447123972));
#30225=CARTESIAN_POINT('Ctrl Pts',(-0.0140289409519074,-0.0303701038014881,
-0.011172687498663));
#30226=CARTESIAN_POINT('Ctrl Pts',(-0.0124827243982298,-0.0302905270691714,
-0.0103477488737881));
#30227=CARTESIAN_POINT('Ctrl Pts',(-0.0109509240039545,-0.0302109503368547,
-0.011201730797944));
#30228=CARTESIAN_POINT('Ctrl Pts',(-0.0108462080022495,-0.0301313676081364,
-0.0129550712823894));
#30229=CARTESIAN_POINT('Ctrl Pts',(-0.0117860020704321,-0.030078310456857,
-0.0136406945510677));
#30230=CARTESIAN_POINT('Ctrl Pts',(-0.0122969585536011,-0.0300517788830164,
-0.0137083808366907));
#30231=CARTESIAN_POINT('Ctrl Pts',(-0.0118688946792067,-0.0366318983236434,
-0.0134824316189254));
#30232=CARTESIAN_POINT('Ctrl Pts',(-0.0123045005756168,-0.0366053675324501,
-0.0136928469483057));
#30233=CARTESIAN_POINT('Ctrl Pts',(-0.0133950834370751,-0.0365523111638182,
-0.0136398343933247));
#30234=CARTESIAN_POINT('Ctrl Pts',(-0.0142172087271331,-0.0364727292177471,
-0.0122108315601954));
#30235=CARTESIAN_POINT('Ctrl Pts',(-0.0134563602694476,-0.0363931524854304,
-0.0107511197415665));
#30236=CARTESIAN_POINT('Ctrl Pts',(-0.0118183329091291,-0.0363135757531137,
-0.0106006226265257));
#30237=CARTESIAN_POINT('Ctrl Pts',(-0.0108059424853809,-0.0362339990207971,
-0.0118986972090865));
#30238=CARTESIAN_POINT('Ctrl Pts',(-0.0113515926781112,-0.0361544222884804,
-0.013451408779471));
#30239=CARTESIAN_POINT('Ctrl Pts',(-0.0129527745386553,-0.0360748455561636,
-0.0138314913879993));
#30240=CARTESIAN_POINT('Ctrl Pts',(-0.0141378361041622,-0.035995268823847,
-0.0126893664851646));
#30241=CARTESIAN_POINT('Ctrl Pts',(-0.0138170254269563,-0.0359156920915303,
-0.0110751526121313));
#30242=CARTESIAN_POINT('Ctrl Pts',(-0.0122854093269314,-0.0358361153592136,
-0.0104728878057866));
#30243=CARTESIAN_POINT('Ctrl Pts',(-0.0109510621433456,-0.0357565386268968,
-0.0114363016785914));
#30244=CARTESIAN_POINT('Ctrl Pts',(-0.0110407882155906,-0.0356769618945802,
-0.0130796408409835));
#30245=CARTESIAN_POINT('Ctrl Pts',(-0.0124720782528739,-0.0355973851622634,
-0.0138920578392579));
#30246=CARTESIAN_POINT('Ctrl Pts',(-0.0139290420042062,-0.0355178084299468,
-0.0131266301708478));
#30247=CARTESIAN_POINT('Ctrl Pts',(-0.0140721718924953,-0.0354382316976301,
-0.0114870779764748));
#30248=CARTESIAN_POINT('Ctrl Pts',(-0.0127698795926172,-0.0353586549653134,
-0.0104807716011009));
#30249=CARTESIAN_POINT('Ctrl Pts',(-0.0112194650315414,-0.0352790782329967,
-0.0110328891436582));
#30250=CARTESIAN_POINT('Ctrl Pts',(-0.0108463486183986,-0.0351995015006799,
-0.012635824709955));
#30251=CARTESIAN_POINT('Ctrl Pts',(-0.0119935656909004,-0.0351199247683633,
-0.0138158718980947));
#30252=CARTESIAN_POINT('Ctrl Pts',(-0.0136063882747172,-0.0350403480360466,
-0.0134881191584951));
#30253=CARTESIAN_POINT('Ctrl Pts',(-0.0142020198464027,-0.0349607713037299,
-0.011953895753241));
#30254=CARTESIAN_POINT('Ctrl Pts',(-0.0132328488455326,-0.0348811945714132,
-0.0106237356054045));
#30255=CARTESIAN_POINT('Ctrl Pts',(-0.011589911444255,-0.0348016178390965,
-0.0107205610332662));
#30256=CARTESIAN_POINT('Ctrl Pts',(-0.0107836910405988,-0.0347220411067798,
-0.0121553526946449));
#30257=CARTESIAN_POINT('Ctrl Pts',(-0.0115554103447796,-0.0346424643744631,
-0.0136089921859133));
#30258=CARTESIAN_POINT('Ctrl Pts',(-0.0131955662557146,-0.0345628876421464,
-0.0137450327870055));
#30259=CARTESIAN_POINT('Ctrl Pts',(-0.014196232632436,-0.0344833109098297,
-0.0124384015240285));
#30260=CARTESIAN_POINT('Ctrl Pts',(-0.0136374170678924,-0.034403734177513,
-0.010890388726776));
#30261=CARTESIAN_POINT('Ctrl Pts',(-0.0120328832782612,-0.0343241574451963,
-0.0105242060212774));
#30262=CARTESIAN_POINT('Ctrl Pts',(-0.0108578071457864,-0.0342445807128796,
-0.0116765143734234));
#30263=CARTESIAN_POINT('Ctrl Pts',(-0.0111925298768096,-0.0341650039805629,
-0.0132879048130742));
#30264=CARTESIAN_POINT('Ctrl Pts',(-0.0127293141690466,-0.0340854272482462,
-0.01387689759301));
#30265=CARTESIAN_POINT('Ctrl Pts',(-0.0140552716567745,-0.0340058505159295,
-0.0129019846756805));
#30266=CARTESIAN_POINT('Ctrl Pts',(-0.0139513438701481,-0.0339262737836128,
-0.0112594812599081));
#30267=CARTESIAN_POINT('Ctrl Pts',(-0.0125130799121368,-0.0338466970512961,
-0.0104594717332497));
#30268=CARTESIAN_POINT('Ctrl Pts',(-0.0110627905477149,-0.0337671203189794,
-0.0112374686581132));
#30269=CARTESIAN_POINT('Ctrl Pts',(-0.0109338424570453,-0.0336875435866627,
-0.0128781974125294));
#30270=CARTESIAN_POINT('Ctrl Pts',(-0.0122447879041034,-0.033607966854346,
-0.0138732051966662));
#30271=CARTESIAN_POINT('Ctrl Pts',(-0.0137903701852936,-0.0335283901220293,
-0.013307701997979));
#30272=CARTESIAN_POINT('Ctrl Pts',(-0.0141496122420036,-0.0334488133897126,
-0.0117016000085817));
#30273=CARTESIAN_POINT('Ctrl Pts',(-0.0129922342002428,-0.0333692366573959,
-0.0105315168815755));
#30274=CARTESIAN_POINT('Ctrl Pts',(-0.0113823060001877,-0.0332896599250792,
-0.0108732033552937));
#30275=CARTESIAN_POINT('Ctrl Pts',(-0.0107999630355553,-0.0332100831927625,
-0.0124125198033311));
#30276=CARTESIAN_POINT('Ctrl Pts',(-0.0117805996383446,-0.0331305064604458,
-0.0137342498472222));
#30277=CARTESIAN_POINT('Ctrl Pts',(-0.0134226383691933,-0.0330509297281291,
-0.0136232216433812));
#30278=CARTESIAN_POINT('Ctrl Pts',(-0.0142164220624582,-0.0329713529958124,
-0.012181512274624));
#30279=CARTESIAN_POINT('Ctrl Pts',(-0.0134321620609091,-0.0328917762634957,
-0.0107346001468076));
#30280=CARTESIAN_POINT('Ctrl Pts',(-0.0117908911324214,-0.0328121995311791,
-0.010612746977133));
#30281=CARTESIAN_POINT('Ctrl Pts',(-0.010801560540695,-0.0327326227988623,
-0.0119279821028546));
#30282=CARTESIAN_POINT('Ctrl Pts',(-0.0113737408025024,-0.0326530460665456,
-0.0134711049766514));
#30283=CARTESIAN_POINT('Ctrl Pts',(-0.012981380969088,-0.0325734693342289,
-0.0138233996692927));
#30284=CARTESIAN_POINT('Ctrl Pts',(-0.0141464492183606,-0.0324938926019122,
-0.0126609735726318));
#30285=CARTESIAN_POINT('Ctrl Pts',(-0.0137978053890942,-0.0324143158695955,
-0.0110525377063779));
#30286=CARTESIAN_POINT('Ctrl Pts',(-0.0122559855594419,-0.0323347391372789,
-0.0104768554426548));
#30287=CARTESIAN_POINT('Ctrl Pts',(-0.0109385076664164,-0.0322551624049621,
-0.011463197400103));
#30288=CARTESIAN_POINT('Ctrl Pts',(-0.0110566342118533,-0.0321755856726455,
-0.0131047407513895));
#30289=CARTESIAN_POINT('Ctrl Pts',(-0.0125017620420153,-0.0320960089403287,
-0.013892283773587));
#30290=CARTESIAN_POINT('Ctrl Pts',(-0.0139452698856203,-0.032016432208012,
-0.0131017753546116));
#30291=CARTESIAN_POINT('Ctrl Pts',(-0.0140600258577871,-0.0319368554756953,
-0.0114599929336785));
#30292=CARTESIAN_POINT('Ctrl Pts',(-0.0127405256364799,-0.0318572787433787,
-0.0104763580247982));
#30293=CARTESIAN_POINT('Ctrl Pts',(-0.0111998910201647,-0.0317777020110619,
-0.0110552046597814));
#30294=CARTESIAN_POINT('Ctrl Pts',(-0.010854550267986,-0.0316981252787452,
-0.0126643529411099));
#30295=CARTESIAN_POINT('Ctrl Pts',(-0.0120220027077538,-0.0316185485464285,
-0.0138243845553623));
#30296=CARTESIAN_POINT('Ctrl Pts',(-0.0136289161407313,-0.0315389718141119,
-0.013468789847032));
#30297=CARTESIAN_POINT('Ctrl Pts',(-0.0141979270061085,-0.0314593950817952,
-0.0119244955348821));
#30298=CARTESIAN_POINT('Ctrl Pts',(-0.01320589800924,-0.0313798183494785,
-0.0106112942702744));
#30299=CARTESIAN_POINT('Ctrl Pts',(-0.0115648809575133,-0.0313002416171617,
-0.0107365172369465));
#30300=CARTESIAN_POINT('Ctrl Pts',(-0.0107835928769817,-0.031220664884845,
-0.0121850359624776));
#30301=CARTESIAN_POINT('Ctrl Pts',(-0.011580335802035,-0.0311410881525283,
-0.0136251135991492));
#30302=CARTESIAN_POINT('Ctrl Pts',(-0.0132225973641571,-0.0310615114202117,
-0.0137327681925843));
#30303=CARTESIAN_POINT('Ctrl Pts',(-0.0142005213932173,-0.0309819346878949,
-0.0124090314498447));
#30304=CARTESIAN_POINT('Ctrl Pts',(-0.0136150130812423,-0.0309023579555782,
-0.0108709063855978));
#30305=CARTESIAN_POINT('Ctrl Pts',(-0.0120043985218343,-0.0308227812232616,
-0.0105325404360109));
#30306=CARTESIAN_POINT('Ctrl Pts',(-0.0108494026557598,-0.0307432044909448,
-0.0117049697378681));
#30307=CARTESIAN_POINT('Ctrl Pts',(-0.0112119849282138,-0.0306636277586282,
-0.0133103837976729));
#30308=CARTESIAN_POINT('Ctrl Pts',(-0.0127586416654942,-0.0305840510263114,
-0.0138726106885867));
#30309=CARTESIAN_POINT('Ctrl Pts',(-0.0140677014733492,-0.0305044742939948,
-0.0128751089226279));
#30310=CARTESIAN_POINT('Ctrl Pts',(-0.0139350776945317,-0.030424897561678,
-0.0112342728780215));
#30311=CARTESIAN_POINT('Ctrl Pts',(-0.0124837849651884,-0.0303453208293614,
-0.0104599780836811));
#30312=CARTESIAN_POINT('Ctrl Pts',(-0.0110460233723964,-0.0302657440970446,
-0.0112615331792919));
#30313=CARTESIAN_POINT('Ctrl Pts',(-0.0109477359937244,-0.0301861613683264,
-0.01290723428829));
#30314=CARTESIAN_POINT('Ctrl Pts',(-0.0118298351375922,-0.0301331042170469,
-0.0135507664394204));
#30315=CARTESIAN_POINT('Ctrl Pts',(-0.0123094234768001,-0.0301065726432064,
-0.0136142973943615));
#30316=CARTESIAN_POINT('Ctrl Pts',(-0.0119101730025912,-0.0366866920838333,
-0.013396973041484));
#30317=CARTESIAN_POINT('Ctrl Pts',(-0.012317287488031,-0.0366601612926402,
-0.0135936258628881));
#30318=CARTESIAN_POINT('Ctrl Pts',(-0.0133365392569605,-0.036607104924008,
-0.013544080667975));
#30319=CARTESIAN_POINT('Ctrl Pts',(-0.0141048922962269,-0.0365275229779372,
-0.0122085437574418));
#30320=CARTESIAN_POINT('Ctrl Pts',(-0.0133938081926804,-0.0364479462456204,
-0.0108443064254199));
#30321=CARTESIAN_POINT('Ctrl Pts',(-0.011862918295578,-0.0363683695133038,
-0.0107036527840094));
#30322=CARTESIAN_POINT('Ctrl Pts',(-0.0109167446789555,-0.0362887927809871,
-0.0119168249887406));
#30323=CARTESIAN_POINT('Ctrl Pts',(-0.0114267058600925,-0.0362092160486704,
-0.0133679792940958));
#30324=CARTESIAN_POINT('Ctrl Pts',(-0.0129231601887028,-0.0361296393163537,
-0.0137232020697075));
#30325=CARTESIAN_POINT('Ctrl Pts',(-0.0140307111503216,-0.0360500625840369,
-0.0126557794384769));
#30326=CARTESIAN_POINT('Ctrl Pts',(-0.0137308835427282,-0.0359704858517202,
-0.0111471454743235));
#30327=CARTESIAN_POINT('Ctrl Pts',(-0.0122994449290827,-0.0358909091194036,
-0.0105842726373068));
#30328=CARTESIAN_POINT('Ctrl Pts',(-0.0110523725833671,-0.0358113323870868,
-0.0114846730825829));
#30329=CARTESIAN_POINT('Ctrl Pts',(-0.0111362299967622,-0.0357317556547701,
-0.0130205273559385));
#30330=CARTESIAN_POINT('Ctrl Pts',(-0.0124739045136727,-0.0356521789224534,
-0.0137798070877806));
#30331=CARTESIAN_POINT('Ctrl Pts',(-0.013835573519571,-0.0355726021901367,
-0.0130644432831712));
#30332=CARTESIAN_POINT('Ctrl Pts',(-0.013969341797967,-0.0354930254578201,
-0.0115321282859115));
#30333=CARTESIAN_POINT('Ctrl Pts',(-0.0127522277415997,-0.0354134487255034,
-0.0105916407819971));
#30334=CARTESIAN_POINT('Ctrl Pts',(-0.011303220206457,-0.0353338719931866,
-0.0111076463069289));
#30335=CARTESIAN_POINT('Ctrl Pts',(-0.0109545079925095,-0.03525429526087,
-0.0126057396377221));
#30336=CARTESIAN_POINT('Ctrl Pts',(-0.0120266897329506,-0.0351747185285532,
-0.0137086041943165));
#30337=CARTESIAN_POINT('Ctrl Pts',(-0.0135340234070985,-0.0350951417962365,
-0.0134022885795985));
#30338=CARTESIAN_POINT('Ctrl Pts',(-0.0140906968654169,-0.0350155650639198,
-0.0119684131951576));
#30339=CARTESIAN_POINT('Ctrl Pts',(-0.0131849158450631,-0.0349359883316031,
-0.0107252540262807));
#30340=CARTESIAN_POINT('Ctrl Pts',(-0.0116494370550759,-0.0348564115992864,
-0.0108157464520407));
#30341=CARTESIAN_POINT('Ctrl Pts',(-0.010895948620942,-0.0347768348669697,
-0.0121566935644407));
#30342=CARTESIAN_POINT('Ctrl Pts',(-0.0116171925481127,-0.0346972581346531,
-0.0135152557381391));
#30343=CARTESIAN_POINT('Ctrl Pts',(-0.013150071775011,-0.0346176814023364,
-0.0136423984140509));
#30344=CARTESIAN_POINT('Ctrl Pts',(-0.0140852881722481,-0.0345381046700197,
-0.0124212291905156));
#30345=CARTESIAN_POINT('Ctrl Pts',(-0.0135630227187962,-0.0344585279377029,
-0.0109744663284849));
#30346=CARTESIAN_POINT('Ctrl Pts',(-0.012063435698694,-0.0343789512053863,
-0.0106322343133662));
#30347=CARTESIAN_POINT('Ctrl Pts',(-0.0109652170589382,-0.0342993744730696,
-0.0117091743312082));
#30348=CARTESIAN_POINT('Ctrl Pts',(-0.0112780467830731,-0.0342197977407528,
-0.013215169532576));
#30349=CARTESIAN_POINT('Ctrl Pts',(-0.0127143155561136,-0.0341402210084361,
-0.0137656384185746));
#30350=CARTESIAN_POINT('Ctrl Pts',(-0.0139535469457255,-0.0340606442761194,
-0.0128544910398128));
#30351=CARTESIAN_POINT('Ctrl Pts',(-0.0138564167008781,-0.0339810675438028,
-0.011319417849904));
#30352=CARTESIAN_POINT('Ctrl Pts',(-0.0125122244022477,-0.0339014908114861,
-0.0105717340616986));
#30353=CARTESIAN_POINT('Ctrl Pts',(-0.0111567932356787,-0.0338219140791693,
-0.0112988450130191));
#30354=CARTESIAN_POINT('Ctrl Pts',(-0.0110362791746569,-0.0337423373468527,
-0.0128322596157721));
#30355=CARTESIAN_POINT('Ctrl Pts',(-0.0122614804070487,-0.033662760614536,
-0.0137621875285618));
#30356=CARTESIAN_POINT('Ctrl Pts',(-0.0137059717243087,-0.0335831838822193,
-0.013233671855001));
#30357=CARTESIAN_POINT('Ctrl Pts',(-0.0140417170534496,-0.0335036071499025,
-0.011732619205425));
#30358=CARTESIAN_POINT('Ctrl Pts',(-0.01296003893611,-0.0334240304175859,
-0.0106390669966539));
#30359=CARTESIAN_POINT('Ctrl Pts',(-0.0114554103345184,-0.0333444536852691,
-0.0109584049901842));
#30360=CARTESIAN_POINT('Ctrl Pts',(-0.0109111563233822,-0.0332648769529525,
-0.0123970402998445));
#30361=CARTESIAN_POINT('Ctrl Pts',(-0.0118276530219764,-0.0331853002206357,
-0.0136323207474776));
#30362=CARTESIAN_POINT('Ctrl Pts',(-0.0133622919203268,-0.0331057234883191,
-0.0135285544981027));
#30363=CARTESIAN_POINT('Ctrl Pts',(-0.0141041570844519,-0.0330261467560024,
-0.0121811421406199));
#30364=CARTESIAN_POINT('Ctrl Pts',(-0.0133711927017082,-0.0329465700236857,
-0.0108288673177876));
#30365=CARTESIAN_POINT('Ctrl Pts',(-0.0118372713865348,-0.032866993291369,
-0.0107149841245616));
#30366=CARTESIAN_POINT('Ctrl Pts',(-0.010912649341471,-0.0327874165590523,
-0.011944194463203));
#30367=CARTESIAN_POINT('Ctrl Pts',(-0.0114474053555292,-0.0327078398267356,
-0.0133863872340393));
#30368=CARTESIAN_POINT('Ctrl Pts',(-0.0129498955756703,-0.0326282630944189,
-0.0137156396011444));
#30369=CARTESIAN_POINT('Ctrl Pts',(-0.0140387609117777,-0.0325486863621022,
-0.0126292436039734));
#30370=CARTESIAN_POINT('Ctrl Pts',(-0.0137129206182386,-0.0324691096297855,
-0.0111260097280104));
#30371=CARTESIAN_POINT('Ctrl Pts',(-0.0122719456641281,-0.0323895328974688,
-0.010587980765354));
#30372=CARTESIAN_POINT('Ctrl Pts',(-0.0110406392495048,-0.0323099561651521,
-0.0115098096519313));
#30373=CARTESIAN_POINT('Ctrl Pts',(-0.0111510395635473,-0.0322303794328354,
-0.0130439855717105));
#30374=CARTESIAN_POINT('Ctrl Pts',(-0.0125016467932006,-0.0321508027005187,
-0.0137800182445599));
#30375=CARTESIAN_POINT('Ctrl Pts',(-0.0138507399937766,-0.032071225968202,
-0.0130412141308432));
#30376=CARTESIAN_POINT('Ctrl Pts',(-0.0139579901915926,-0.0319916492358853,
-0.011506814778101));
#30377=CARTESIAN_POINT('Ctrl Pts',(-0.0127247937218885,-0.0319120725035686,
-0.0105875158818058));
#30378=CARTESIAN_POINT('Ctrl Pts',(-0.0112849264605842,-0.0318324957712519,
-0.0111285022456082));
#30379=CARTESIAN_POINT('Ctrl Pts',(-0.0109621732017711,-0.0317529190389352,
-0.0126324019401447));
#30380=CARTESIAN_POINT('Ctrl Pts',(-0.0120532667870702,-0.0316733423066185,
-0.0137165600693672));
#30381=CARTESIAN_POINT('Ctrl Pts',(-0.013555077806628,-0.0315937655743018,
-0.0133842235287005));
#30382=CARTESIAN_POINT('Ctrl Pts',(-0.0140868717230483,-0.0315141888419851,
-0.0119409359390699));
#30383=CARTESIAN_POINT('Ctrl Pts',(-0.0131597277657927,-0.0314346121096684,
-0.0107136264340204));
#30384=CARTESIAN_POINT('Ctrl Pts',(-0.0116260437222168,-0.0313550353773517,
-0.0108306590179733));
#30385=CARTESIAN_POINT('Ctrl Pts',(-0.0108958568778532,-0.031275458645035,
-0.0121844353567568));
#30386=CARTESIAN_POINT('Ctrl Pts',(-0.0116404877210857,-0.0311958819127183,
-0.0135303227078661));
#30387=CARTESIAN_POINT('Ctrl Pts',(-0.0131753348761194,-0.0311163051804016,
-0.0136309360025271));
#30388=CARTESIAN_POINT('Ctrl Pts',(-0.0140892964206512,-0.0310367284480849,
-0.0123937801069812));
#30389=CARTESIAN_POINT('Ctrl Pts',(-0.0135420840961283,-0.0309571517157682,
-0.0109562582569936));
#30390=CARTESIAN_POINT('Ctrl Pts',(-0.0120368140274742,-0.0308775749834515,
-0.0106400236040845));
#30391=CARTESIAN_POINT('Ctrl Pts',(-0.0109573622762991,-0.0307979982511348,
-0.0117357685328693));
#30392=CARTESIAN_POINT('Ctrl Pts',(-0.0112962293497164,-0.0307184215188181,
-0.013236178247847));
#30393=CARTESIAN_POINT('Ctrl Pts',(-0.012741724846768,-0.0306388447865014,
-0.0137616319051119));
#30394=CARTESIAN_POINT('Ctrl Pts',(-0.0139651637728177,-0.0305592680541847,
-0.0128293731328584));
#30395=CARTESIAN_POINT('Ctrl Pts',(-0.013841214437156,-0.030479691321868,
-0.0112958582573798));
#30396=CARTESIAN_POINT('Ctrl Pts',(-0.012484845532147,-0.0304001145895513,
-0.0105722072935741));
#30397=CARTESIAN_POINT('Ctrl Pts',(-0.0111411227408385,-0.0303205378572346,
-0.0113213355606397));
#30398=CARTESIAN_POINT('Ctrl Pts',(-0.0110492639851992,-0.0302409551285162,
-0.0128593972941908));
#30399=CARTESIAN_POINT('Ctrl Pts',(-0.0118736682047523,-0.0301878979772368,
-0.0134608383277731));
#30400=CARTESIAN_POINT('Ctrl Pts',(-0.012321888399999,-0.0301613664033963,
-0.0135202139520323));
#30401=CARTESIAN_POINT('Ctrl Pts',(-0.0119514513259758,-0.0367414858440234,
-0.0133115144640425));
#30402=CARTESIAN_POINT('Ctrl Pts',(-0.0123300744004454,-0.0367149550528302,
-0.0134944047774705));
#30403=CARTESIAN_POINT('Ctrl Pts',(-0.013277995076846,-0.0366618986841981,
-0.0134483269426253));
#30404=CARTESIAN_POINT('Ctrl Pts',(-0.0139925758653207,-0.0365823167381272,
-0.0122062559546884));
#30405=CARTESIAN_POINT('Ctrl Pts',(-0.0133312561159133,-0.0365027400058105,
-0.0109374931092734));
#30406=CARTESIAN_POINT('Ctrl Pts',(-0.011907503682027,-0.0364231632734937,
-0.0108066829414929));
#30407=CARTESIAN_POINT('Ctrl Pts',(-0.01102754687253,-0.036343586541177,
-0.0119349527683947));
#30408=CARTESIAN_POINT('Ctrl Pts',(-0.0115018190420739,-0.0362640098088604,
-0.0132845498087204));
#30409=CARTESIAN_POINT('Ctrl Pts',(-0.0128935458387502,-0.0361844330765436,
-0.0136149127514156));
#30410=CARTESIAN_POINT('Ctrl Pts',(-0.013923586196481,-0.0361048563442269,
-0.0126221923917892));
#30411=CARTESIAN_POINT('Ctrl Pts',(-0.0136447416585,-0.0360252796119103,
-0.0112191383365156));
#30412=CARTESIAN_POINT('Ctrl Pts',(-0.0123134805312341,-0.0359457028795936,
-0.0106956574688269));
#30413=CARTESIAN_POINT('Ctrl Pts',(-0.0111536830233888,-0.0358661261472768,
-0.0115330444865743));
#30414=CARTESIAN_POINT('Ctrl Pts',(-0.0112316717779339,-0.0357865494149602,
-0.0129614138708936));
#30415=CARTESIAN_POINT('Ctrl Pts',(-0.0124757307744716,-0.0357069726826434,
-0.0136675563363033));
#30416=CARTESIAN_POINT('Ctrl Pts',(-0.0137421050349358,-0.0356273959503267,
-0.0130022563954946));
#30417=CARTESIAN_POINT('Ctrl Pts',(-0.0138665117034386,-0.03554781921801,
-0.0115771785953483));
#30418=CARTESIAN_POINT('Ctrl Pts',(-0.0127345758905823,-0.0354682424856935,
-0.0107025099628932));
#30419=CARTESIAN_POINT('Ctrl Pts',(-0.0113869753813728,-0.0353886657533766,
-0.0111824034701997));
#30420=CARTESIAN_POINT('Ctrl Pts',(-0.0110626673666204,-0.0353090890210599,
-0.0125756545654891));
#30421=CARTESIAN_POINT('Ctrl Pts',(-0.0120598137750008,-0.0352295122887433,
-0.0136013364905383));
#30422=CARTESIAN_POINT('Ctrl Pts',(-0.0134616585394798,-0.0351499355564267,
-0.0133164580007021));
#30423=CARTESIAN_POINT('Ctrl Pts',(-0.0139793738844311,-0.0350703588241098,
-0.0119829306370743));
#30424=CARTESIAN_POINT('Ctrl Pts',(-0.0131369828445936,-0.0349907820917932,
-0.010826772447157));
#30425=CARTESIAN_POINT('Ctrl Pts',(-0.011708962665897,-0.0349112053594765,
-0.0109109318708149));
#30426=CARTESIAN_POINT('Ctrl Pts',(-0.0110082062012852,-0.0348316286271599,
-0.0121580344342364));
#30427=CARTESIAN_POINT('Ctrl Pts',(-0.0116789747514459,-0.034752051894843,
-0.0134215192903648));
#30428=CARTESIAN_POINT('Ctrl Pts',(-0.0131045772943074,-0.0346724751625264,
-0.0135397640410964));
#30429=CARTESIAN_POINT('Ctrl Pts',(-0.0139743437120601,-0.0345928984302097,
-0.0124040568570029));
#30430=CARTESIAN_POINT('Ctrl Pts',(-0.0134886283696999,-0.034513321697893,
-0.0110585439301939));
#30431=CARTESIAN_POINT('Ctrl Pts',(-0.0120939881191268,-0.0344337449655762,
-0.0107402626054551));
#30432=CARTESIAN_POINT('Ctrl Pts',(-0.01107262697209,-0.0343541682332596,
-0.0117418342889929));
#30433=CARTESIAN_POINT('Ctrl Pts',(-0.0113635636893366,-0.0342745915009429,
-0.0131424342520777));
#30434=CARTESIAN_POINT('Ctrl Pts',(-0.0126993169431805,-0.0341950147686261,
-0.0136543792441393));
#30435=CARTESIAN_POINT('Ctrl Pts',(-0.0138518222346766,-0.0341154380363095,
-0.0128069974039453));
#30436=CARTESIAN_POINT('Ctrl Pts',(-0.013761489531608,-0.0340358613039928,
-0.0113793544398999));
#30437=CARTESIAN_POINT('Ctrl Pts',(-0.0125113688923585,-0.0339562845716761,
-0.0106839963901475));
#30438=CARTESIAN_POINT('Ctrl Pts',(-0.0112507959236424,-0.0338767078393595,
-0.0113602213679251));
#30439=CARTESIAN_POINT('Ctrl Pts',(-0.0111387158922684,-0.0337971311070428,
-0.0127863218190147));
#30440=CARTESIAN_POINT('Ctrl Pts',(-0.0122781729099938,-0.0337175543747259,
-0.0136511698604572));
#30441=CARTESIAN_POINT('Ctrl Pts',(-0.0136215732633237,-0.0336379776424093,
-0.0131596417120232));
#30442=CARTESIAN_POINT('Ctrl Pts',(-0.0139338218648953,-0.0335584009100925,
-0.0117636384022682));
#30443=CARTESIAN_POINT('Ctrl Pts',(-0.0129278436719772,-0.0334788241777758,
-0.0107466171117322));
#30444=CARTESIAN_POINT('Ctrl Pts',(-0.0115285146688493,-0.0333992474454591,
-0.0110436066250744));
#30445=CARTESIAN_POINT('Ctrl Pts',(-0.0110223496112091,-0.0333196707131425,
-0.0123815607963578));
#30446=CARTESIAN_POINT('Ctrl Pts',(-0.0118747064056083,-0.0332400939808259,
-0.013530391647733));
#30447=CARTESIAN_POINT('Ctrl Pts',(-0.0133019454714604,-0.0331605172485091,
-0.0134338873528243));
#30448=CARTESIAN_POINT('Ctrl Pts',(-0.0139918921064455,-0.0330809405161923,
-0.0121807720066158));
#30449=CARTESIAN_POINT('Ctrl Pts',(-0.0133102233425074,-0.0330013637838758,
-0.0109231344887676));
#30450=CARTESIAN_POINT('Ctrl Pts',(-0.0118836516406484,-0.0329217870515589,
-0.0108172212719902));
#30451=CARTESIAN_POINT('Ctrl Pts',(-0.011023738142247,-0.0328422103192422,
-0.0119604068235517));
#30452=CARTESIAN_POINT('Ctrl Pts',(-0.0115210699085561,-0.0327626335869256,
-0.0133016694914273));
#30453=CARTESIAN_POINT('Ctrl Pts',(-0.0129184101822527,-0.0326830568546089,
-0.0136078795329958));
#30454=CARTESIAN_POINT('Ctrl Pts',(-0.0139310726051947,-0.0326034801222921,
-0.0125975136353148));
#30455=CARTESIAN_POINT('Ctrl Pts',(-0.0136280358473832,-0.0325239033899755,
-0.0111994817496426));
#30456=CARTESIAN_POINT('Ctrl Pts',(-0.0122879057688142,-0.0324443266576589,
-0.0106991060880532));
#30457=CARTESIAN_POINT('Ctrl Pts',(-0.0111427708325933,-0.0323647499253422,
-0.0115564219037597));
#30458=CARTESIAN_POINT('Ctrl Pts',(-0.011245444915241,-0.0322851731930254,
-0.0129832303920315));
#30459=CARTESIAN_POINT('Ctrl Pts',(-0.0125015315443861,-0.0322055964607087,
-0.0136677527155328));
#30460=CARTESIAN_POINT('Ctrl Pts',(-0.0137562101019329,-0.0321260197283921,
-0.0129806529070748));
#30461=CARTESIAN_POINT('Ctrl Pts',(-0.0138559545253982,-0.0320464429960753,
-0.0115536366225233));
#30462=CARTESIAN_POINT('Ctrl Pts',(-0.0127090618072971,-0.0319668662637586,
-0.0106986737388134));
#30463=CARTESIAN_POINT('Ctrl Pts',(-0.0113699619010038,-0.0318872895314419,
-0.0112017998314348));
#30464=CARTESIAN_POINT('Ctrl Pts',(-0.0110697961355561,-0.0318077127991252,
-0.0126004509391794));
#30465=CARTESIAN_POINT('Ctrl Pts',(-0.0120845308663866,-0.0317281360668085,
-0.0136087355833722));
#30466=CARTESIAN_POINT('Ctrl Pts',(-0.0134812394725246,-0.0316485593344919,
-0.0132996572103688));
#30467=CARTESIAN_POINT('Ctrl Pts',(-0.0139758164399881,-0.0315689826021751,
-0.0119573763432578));
#30468=CARTESIAN_POINT('Ctrl Pts',(-0.0131135575223454,-0.0314894058698584,
-0.0108159585977663));
#30469=CARTESIAN_POINT('Ctrl Pts',(-0.0116872064869202,-0.0314098291375418,
-0.010924800799));
#30470=CARTESIAN_POINT('Ctrl Pts',(-0.0110081208787246,-0.031330252405225,
-0.0121838347510359));
#30471=CARTESIAN_POINT('Ctrl Pts',(-0.0117006396401363,-0.0312506756729083,
-0.0134355318165829));
#30472=CARTESIAN_POINT('Ctrl Pts',(-0.0131280723880818,-0.0311710989405916,
-0.0135291038124697));
#30473=CARTESIAN_POINT('Ctrl Pts',(-0.013978071448085,-0.031091522208275,
-0.0123785287641178));
#30474=CARTESIAN_POINT('Ctrl Pts',(-0.0134691551110141,-0.0310119454759582,
-0.0110416101283893));
#30475=CARTESIAN_POINT('Ctrl Pts',(-0.0120692295331141,-0.0309323687436415,
-0.0107475067721579));
#30476=CARTESIAN_POINT('Ctrl Pts',(-0.0110653218968386,-0.0308527920113249,
-0.0117665673278705));
#30477=CARTESIAN_POINT('Ctrl Pts',(-0.0113804737712188,-0.0307732152790082,
-0.0131619726980214));
#30478=CARTESIAN_POINT('Ctrl Pts',(-0.0127248080280418,-0.0306936385466914,
-0.0136506531216372));
#30479=CARTESIAN_POINT('Ctrl Pts',(-0.0138626260722862,-0.0306140618143747,
-0.012783637343089));
#30480=CARTESIAN_POINT('Ctrl Pts',(-0.0137473511797801,-0.0305344850820581,
-0.0113574436367382));
#30481=CARTESIAN_POINT('Ctrl Pts',(-0.0124859060991057,-0.0304549083497413,
-0.0106844365034671));
#30482=CARTESIAN_POINT('Ctrl Pts',(-0.0112362221092804,-0.0303753316174246,
-0.0113811379419875));
#30483=CARTESIAN_POINT('Ctrl Pts',(-0.0111507919766741,-0.0302957488887063,
-0.0128115603000916));
#30484=CARTESIAN_POINT('Ctrl Pts',(-0.0119175012719124,-0.0302426917374269,
-0.0133709102161257));
#30485=CARTESIAN_POINT('Ctrl Pts',(-0.012334353323198,-0.0302161601635864,
-0.0134261305097031));
#30486=CARTESIAN_POINT('Ctrl Pts',(-0.012333636867918,-0.0302142743898723,
-0.0134293617860453));
#30487=CARTESIAN_POINT('Ctrl Pts',(-0.0121831476494517,-0.0302142743898723,
-0.013425843584848));
#30488=CARTESIAN_POINT('Ctrl Pts',(-0.0120341035714372,-0.030214274389864,
-0.0133932994687964));
#30489=CARTESIAN_POINT('Ctrl Pts',(-0.0118942833424323,-0.030214274389864,
-0.0133373140318196));
#30490=CARTESIAN_POINT('Ctrl Pts',(-0.0117668876252743,-0.030214274389864,
-0.013286303495327));
#30491=CARTESIAN_POINT('Ctrl Pts',(-0.0116469983405503,-0.030214274389864,
-0.0132157825727993));
#30492=CARTESIAN_POINT('Ctrl Pts',(-0.0115400467092915,-0.030214274389864,
-0.0131295918764286));
#30493=CARTESIAN_POINT('Ctrl Pts',(-0.011467013779984,-0.030214274389864,
-0.0130707357471586));
#30494=CARTESIAN_POINT('Ctrl Pts',(-0.0113969920402463,-0.030214274389864,
-0.0130030912482422));
#30495=CARTESIAN_POINT('Ctrl Pts',(-0.0113289969754534,-0.030214274389864,
-0.0129177922909469));
#30496=CARTESIAN_POINT('Ctrl Pts',(-0.011293993783658,-0.0302142743898639,
-0.012873881225177));
#30497=CARTESIAN_POINT('Ctrl Pts',(-0.0112601502658924,-0.0302142743898639,
-0.0128257337008467));
#30498=CARTESIAN_POINT('Ctrl Pts',(-0.0112287294385481,-0.0302142743898639,
-0.0127729949610184));
#30499=CARTESIAN_POINT('Ctrl Pts',(-0.0111686663713541,-0.0302142743898639,
-0.0126721812415285));
#30500=CARTESIAN_POINT('Ctrl Pts',(-0.0111196338579071,-0.030214274389864,
-0.0125561133975683));
#30501=CARTESIAN_POINT('Ctrl Pts',(-0.0110871847907948,-0.030214274389864,
-0.0124384291957896));
#30502=CARTESIAN_POINT('Ctrl Pts',(-0.011026262475289,-0.030214274389864,
-0.0122174800373441));
#30503=CARTESIAN_POINT('Ctrl Pts',(-0.0110174454473768,-0.0302142743898639,
-0.0119820737242676));
#30504=CARTESIAN_POINT('Ctrl Pts',(-0.0110588114931852,-0.030214274389864,
-0.0117565343966462));
#30505=CARTESIAN_POINT('Ctrl Pts',(-0.0110777497677168,-0.030214274389864,
-0.0116532775921661));
#30506=CARTESIAN_POINT('Ctrl Pts',(-0.0111143381091383,-0.0302142743898714,
-0.0115105391820177));
#30507=CARTESIAN_POINT('Ctrl Pts',(-0.0111936560887727,-0.0302142743898722,
-0.0113546716118303));
#30508=CARTESIAN_POINT('Ctrl Pts',(-0.0111983292156988,-0.0302142743898722,
-0.0113454884613957));
#30509=CARTESIAN_POINT('Ctrl Pts',(-0.0112031507400948,-0.0302142743898723,
-0.0113362652498508));
#30510=CARTESIAN_POINT('Ctrl Pts',(-0.0112081237276435,-0.0302142743898723,
-0.0113270082871182));
#30511=CARTESIAN_POINT('Origin',(0.006,-0.0355287743898723,-0.00417585328655812));
#30512=CARTESIAN_POINT('',(0.00445,-0.0355287743898723,-0.00417585328655812));
#30513=CARTESIAN_POINT('',(0.00721995334505415,-0.0364849196904892,-0.0112310978494783));
#30514=CARTESIAN_POINT('',(0.00708453011998519,-0.0366362514743427,-0.0115256574169581));
#30515=CARTESIAN_POINT('Ctrl Pts',(0.00721995334504645,-0.0364849196904987,
-0.0112310978494762));
#30516=CARTESIAN_POINT('Ctrl Pts',(0.00719897063095221,-0.0365116917012283,
-0.011283959762924));
#30517=CARTESIAN_POINT('Ctrl Pts',(0.00717654508557251,-0.0365384837930159,
-0.0113366586152459));
#30518=CARTESIAN_POINT('Ctrl Pts',(0.00715270723066132,-0.0365650012185064,
-0.0113883725609347));
#30519=CARTESIAN_POINT('Ctrl Pts',(0.00713138418908878,-0.0365887211449947,
-0.0114346308596746));
#30520=CARTESIAN_POINT('Ctrl Pts',(0.00710860625998018,-0.0366125765485143,
-0.0114808035328048));
#30521=CARTESIAN_POINT('Ctrl Pts',(0.00708453754730291,-0.0366361489012686,
-0.0115256728563643));
#30522=CARTESIAN_POINT('',(0.00700668322306563,-0.0367087073891193,-0.0114115336377739));
#30523=CARTESIAN_POINT('Ctrl Pts',(0.00708451613677846,-0.0366361698698464,
-0.0115256340934646));
#30524=CARTESIAN_POINT('Ctrl Pts',(0.00706046816155679,-0.0366597210019003,
-0.0114855239006838));
#30525=CARTESIAN_POINT('Ctrl Pts',(0.00703434025913843,-0.0366837566058097,
-0.0114470041691646));
#30526=CARTESIAN_POINT('Ctrl Pts',(0.00700646285490531,-0.0367075587304944,
-0.0114103516394692));
#30527=CARTESIAN_POINT('',(0.00671669833332503,-0.0369031264201922,-0.0108094007648104));
#30528=CARTESIAN_POINT('Ctrl Pts',(0.00700524248433158,-0.0367085996090022,
-0.0114112785004056));
#30529=CARTESIAN_POINT('Ctrl Pts',(0.00697164972371802,-0.036737221535019,
-0.0113040197252933));
#30530=CARTESIAN_POINT('Ctrl Pts',(0.00693135743213202,-0.0367690921506772,
-0.0111983546505858));
#30531=CARTESIAN_POINT('Ctrl Pts',(0.0068368208233598,-0.0368347373794732,
-0.0109973266739168));
#30532=CARTESIAN_POINT('Ctrl Pts',(0.00678126879680362,-0.0368694541553801,
-0.0108991521238439));
#30533=CARTESIAN_POINT('Ctrl Pts',(0.00671669833068704,-0.036903126420027,
-0.0108094007666463));
#30534=CARTESIAN_POINT('',(0.00634923972919489,-0.0370392946212466,-0.010672896044278));
#30535=CARTESIAN_POINT('Ctrl Pts',(0.00671669833340338,-0.0369031264186105,
-0.0108094007630884));
#30536=CARTESIAN_POINT('Ctrl Pts',(0.00668434001035949,-0.0369200006660466,
-0.0107924289650939));
#30537=CARTESIAN_POINT('Ctrl Pts',(0.00665104602607226,-0.0369359068209843,
-0.0107764344608264));
#30538=CARTESIAN_POINT('Ctrl Pts',(0.00653214916248705,-0.0369874926958288,
-0.0107245701498326));
#30539=CARTESIAN_POINT('Ctrl Pts',(0.00644209798508761,-0.0370174454481331,
-0.010694470505926));
#30540=CARTESIAN_POINT('Ctrl Pts',(0.00634919653914119,-0.0370389272884398,
-0.0106728859625448));
#30541=CARTESIAN_POINT('Ctrl Pts',(0.00634889289767975,-0.0370389974680792,
-0.010674460128291));
#30542=CARTESIAN_POINT('Ctrl Pts',(0.00628453094295314,-0.0370538664163882,
-0.0106801749938966));
#30543=CARTESIAN_POINT('Ctrl Pts',(0.00621892219545928,-0.0370646669836523,
-0.0106815858596051));
#30544=CARTESIAN_POINT('Ctrl Pts',(0.00613401119738346,-0.0370730877719417,
-0.010679137413212));
#30545=CARTESIAN_POINT('Ctrl Pts',(0.00611502706975014,-0.0370746174397915,
-0.0106783151674329));
#30546=CARTESIAN_POINT('Ctrl Pts',(0.00609289604103467,-0.0370759913228217,
-0.0106770563132658));
#30547=CARTESIAN_POINT('Ctrl Pts',(0.00608975354297057,-0.0370761767965982,
-0.0106768705011461));
#30548=CARTESIAN_POINT('Ctrl Pts',(0.00608576149263246,-0.0370764002135845,
-0.0106766255696088));
#30549=CARTESIAN_POINT('Ctrl Pts',(0.00608491202614355,-0.0370764470527918,
-0.0106765729396212));
#30550=CARTESIAN_POINT('Ctrl Pts',(0.00608355432315204,-0.037076520794857,
-0.0106764880061428));
#30551=CARTESIAN_POINT('Ctrl Pts',(0.00608304609026255,-0.0370765481478644,
-0.0106764560302396));
#30552=CARTESIAN_POINT('Ctrl Pts',(0.00608208535556954,-0.0370765993798952,
-0.0106763952402986));
#30553=CARTESIAN_POINT('Ctrl Pts',(0.00608163285407564,-0.0370766233109422,
-0.0106763664640596));
#30554=CARTESIAN_POINT('Ctrl Pts',(0.00608061127185519,-0.037076676889254,
-0.010676301172149));
#30555=CARTESIAN_POINT('Ctrl Pts',(0.00608004219029104,-0.0370767064208356,
-0.0106762645725075));
#30556=CARTESIAN_POINT('Ctrl Pts',(0.00607834196728137,-0.0370767937111384,
-0.0106761545444927));
#30557=CARTESIAN_POINT('Ctrl Pts',(0.00607721082082661,-0.0370768505416594,
-0.0106760804435228));
#30558=CARTESIAN_POINT('Ctrl Pts',(0.00606775814820463,-0.0370773150733444,
-0.01067545370425));
#30559=CARTESIAN_POINT('Ctrl Pts',(0.00605943626584679,-0.0370776567709202,
-0.0106748533872717));
#30560=CARTESIAN_POINT('Ctrl Pts',(0.00603153518532823,-0.0370785773976582,
-0.0106726813288391));
#30561=CARTESIAN_POINT('Ctrl Pts',(0.00601195864463628,-0.0370788514854428,
-0.0106708943268714));
#30562=CARTESIAN_POINT('Ctrl Pts',(0.00593170148651683,-0.0370784586746065,
-0.0106625286154495));
#30563=CARTESIAN_POINT('Ctrl Pts',(0.00587115571686308,-0.0370745767210469,
-0.0106537962981553));
#30564=CARTESIAN_POINT('Ctrl Pts',(0.00581155370696253,-0.0370672762568326,
-0.010642763081521));
#30565=CARTESIAN_POINT('',(0.0051699690934982,-0.0368386696897961,-0.0112224559460341));
#30566=CARTESIAN_POINT('Ctrl Pts',(0.00543336738962369,-0.036971489706509,
-0.0107406611507994));
#30567=CARTESIAN_POINT('Ctrl Pts',(0.00537662766820104,-0.036949204938273,
-0.0108121501534098));
#30568=CARTESIAN_POINT('Ctrl Pts',(0.00532685230785057,-0.0369258210465427,
-0.0108903032522527));
#30569=CARTESIAN_POINT('Ctrl Pts',(0.00524052614104284,-0.0368808358599697,
-0.0110513873789148));
#30570=CARTESIAN_POINT('Ctrl Pts',(0.00520302724223552,-0.0368587245012713,
-0.0111360978982334));
#30571=CARTESIAN_POINT('Ctrl Pts',(0.00517104225064472,-0.0368384801010089,
-0.0112223933179672));
#30572=CARTESIAN_POINT('',(0.00508837275154337,-0.0367823435977278,-0.0112995565278748));
#30573=CARTESIAN_POINT('Ctrl Pts',(0.00517029079620948,-0.0368380041776274,
-0.0112216295773864));
#30574=CARTESIAN_POINT('Ctrl Pts',(0.00514776779428583,-0.0368237304862038,
-0.0112412136034523));
#30575=CARTESIAN_POINT('Ctrl Pts',(0.00512627760027647,-0.0368092952781386,
-0.0112613026366608));
#30576=CARTESIAN_POINT('Ctrl Pts',(0.00509999117843507,-0.0367907315219668,
-0.0112875890585023));
#30577=CARTESIAN_POINT('Ctrl Pts',(0.00509415983457079,-0.036786552111337,
-0.0112935361211783));
#30578=CARTESIAN_POINT('Ctrl Pts',(0.00508837275129895,-0.0367823435979441,
-0.011299556527791));
#30579=CARTESIAN_POINT('',(0.00489985734136505,-0.0366206471529012,-0.0110939405679692));
#30580=CARTESIAN_POINT('Ctrl Pts',(0.00508837275077811,-0.0367823435975653,
-0.0112995565289848));
#30581=CARTESIAN_POINT('Ctrl Pts',(0.00505343997080538,-0.0367569395961701,
-0.0112717537544348));
#30582=CARTESIAN_POINT('Ctrl Pts',(0.00502114020158271,-0.0367312295393717,
-0.0112411171694515));
#30583=CARTESIAN_POINT('Ctrl Pts',(0.00499110859515615,-0.0367054808669651,
-0.0112083991960897));
#30584=CARTESIAN_POINT('Ctrl Pts',(0.00495813976451085,-0.0366772138602703,
-0.011172481259916));
#30585=CARTESIAN_POINT('Ctrl Pts',(0.00492779975572552,-0.0366488012044239,
-0.0111339368794957));
#30586=CARTESIAN_POINT('Ctrl Pts',(0.00489985734136859,-0.0366206471529081,
-0.0110939405679709));
#30587=CARTESIAN_POINT('',(0.0048020155877565,-0.0365123054509049,-0.0112033912831791));
#30588=CARTESIAN_POINT('Origin',(0.00584908854435658,-0.0356866920263109,
-0.0120603327566456));
#30589=CARTESIAN_POINT('',(0.00473550000001,-0.036425178177226,-0.0117172854002574));
#30590=CARTESIAN_POINT('Ctrl Pts',(0.00480201558775629,-0.0365123054509075,
-0.0112033912831797));
#30591=CARTESIAN_POINT('Ctrl Pts',(0.00478601756319877,-0.0364928191481298,
-0.0112873168359884));
#30592=CARTESIAN_POINT('Ctrl Pts',(0.00477251148750761,-0.0364754056904488,
-0.0113723549961358));
#30593=CARTESIAN_POINT('Ctrl Pts',(0.00475037618306168,-0.0364459871029898,
-0.0115437515601713));
#30594=CARTESIAN_POINT('Ctrl Pts',(0.00474172253563746,-0.0364339559138146,
-0.0116302694145159));
#30595=CARTESIAN_POINT('Ctrl Pts',(0.00473550000000279,-0.0364251781772399,
-0.0117172854002583));
#30596=CARTESIAN_POINT('',(0.00473549206322617,-0.0364251864739627,-0.012361204277891));
#30597=CARTESIAN_POINT('',(0.00473550000001,-0.036425178177226,-0.00417585328655812));
#30598=CARTESIAN_POINT('',(0.0049082256814125,-0.036629014744185,-0.0132662100342696));
#30599=CARTESIAN_POINT('Ctrl Pts',(0.00473551176325926,-0.0364251947706894,
-0.0123613358119503));
#30600=CARTESIAN_POINT('Ctrl Pts',(0.00473977927981908,-0.0364312145183496,
-0.0124184833562194));
#30601=CARTESIAN_POINT('Ctrl Pts',(0.0047451967074644,-0.0364387690287892,
-0.012475379285434));
#30602=CARTESIAN_POINT('Ctrl Pts',(0.00476256626397218,-0.0364623651597535,
-0.0126256583208612));
#30603=CARTESIAN_POINT('Ctrl Pts',(0.00477650468131714,-0.0364807673113787,
-0.0127187012120098));
#30604=CARTESIAN_POINT('Ctrl Pts',(0.00482227803519832,-0.0365375236924042,
-0.0129655152140196));
#30605=CARTESIAN_POINT('Ctrl Pts',(0.00486032803510807,-0.0365814856566146,
-0.0131191817101595));
#30606=CARTESIAN_POINT('Ctrl Pts',(0.00490822568140912,-0.0366290147441883,
-0.013266210034263));
#30607=CARTESIAN_POINT('',(0.00505141064578676,-0.0367547927210949,-0.013392827911221));
#30608=CARTESIAN_POINT('Origin',(0.00581953823041687,-0.0357498950543636,
-0.0123679117387863));
#30609=CARTESIAN_POINT('',(0.00532350116102365,-0.0369233529358313,-0.013244174198489));
#30610=CARTESIAN_POINT('Ctrl Pts',(0.00505164266800161,-0.0367547916698667,
-0.0133924971879909));
#30611=CARTESIAN_POINT('Ctrl Pts',(0.00509087188926385,-0.036785136527333,
-0.0133575836405446));
#30612=CARTESIAN_POINT('Ctrl Pts',(0.00513346141989738,-0.0368151056157171,
-0.0133268047857448));
#30613=CARTESIAN_POINT('Ctrl Pts',(0.00518023319210897,-0.0368442523945079,
-0.0133013178572232));
#30614=CARTESIAN_POINT('Ctrl Pts',(0.00522512071345914,-0.0368722249641455,
-0.0132768576968728));
#30615=CARTESIAN_POINT('Ctrl Pts',(0.00527254249817658,-0.0368986332982427,
-0.0132579818935523));
#30616=CARTESIAN_POINT('Ctrl Pts',(0.00532350116101516,-0.0369233529358324,
-0.013244174198484));
#30617=CARTESIAN_POINT('',(0.00550885620308809,-0.0369996744090014,-0.0133404525414052));
#30618=CARTESIAN_POINT('Ctrl Pts',(0.0053235011610258,-0.0369233529358359,
-0.0132441741984879));
#30619=CARTESIAN_POINT('Ctrl Pts',(0.0053828710383028,-0.0369521527859156,
-0.0132817693186428));
#30620=CARTESIAN_POINT('Ctrl Pts',(0.00544487207496328,-0.0369775422367839,
-0.0133141218395921));
#30621=CARTESIAN_POINT('Ctrl Pts',(0.00550913196779272,-0.036998994987575,
-0.0133411896435628));
#30622=CARTESIAN_POINT('Ctrl Pts',(0.00550973902764092,-0.0369991975191047,
-0.0133401758005509));
#30623=CARTESIAN_POINT('Ctrl Pts',(0.00557239949470718,-0.0370200894521147,
-0.0133958926875114));
#30624=CARTESIAN_POINT('Ctrl Pts',(0.0056432881507905,-0.0370392637429235,
-0.0134441367408925));
#30625=CARTESIAN_POINT('Ctrl Pts',(0.00575851694623828,-0.0370603101471249,
-0.013493473393482));
#30626=CARTESIAN_POINT('Ctrl Pts',(0.00579699572419665,-0.0370659426799965,
-0.0135059326595814));
#30627=CARTESIAN_POINT('Ctrl Pts',(0.00585469055904418,-0.0370720537271489,
-0.0135180201626379));
#30628=CARTESIAN_POINT('Ctrl Pts',(0.00587282257791823,-0.037073656915028,
-0.0135209210756684));
#30629=CARTESIAN_POINT('Ctrl Pts',(0.00589513658530892,-0.0370752283829208,
-0.0135233528248468));
#30630=CARTESIAN_POINT('Ctrl Pts',(0.00589916799537088,-0.0370754964933055,
-0.0135237473367194));
#30631=CARTESIAN_POINT('Ctrl Pts',(0.00590423872634902,-0.037075813772681,
-0.0135241868836967));
#30632=CARTESIAN_POINT('Ctrl Pts',(0.00590527310976059,-0.0370758774539166,
-0.0135242735905519));
#30633=CARTESIAN_POINT('Ctrl Pts',(0.00590690057550275,-0.0370759760088702,
-0.0135244053545441));
#30634=CARTESIAN_POINT('Ctrl Pts',(0.00590749344823749,-0.03707601156973,
-0.0135244523834596));
#30635=CARTESIAN_POINT('Ctrl Pts',(0.00590853919498026,-0.0370760736908727,
-0.0135245336210213));
#30636=CARTESIAN_POINT('Ctrl Pts',(0.00590899202748707,-0.0370761003913174,
-0.0135245682318516));
#30637=CARTESIAN_POINT('Ctrl Pts',(0.00591002705405027,-0.0370761609637588,
-0.0135246460444136));
#30638=CARTESIAN_POINT('Ctrl Pts',(0.0059106092813878,-0.0370761947075729,
-0.0135246888786905));
#30639=CARTESIAN_POINT('Ctrl Pts',(0.00591220602721993,-0.0370762863448517,
-0.013524803778942));
#30640=CARTESIAN_POINT('Ctrl Pts',(0.00591322071215222,-0.0370763435768412,
-0.0135248739487088));
#30641=CARTESIAN_POINT('Ctrl Pts',(0.00591851083039439,-0.0370766367379395,
-0.0135252249287804));
#30642=CARTESIAN_POINT('Ctrl Pts',(0.00592278981535103,-0.0370768560956537,
-0.0135254582713297));
#30643=CARTESIAN_POINT('Ctrl Pts',(0.00594514557399332,-0.0370779091031153,
-0.0135264121346295));
#30644=CARTESIAN_POINT('Ctrl Pts',(0.00596323246802831,-0.0370784437138682,
-0.0135262796754723));
#30645=CARTESIAN_POINT('Ctrl Pts',(0.00601731944718832,-0.0370790959258226,
-0.0135231506769677));
#30646=CARTESIAN_POINT('Ctrl Pts',(0.00605283405859192,-0.037078266965631,
-0.0135174708951169));
#30647=CARTESIAN_POINT('Ctrl Pts',(0.00614970529758117,-0.0370727779032569,
-0.0134922183002785));
#30648=CARTESIAN_POINT('Ctrl Pts',(0.00622246849129482,-0.0370647759109164,
-0.0134620967630096));
#30649=CARTESIAN_POINT('Ctrl Pts',(0.00630029331254413,-0.0370494071287153,
-0.0134053749986389));
#30650=CARTESIAN_POINT('',(0.00680869722628235,-0.0368513852118003,-0.0134899528977776));
#30651=CARTESIAN_POINT('Ctrl Pts',(0.00648836437726054,-0.0369998285136294,
-0.0133422410801523));
#30652=CARTESIAN_POINT('Ctrl Pts',(0.00654817215037741,-0.0369799733734263,
-0.013360182848383));
#30653=CARTESIAN_POINT('Ctrl Pts',(0.0066053348750835,-0.036956968639739,
-0.013381036200993));
#30654=CARTESIAN_POINT('Ctrl Pts',(0.00666013990064864,-0.0369311706646718,
-0.0134061770452628));
#30655=CARTESIAN_POINT('Ctrl Pts',(0.00671261604440717,-0.0369064689473686,
-0.0134302495558493));
#30656=CARTESIAN_POINT('Ctrl Pts',(0.00676176143889012,-0.0368797672711963,
-0.0134577138102791));
#30657=CARTESIAN_POINT('Ctrl Pts',(0.00680820361295115,-0.0368513880598503,
-0.0134890451831761));
#30658=CARTESIAN_POINT('',(0.0069608110048393,-0.036745056517083,-0.0133832021230568));
#30659=CARTESIAN_POINT('Origin',(0.00617971096306188,-0.0357989913886571,
-0.0124240807529343));
#30660=CARTESIAN_POINT('',(0.00710501796773384,-0.03661664768168,-0.0127892153648441));
#30661=CARTESIAN_POINT('Ctrl Pts',(0.00696081100483564,-0.036745056517089,
-0.0133832021230525));
#30662=CARTESIAN_POINT('Ctrl Pts',(0.00699435314294245,-0.0367185596585908,
-0.013288099714129));
#30663=CARTESIAN_POINT('Ctrl Pts',(0.00702288481908988,-0.0366937839905792,
-0.0131901514676876));
#30664=CARTESIAN_POINT('Ctrl Pts',(0.00704667882519898,-0.0366719994057288,
-0.013090924388801));
#30665=CARTESIAN_POINT('Ctrl Pts',(0.00707034230680265,-0.0366503343224936,
-0.0129922416304184));
#30666=CARTESIAN_POINT('Ctrl Pts',(0.00708952955233279,-0.0366314365546728,
-0.0128914214092024));
#30667=CARTESIAN_POINT('Ctrl Pts',(0.0071042246890736,-0.036616518769789,
-0.0127897291648212));
#30668=CARTESIAN_POINT('',(0.00715706304473573,-0.036560233653124,-0.0126859173614613));
#30669=CARTESIAN_POINT('Ctrl Pts',(0.00710521494511478,-0.0366155125943608,
-0.0127902311630274));
#30670=CARTESIAN_POINT('Ctrl Pts',(0.00712399117977778,-0.0365964171258507,
-0.012756454271057));
#30671=CARTESIAN_POINT('Ctrl Pts',(0.00714131329460908,-0.0365778042956974,
-0.0127216438762269));
#30672=CARTESIAN_POINT('Ctrl Pts',(0.00715705640924412,-0.0365601426392513,
-0.0126859324135836));
#30673=CARTESIAN_POINT('',(0.0072645000000106,-0.0364251781772283,-0.012945467333915));
#30674=CARTESIAN_POINT('Ctrl Pts',(0.0071570835597271,-0.0365601121792552,
-0.0126858905925983));
#30675=CARTESIAN_POINT('Ctrl Pts',(0.00717621068139738,-0.0365386529849375,
-0.0127267486831773));
#30676=CARTESIAN_POINT('Ctrl Pts',(0.00719440998528269,-0.036517030430569,
-0.0127682118485989));
#30677=CARTESIAN_POINT('Ctrl Pts',(0.00721166125580552,-0.0364954061714623,
-0.0128098344234972));
#30678=CARTESIAN_POINT('Ctrl Pts',(0.00723023900793353,-0.0364721191836949,
-0.0128546574339745));
#30679=CARTESIAN_POINT('Ctrl Pts',(0.007247849025769,-0.0364486666510824,
-0.0128999824936057));
#30680=CARTESIAN_POINT('Ctrl Pts',(0.00726450000000412,-0.0364251781772302,
-0.0129454673339182));
#30681=CARTESIAN_POINT('',(0.007264500000004,-0.0364251781772306,-0.0112916085523411));
#30682=CARTESIAN_POINT('',(0.00726450000001,-0.036425178177226,-0.00417585328655812));
#30683=CARTESIAN_POINT('Origin',(0.00607243076165687,-0.0356158716997798,
-0.0121519018301174));
#30684=CARTESIAN_POINT('Origin',(0.008,-0.0301787743898723,-0.00457585328655812));
#30685=CARTESIAN_POINT('',(0.00760000000001,-0.0297787743898623,-0.00457585328656812));
#30686=CARTESIAN_POINT('Origin',(-0.0146,-0.0301787743898723,-0.00417585328655812));
#30687=CARTESIAN_POINT('',(-0.015,-0.0301787743898623,-0.00457585328656812));
#30688=CARTESIAN_POINT('Ctrl Pts',(0.0007247979407562,-0.0405744211147313,
-0.0150948585672975));
#30689=CARTESIAN_POINT('Ctrl Pts',(-0.000237867174816089,-0.0405219330120263,
-0.015333921225633));
#30690=CARTESIAN_POINT('Ctrl Pts',(-0.00240155359114006,-0.0404169768530862,
-0.0147817233443831));
#30691=CARTESIAN_POINT('Ctrl Pts',(-0.00349898809073308,-0.0402595526379108,
-0.0115953997864184));
#30692=CARTESIAN_POINT('Ctrl Pts',(-0.00143658133088921,-0.0401021484692049,
-0.00893630820182674));
#30693=CARTESIAN_POINT('Ctrl Pts',(0.0019164823364414,-0.0399447443004989,
-0.0091940107250774));
#30694=CARTESIAN_POINT('Ctrl Pts',(0.00354474713388061,-0.0397873401317929,
-0.0121391462709199));
#30695=CARTESIAN_POINT('Ctrl Pts',(0.00197842869696902,-0.0396299359630869,
-0.0151168671994064));
#30696=CARTESIAN_POINT('Ctrl Pts',(-0.00136986320203818,-0.0394725317943809,
-0.0154451367971516));
#30697=CARTESIAN_POINT('Ctrl Pts',(-0.00348423018666191,-0.0393151276256749,
-0.0128278237290509));
#30698=CARTESIAN_POINT('Ctrl Pts',(-0.00245935806117728,-0.0391577234569689,
-0.00962318496292607));
#30699=CARTESIAN_POINT('Ctrl Pts',(0.00078120175765321,-0.0390003192882629,
-0.00871833392572952));
#30700=CARTESIAN_POINT('Ctrl Pts',(0.00331797335358058,-0.038842915119557,
-0.0109285455423723));
#30701=CARTESIAN_POINT('Ctrl Pts',(0.00286540590808132,-0.038685510950851,
-0.0142625077104432));
#30702=CARTESIAN_POINT('Ctrl Pts',(-0.000168734413497188,-0.038528106782145,
-0.0157165072437804));
#30703=CARTESIAN_POINT('Ctrl Pts',(-0.00305085839970424,-0.038370702613439,
-0.0139805591784971));
#30704=CARTESIAN_POINT('Ctrl Pts',(-0.00318431512310994,-0.038213298444733,
-0.0106186660841466));
#30705=CARTESIAN_POINT('Ctrl Pts',(-0.000448870589781203,-0.0380558942760271,
-0.0086597171282114));
#30706=CARTESIAN_POINT('Ctrl Pts',(0.00269098364593626,-0.037898490107321,
-0.00986862447417986));
#30707=CARTESIAN_POINT('Ctrl Pts',(0.00340640111752454,-0.037741085938615,
-0.0131562249345524));
#30708=CARTESIAN_POINT('Ctrl Pts',(0.00105282834073001,-0.0375836817699092,
-0.0155605615635386));
#30709=CARTESIAN_POINT('Ctrl Pts',(-0.00224928815150608,-0.0374262776012032,
-0.0149154518584878));
#30710=CARTESIAN_POINT('Ctrl Pts',(-0.00352491284701288,-0.0372688734324972,
-0.0118021062096773));
#30711=CARTESIAN_POINT('Ctrl Pts',(-0.00162477424132635,-0.0371114692637911,
-0.00902548724613536));
#30712=CARTESIAN_POINT('Ctrl Pts',(0.00173920154528507,-0.0369540650950852,
-0.00908718440036995));
#30713=CARTESIAN_POINT('Ctrl Pts',(0.0035362471012298,-0.0367966609263792,
-0.0119316117332855));
#30714=CARTESIAN_POINT('Ctrl Pts',(0.0021473177625627,-0.0366392567576732,
-0.0149960880166491));
#30715=CARTESIAN_POINT('Ctrl Pts',(-0.00117623330881229,-0.0364818525889673,
-0.0155196793445491));
#30716=CARTESIAN_POINT('Ctrl Pts',(-0.00344005928429201,-0.0363244484202613,
-0.0130306571371357));
#30717=CARTESIAN_POINT('Ctrl Pts',(-0.00260457058776481,-0.0361670442515553,
-0.00977150107506731));
#30718=CARTESIAN_POINT('Ctrl Pts',(0.000577500877143375,-0.0360096400828493,
-0.0086785414274407));
#30719=CARTESIAN_POINT('Ctrl Pts',(0.00323927405812123,-0.0358522359141433,
-0.0107364780472958));
#30720=CARTESIAN_POINT('Ctrl Pts',(0.00298262962287774,-0.0356948317454372,
-0.0140912169689667));
#30721=CARTESIAN_POINT('Ctrl Pts',(3.8790872444014E-5,-0.0355374275767314,
-0.0157203127335408));
#30722=CARTESIAN_POINT('Ctrl Pts',(-0.00293999643850483,-0.0353800234080254,
-0.014156034703666));
#30723=CARTESIAN_POINT('Ctrl Pts',(-0.00326999971823222,-0.0352226192393194,
-0.0108077161056251));
#30724=CARTESIAN_POINT('Ctrl Pts',(-0.000653903158401233,-0.0350652150706134,
-0.00869201802027602));
#30725=CARTESIAN_POINT('Ctrl Pts',(0.00255132617086471,-0.0349078109019074,
-0.00971507449258273));
#30726=CARTESIAN_POINT('Ctrl Pts',(0.0034579431850454,-0.0347504067332014,
-0.0129551647981007));
#30727=CARTESIAN_POINT('Ctrl Pts',(0.00124913306147382,-0.0345930025644954,
-0.0154931359242426));
#30728=CARTESIAN_POINT('Ctrl Pts',(-0.00208508104655071,-0.0344355983957894,
-0.0150424077569494));
#30729=CARTESIAN_POINT('Ctrl Pts',(-0.00354074547073748,-0.0342781942270835,
-0.0120090629561708));
#30730=CARTESIAN_POINT('Ctrl Pts',(-0.00180638220017174,-0.0341207900583776,
-0.00912598757588634));
#30731=CARTESIAN_POINT('Ctrl Pts',(0.0015554375747254,-0.0339633858896715,
-0.00899068273407062));
#30732=CARTESIAN_POINT('Ctrl Pts',(0.00351588891379242,-0.0338059817209656,
-0.0117250510577476));
#30733=CARTESIAN_POINT('Ctrl Pts',(0.002308707024885,-0.0336485775522596,
-0.0148655687728454));
#30734=CARTESIAN_POINT('Ctrl Pts',(-0.000978499935992214,-0.0334911733835535,
-0.0155827925774432));
#30735=CARTESIAN_POINT('Ctrl Pts',(-0.00338412929443487,-0.0333337692148475,
-0.0132305411277567));
#30736=CARTESIAN_POINT('Ctrl Pts',(-0.00274083399948854,-0.0331763650461416,
-0.00992807068529279));
#30737=CARTESIAN_POINT('Ctrl Pts',(0.000371810325715763,-0.0330189608774355,
-0.00865073566818646));
#30738=CARTESIAN_POINT('Ctrl Pts',(0.00314947285033218,-0.0328615567087297,
-0.0105493482787621));
#30739=CARTESIAN_POINT('Ctrl Pts',(0.00308962401220603,-0.0327041525400237,
-0.013913357748021));
#30740=CARTESIAN_POINT('Ctrl Pts',(0.000246184412511208,-0.0325467483713177,
-0.0157119652787973));
#30741=CARTESIAN_POINT('Ctrl Pts',(-0.0028190544326237,-0.0323893442026117,
-0.0143247209970861));
#30742=CARTESIAN_POINT('Ctrl Pts',(-0.00334447194084124,-0.0322319400339057,
-0.0110014559159814));
#30743=CARTESIAN_POINT('Ctrl Pts',(-0.000856693556614904,-0.0320745358651996,
-0.00873626699561545));
#30744=CARTESIAN_POINT('Ctrl Pts',(0.00240292033326581,-0.0319171316964937,
-0.00956995657798453));
#30745=CARTESIAN_POINT('Ctrl Pts',(0.00349762956160217,-0.0317597275277878,
-0.0127514432156497));
#30746=CARTESIAN_POINT('Ctrl Pts',(0.00144115296983182,-0.0316023233590818,
-0.015414315230305));
#30747=CARTESIAN_POINT('Ctrl Pts',(-0.00191372110484731,-0.0314449191903758,
-0.0151595752884196));
#30748=CARTESIAN_POINT('Ctrl Pts',(-0.00354444447940972,-0.0312875150216698,
-0.0122165128157948));
#30749=CARTESIAN_POINT('Ctrl Pts',(-0.00198178305265353,-0.0311301108529639,
-0.00923709863930153));
#30750=CARTESIAN_POINT('Ctrl Pts',(0.00136631424027315,-0.0309727066842579,
-0.00890480375391904));
#30751=CARTESIAN_POINT('Ctrl Pts',(0.00348352636012016,-0.0308153025155519,
-0.0115206176757296));
#30752=CARTESIAN_POINT('Ctrl Pts',(0.00246208004358717,-0.0306578983468459,
-0.014724692264453));
#30753=CARTESIAN_POINT('Ctrl Pts',(-0.000777205389354121,-0.0305004941781399,
-0.0156364595495813));
#30754=CARTESIAN_POINT('Ctrl Pts',(-0.00331711149080357,-0.030343090009434,
-0.0134221865174339));
#30755=CARTESIAN_POINT('Ctrl Pts',(-0.00301603592565593,-0.0302381538969633,
-0.0112101605671168));
#30756=CARTESIAN_POINT('Ctrl Pts',(-0.0024332353179461,-0.030185685840728,
-0.0104080043474256));
#30757=CARTESIAN_POINT('Ctrl Pts',(0.000683754430426,-0.0406727527782625,
-0.0149295625355936));
#30758=CARTESIAN_POINT('Ctrl Pts',(-0.00022439734647116,-0.0406202646755577,
-0.0151550876683166));
#30759=CARTESIAN_POINT('Ctrl Pts',(-0.00226555956565516,-0.0405153085166175,
-0.0146341593839695));
#30760=CARTESIAN_POINT('Ctrl Pts',(-0.00330084907050131,-0.040357884301442,
-0.0116282694289622));
#30761=CARTESIAN_POINT('Ctrl Pts',(-0.00135523129196235,-0.0402004801327361,
-0.00911975560788823));
#30762=CARTESIAN_POINT('Ctrl Pts',(0.00180795669343061,-0.0400430759640301,
-0.00936286507619158));
#30763=CARTESIAN_POINT('Ctrl Pts',(0.00334401689248984,-0.039885671795324,
-0.0121412248982046));
#30764=CARTESIAN_POINT('Ctrl Pts',(0.00186639518515057,-0.0397282676266182,
-0.0149503248734341));
#30765=CARTESIAN_POINT('Ctrl Pts',(-0.00129229124532808,-0.0395708634579122,
-0.0152600053777664));
#30766=CARTESIAN_POINT('Ctrl Pts',(-0.00328692686994726,-0.0394134592892061,
-0.0127909042593799));
#30767=CARTESIAN_POINT('Ctrl Pts',(-0.00232009071187387,-0.0392560551205001,
-0.00976773624103997));
#30768=CARTESIAN_POINT('Ctrl Pts',(0.000736964239018967,-0.0390986509517941,
-0.00891412467460375));
#30769=CARTESIAN_POINT('Ctrl Pts',(0.0031300847491082,-0.0389412467830881,
-0.0109991774873666));
#30770=CARTESIAN_POINT('Ctrl Pts',(0.00270314507595757,-0.0387838426143821,
-0.0141443456440431));
#30771=CARTESIAN_POINT('Ctrl Pts',(-0.000159179402018772,-0.0386264384456762,
-0.0155160087888353));
#30772=CARTESIAN_POINT('Ctrl Pts',(-0.00287809585278843,-0.0384690342769703,
-0.0138783631584014));
#30773=CARTESIAN_POINT('Ctrl Pts',(-0.00300399525283862,-0.0383116301082643,
-0.010706845734549));
#30774=CARTESIAN_POINT('Ctrl Pts',(-0.000423452161205861,-0.0381542259395583,
-0.00885882720099533));
#30775=CARTESIAN_POINT('Ctrl Pts',(0.00253859991405746,-0.0379968217708523,
-0.00999927712131107));
#30776=CARTESIAN_POINT('Ctrl Pts',(0.00321350506802662,-0.0378394176021462,
-0.0131007089188475));
#30777=CARTESIAN_POINT('Ctrl Pts',(0.000993209282163632,-0.0376820134334403,
-0.0153688939258157));
#30778=CARTESIAN_POINT('Ctrl Pts',(-0.00212191654034275,-0.0375246092647344,
-0.0147603151838852));
#30779=CARTESIAN_POINT('Ctrl Pts',(-0.00332530577211061,-0.0373672050960284,
-0.0118232705799774));
#30780=CARTESIAN_POINT('Ctrl Pts',(-0.00153276730448458,-0.0372098009273224,
-0.00920388466402705));
#30781=CARTESIAN_POINT('Ctrl Pts',(0.00164071487392983,-0.0370523967586164,
-0.00926208806138846));
#30782=CARTESIAN_POINT('Ctrl Pts',(0.00333599819561317,-0.0368949925899104,
-0.0119454425268779));
#30783=CARTESIAN_POINT('Ctrl Pts',(0.00202572048170102,-0.0367375884212043,
-0.0148363851163382));
#30784=CARTESIAN_POINT('Ctrl Pts',(-0.00110962613287212,-0.0365801842524984,
-0.0153303267655248));
#30785=CARTESIAN_POINT('Ctrl Pts',(-0.00324525725626169,-0.0364227800837924,
-0.0129822517144672));
#30786=CARTESIAN_POINT('Ctrl Pts',(-0.00245708021311881,-0.0362653759150866,
-0.00990765357948378));
#30787=CARTESIAN_POINT('Ctrl Pts',(0.000544798434319117,-0.0361079717463805,
-0.008876585526832));
#30788=CARTESIAN_POINT('Ctrl Pts',(0.00305584199962463,-0.0359505675776744,
-0.0108179862983266));
#30789=CARTESIAN_POINT('Ctrl Pts',(0.00281373070242807,-0.0357931634089685,
-0.0139827546725603));
#30790=CARTESIAN_POINT('Ctrl Pts',(3.65942415151312E-5,-0.0356357592402625,
-0.0155195987831459));
#30791=CARTESIAN_POINT('Ctrl Pts',(-0.00277351172958201,-0.0354783550715565,
-0.0140439019396519));
#30792=CARTESIAN_POINT('Ctrl Pts',(-0.00308482774178444,-0.0353209509028505,
-0.0108851903220393));
#30793=CARTESIAN_POINT('Ctrl Pts',(-0.000616874243820103,-0.0351635467341445,
-0.00888929897362878));
#30794=CARTESIAN_POINT('Ctrl Pts',(0.00240685089553428,-0.0350061425654386,
-0.00985442229446193));
#30795=CARTESIAN_POINT('Ctrl Pts',(0.00326212843605663,-0.0348487383967326,
-0.012911034319417));
#30796=CARTESIAN_POINT('Ctrl Pts',(0.00117839775328719,-0.0346913342280267,
-0.0153052864332988));
#30797=CARTESIAN_POINT('Ctrl Pts',(-0.00196700807660791,-0.0345339300593206,
-0.0148800818845899));
#30798=CARTESIAN_POINT('Ctrl Pts',(-0.00334024183360881,-0.0343765258906146,
-0.0120185078790428));
#30799=CARTESIAN_POINT('Ctrl Pts',(-0.00170409125489704,-0.0342191217219087,
-0.00929869390928347));
#30800=CARTESIAN_POINT('Ctrl Pts',(0.00146735700140084,-0.0340617175532028,
-0.00917105104518666));
#30801=CARTESIAN_POINT('Ctrl Pts',(0.00331679284185456,-0.0339043133844968,
-0.0117505788702519));
#30802=CARTESIAN_POINT('Ctrl Pts',(0.00217797067024458,-0.0337469092157907,
-0.0147132568537032));
#30803=CARTESIAN_POINT('Ctrl Pts',(-0.000923089910697239,-0.0335895050470848,
-0.0153898660525223));
#30804=CARTESIAN_POINT('Ctrl Pts',(-0.00319249444305807,-0.0334321008783788,
-0.0131708167702892));
#30805=CARTESIAN_POINT('Ctrl Pts',(-0.0025856273656865,-0.0332746967096728,
-0.0100553570408789));
#30806=CARTESIAN_POINT('Ctrl Pts',(0.000350755628832307,-0.0331172925409668,
-0.00885035433878307));
#30807=CARTESIAN_POINT('Ctrl Pts',(0.00297112601158075,-0.032959888372261,
-0.0106414532246178));
#30808=CARTESIAN_POINT('Ctrl Pts',(0.00291466626476923,-0.0328024842035548,
-0.0138149671783149));
#30809=CARTESIAN_POINT('Ctrl Pts',(0.00023224359961718,-0.032645080034849,
-0.015511724024068));
#30810=CARTESIAN_POINT('Ctrl Pts',(-0.00265941836963197,-0.0324876758661428,
-0.0142030359465141));
#30811=CARTESIAN_POINT('Ctrl Pts',(-0.00315508278707255,-0.0323302716974368,
-0.0110679591272914));
#30812=CARTESIAN_POINT('Ctrl Pts',(-0.000808181124578904,-0.0321728675287309,
-0.00893104223920506));
#30813=CARTESIAN_POINT('Ctrl Pts',(0.00226684891256305,-0.0320154633600249,
-0.00971752204756393));
#30814=CARTESIAN_POINT('Ctrl Pts',(0.00329956747150683,-0.0318580591913191,
-0.0127188489850756));
#30815=CARTESIAN_POINT('Ctrl Pts',(0.00135954405032654,-0.0317006550226131,
-0.015230929159832));
#30816=CARTESIAN_POINT('Ctrl Pts',(-0.00180535182353563,-0.0315432508539071,
-0.0149906145092565));
#30817=CARTESIAN_POINT('Ctrl Pts',(-0.00334373137659125,-0.0313858466852011,
-0.0122142103674649));
#30818=CARTESIAN_POINT('Ctrl Pts',(-0.00186955959198933,-0.031228442516495,
-0.00940351302866479));
#30819=CARTESIAN_POINT('Ctrl Pts',(0.00128894325246858,-0.031071038347789,
-0.00909003517875381));
#30820=CARTESIAN_POINT('Ctrl Pts',(0.00328626289935744,-0.0309136341790831,
-0.0115577220437879));
#30821=CARTESIAN_POINT('Ctrl Pts',(0.0023226585551687,-0.0307562300103771,
-0.0145803578326937));
#30822=CARTESIAN_POINT('Ctrl Pts',(-0.000733194175148143,-0.0305988258416712,
-0.0154404939970894));
#30823=CARTESIAN_POINT('Ctrl Pts',(-0.00312927169148336,-0.0304414216729651,
-0.0133516097567121));
#30824=CARTESIAN_POINT('Ctrl Pts',(-0.00284524528910707,-0.0303364855604945,
-0.0112648453514926));
#30825=CARTESIAN_POINT('Ctrl Pts',(-0.00229544723482355,-0.0302840175042591,
-0.0105081132496665));
#30826=CARTESIAN_POINT('Ctrl Pts',(0.000642710920095802,-0.0407710844417939,
-0.0147642665038899));
#30827=CARTESIAN_POINT('Ctrl Pts',(-0.000210927518126123,-0.040718596339089,
-0.0149762541110002));
#30828=CARTESIAN_POINT('Ctrl Pts',(-0.00212956554017036,-0.0406136401801488,
-0.0144865954235559));
#30829=CARTESIAN_POINT('Ctrl Pts',(-0.00310271005026966,-0.0404562159649733,
-0.0116611390715061));
#30830=CARTESIAN_POINT('Ctrl Pts',(-0.00127388125303559,-0.0402988117962673,
-0.00930320301394971));
#30831=CARTESIAN_POINT('Ctrl Pts',(0.00169943105041994,-0.0401414076275612,
-0.00953171942730572));
#30832=CARTESIAN_POINT('Ctrl Pts',(0.00314328665109908,-0.0399840034588552,
-0.0121433035254893));
#30833=CARTESIAN_POINT('Ctrl Pts',(0.00175436167333222,-0.0398265992901494,
-0.0147837825474619));
#30834=CARTESIAN_POINT('Ctrl Pts',(-0.00121471928861808,-0.0396691951214434,
-0.0150748739583816));
#30835=CARTESIAN_POINT('Ctrl Pts',(-0.0030896235532325,-0.0395117909527374,
-0.0127539847897086));
#30836=CARTESIAN_POINT('Ctrl Pts',(-0.00218082336257045,-0.0393543867840314,
-0.00991228751915392));
#30837=CARTESIAN_POINT('Ctrl Pts',(0.000692726720384725,-0.0391969826153254,
-0.00910991542347796));
#30838=CARTESIAN_POINT('Ctrl Pts',(0.00294219614463583,-0.0390395784466194,
-0.011069809432361));
#30839=CARTESIAN_POINT('Ctrl Pts',(0.00254088424383383,-0.0388821742779135,
-0.0140261835776428));
#30840=CARTESIAN_POINT('Ctrl Pts',(-0.000149624390540353,-0.0387247701092075,
-0.0153155103338901));
#30841=CARTESIAN_POINT('Ctrl Pts',(-0.00270533330587274,-0.0385673659405015,
-0.0137761671383057));
#30842=CARTESIAN_POINT('Ctrl Pts',(-0.0028236753825673,-0.0384099617717955,
-0.0107950253849515));
#30843=CARTESIAN_POINT('Ctrl Pts',(-0.000398033732630625,-0.0382525576030895,
-0.00905793727377927));
#30844=CARTESIAN_POINT('Ctrl Pts',(0.00238621618217868,-0.0380951534343835,
-0.0101299297684424));
#30845=CARTESIAN_POINT('Ctrl Pts',(0.00302060901852883,-0.0379377492656776,
-0.0130451929031425));
#30846=CARTESIAN_POINT('Ctrl Pts',(0.000933590223597251,-0.0377803450969715,
-0.0151772262880931));
#30847=CARTESIAN_POINT('Ctrl Pts',(-0.00199454492917932,-0.0376229409282657,
-0.0146051785092827));
#30848=CARTESIAN_POINT('Ctrl Pts',(-0.00312569869720836,-0.0374655367595595,
-0.0118444349502773));
#30849=CARTESIAN_POINT('Ctrl Pts',(-0.00144076036764282,-0.0373081325908537,
-0.00938228208191872));
#30850=CARTESIAN_POINT('Ctrl Pts',(0.00154222820257447,-0.0371507284221477,
-0.00943699172240697));
#30851=CARTESIAN_POINT('Ctrl Pts',(0.00313574928999666,-0.0369933242534416,
-0.0119592733204704));
#30852=CARTESIAN_POINT('Ctrl Pts',(0.00190412320083946,-0.0368359200847357,
-0.0146766822160272));
#30853=CARTESIAN_POINT('Ctrl Pts',(-0.00104301895693193,-0.0366785159160298,
-0.0151409741865006));
#30854=CARTESIAN_POINT('Ctrl Pts',(-0.00305045522823148,-0.0365211117473236,
-0.0129338462917988));
#30855=CARTESIAN_POINT('Ctrl Pts',(-0.0023095898384728,-0.0363637075786177,
-0.0100438060839003));
#30856=CARTESIAN_POINT('Ctrl Pts',(0.000512095991494752,-0.0362063034099118,
-0.00907462962622331));
#30857=CARTESIAN_POINT('Ctrl Pts',(0.00287240994112814,-0.0360488992412058,
-0.0108994945493574));
#30858=CARTESIAN_POINT('Ctrl Pts',(0.00264483178197851,-0.0358914950724998,
-0.0138742923761538));
#30859=CARTESIAN_POINT('Ctrl Pts',(3.43976105861402E-5,-0.0357340909037938,
-0.0153188848327509));
#30860=CARTESIAN_POINT('Ctrl Pts',(-0.00260702702065921,-0.0355766867350878,
-0.0139317691756377));
#30861=CARTESIAN_POINT('Ctrl Pts',(-0.00289965576533666,-0.0354192825663817,
-0.0109626645384537));
#30862=CARTESIAN_POINT('Ctrl Pts',(-0.00057984532923908,-0.0352618783976759,
-0.00908657992698152));
#30863=CARTESIAN_POINT('Ctrl Pts',(0.00226237562020386,-0.0351044742289698,
-0.00999377009634113));
#30864=CARTESIAN_POINT('Ctrl Pts',(0.00306631368706786,-0.0349470700602639,
-0.0128669038407335));
#30865=CARTESIAN_POINT('Ctrl Pts',(0.00110766244510046,-0.0347896658915579,
-0.0151174369423551));
#30866=CARTESIAN_POINT('Ctrl Pts',(-0.00184893510666519,-0.0346322617228519,
-0.0147177560122302));
#30867=CARTESIAN_POINT('Ctrl Pts',(-0.00313973819648023,-0.0344748575541459,
-0.0120279528019148));
#30868=CARTESIAN_POINT('Ctrl Pts',(-0.00160180030962234,-0.0343174533854399,
-0.00947140024268058));
#30869=CARTESIAN_POINT('Ctrl Pts',(0.00137927642807616,-0.0341600492167341,
-0.00935141935630271));
#30870=CARTESIAN_POINT('Ctrl Pts',(0.0031176967699168,-0.0340026450480281,
-0.0117761066827561));
#30871=CARTESIAN_POINT('Ctrl Pts',(0.00204723431560415,-0.033845240879322,
-0.0145609449345611));
#30872=CARTESIAN_POINT('Ctrl Pts',(-0.000867679885402264,-0.0336878367106161,
-0.0151969395276014));
#30873=CARTESIAN_POINT('Ctrl Pts',(-0.00300085959168136,-0.0335304325419101,
-0.0131110924128218));
#30874=CARTESIAN_POINT('Ctrl Pts',(-0.00243042073188435,-0.033373028373204,
-0.0101826433964649));
#30875=CARTESIAN_POINT('Ctrl Pts',(0.000329700931948742,-0.0332156242044981,
-0.00904997300937973));
#30876=CARTESIAN_POINT('Ctrl Pts',(0.00279277917282932,-0.0330582200357922,
-0.0107335581704735));
#30877=CARTESIAN_POINT('Ctrl Pts',(0.00273970851733244,-0.032900815867086,
-0.0137165766086087));
#30878=CARTESIAN_POINT('Ctrl Pts',(0.000218302786723153,-0.0327434116983802,
-0.0153114827693384));
#30879=CARTESIAN_POINT('Ctrl Pts',(-0.00249978230664013,-0.0325860075296742,
-0.0140813508959422));
#30880=CARTESIAN_POINT('Ctrl Pts',(-0.00296569363330397,-0.0324286033609682,
-0.0111344623386012));
#30881=CARTESIAN_POINT('Ctrl Pts',(-0.000759668692542901,-0.0322711991922623,
-0.00912581748279469));
#30882=CARTESIAN_POINT('Ctrl Pts',(0.00213077749186029,-0.0321137950235563,
-0.00986508751714331));
#30883=CARTESIAN_POINT('Ctrl Pts',(0.00310150538141159,-0.0319563908548502,
-0.0126862547545015));
#30884=CARTESIAN_POINT('Ctrl Pts',(0.00127793513082136,-0.0317989866861443,
-0.0150475430893589));
#30885=CARTESIAN_POINT('Ctrl Pts',(-0.00169698254222384,-0.0316415825174383,
-0.0148216537300935));
#30886=CARTESIAN_POINT('Ctrl Pts',(-0.00314301827377279,-0.0314841783487323,
-0.0122119079191349));
#30887=CARTESIAN_POINT('Ctrl Pts',(-0.00175733613132536,-0.0313267741800263,
-0.00956992741802806));
#30888=CARTESIAN_POINT('Ctrl Pts',(0.00121157226466413,-0.0311693700113203,
-0.00927526660358858));
#30889=CARTESIAN_POINT('Ctrl Pts',(0.00308899943859484,-0.0310119658426143,
-0.0115948264118463));
#30890=CARTESIAN_POINT('Ctrl Pts',(0.00218323706675035,-0.0308545616739084,
-0.0144360234009344));
#30891=CARTESIAN_POINT('Ctrl Pts',(-0.000689182960942163,-0.0306971575052024,
-0.0152445284445975));
#30892=CARTESIAN_POINT('Ctrl Pts',(-0.00294143189216317,-0.0305397533364964,
-0.0132810329959904));
#30893=CARTESIAN_POINT('Ctrl Pts',(-0.00267445465255833,-0.0304348172240258,
-0.0113195301358683));
#30894=CARTESIAN_POINT('Ctrl Pts',(-0.0021576591517009,-0.0303823491677905,
-0.0106082221519074));
#30895=CARTESIAN_POINT('Ctrl Pts',(0.000601667409765497,-0.0408694161053251,
-0.0145989704721862));
#30896=CARTESIAN_POINT('Ctrl Pts',(-0.000197457689781191,-0.0408169280026203,
-0.0147974205536838));
#30897=CARTESIAN_POINT('Ctrl Pts',(-0.00199357151468546,-0.0407119718436801,
-0.0143390314631424));
#30898=CARTESIAN_POINT('Ctrl Pts',(-0.00290457103003801,-0.0405545476285045,
-0.01169400871405));
#30899=CARTESIAN_POINT('Ctrl Pts',(-0.00119253121410882,-0.0403971434597985,
-0.0094866504200112));
#30900=CARTESIAN_POINT('Ctrl Pts',(0.00159090540740915,-0.0402397392910926,
-0.0097005737784199));
#30901=CARTESIAN_POINT('Ctrl Pts',(0.00294255640970842,-0.0400823351223866,
-0.012145382152774));
#30902=CARTESIAN_POINT('Ctrl Pts',(0.00164232816151378,-0.0399249309536806,
-0.0146172402214899));
#30903=CARTESIAN_POINT('Ctrl Pts',(-0.00113714733190809,-0.0397675267849747,
-0.0148897425389965));
#30904=CARTESIAN_POINT('Ctrl Pts',(-0.00289232023651785,-0.0396101226162687,
-0.0127170653200376));
#30905=CARTESIAN_POINT('Ctrl Pts',(-0.00204155601326713,-0.0394527184475627,
-0.0100568387972678));
#30906=CARTESIAN_POINT('Ctrl Pts',(0.00064848920175059,-0.0392953142788567,
-0.00930570617235219));
#30907=CARTESIAN_POINT('Ctrl Pts',(0.00275430754016345,-0.0391379101101507,
-0.0111404413773551));
#30908=CARTESIAN_POINT('Ctrl Pts',(0.0023786234117102,-0.0389805059414447,
-0.0139080215112426));
#30909=CARTESIAN_POINT('Ctrl Pts',(-0.000140069379062041,-0.0388231017727388,
-0.015115011878945));
#30910=CARTESIAN_POINT('Ctrl Pts',(-0.00253257075895693,-0.0386656976040327,
-0.0136739711182101));
#30911=CARTESIAN_POINT('Ctrl Pts',(-0.00264335551229598,-0.0385082934353268,
-0.0108832050353539));
#30912=CARTESIAN_POINT('Ctrl Pts',(-0.000372615304055287,-0.0383508892666208,
-0.00925704734656319));
#30913=CARTESIAN_POINT('Ctrl Pts',(0.00223383245029989,-0.0381934850979148,
-0.0102605824155735));
#30914=CARTESIAN_POINT('Ctrl Pts',(0.00282771296903102,-0.0380360809292088,
-0.0129896768874376));
#30915=CARTESIAN_POINT('Ctrl Pts',(0.000873971165030867,-0.0378786767605029,
-0.0149855586503702));
#30916=CARTESIAN_POINT('Ctrl Pts',(-0.00186717331801599,-0.0377212725917968,
-0.0144500418346802));
#30917=CARTESIAN_POINT('Ctrl Pts',(-0.002926091622306,-0.0375638684230909,
-0.0118655993205774));
#30918=CARTESIAN_POINT('Ctrl Pts',(-0.00134875343080115,-0.0374064642543849,
-0.00956067949981042));
#30919=CARTESIAN_POINT('Ctrl Pts',(0.00144374153121912,-0.0372490600856789,
-0.00961189538342548));
#30920=CARTESIAN_POINT('Ctrl Pts',(0.00293550038438004,-0.0370916559169729,
-0.0119731041140629));
#30921=CARTESIAN_POINT('Ctrl Pts',(0.00178252591997789,-0.036934251748267,
-0.0145169793157163));
#30922=CARTESIAN_POINT('Ctrl Pts',(-0.000976411780991844,-0.0367768475795609,
-0.0149516216074763));
#30923=CARTESIAN_POINT('Ctrl Pts',(-0.00285565320020116,-0.036619443410855,
-0.0128854408691303));
#30924=CARTESIAN_POINT('Ctrl Pts',(-0.0021620994638269,-0.036462039242149,
-0.0101799585883167));
#30925=CARTESIAN_POINT('Ctrl Pts',(0.000479393548670495,-0.0363046350734431,
-0.00927267372561462));
#30926=CARTESIAN_POINT('Ctrl Pts',(0.00268897788263155,-0.0361472309047371,
-0.0109810028003882));
#30927=CARTESIAN_POINT('Ctrl Pts',(0.00247593286152883,-0.0359898267360311,
-0.0137658300797473));
#30928=CARTESIAN_POINT('Ctrl Pts',(3.22009796572556E-5,-0.0358324225673251,
-0.0151181708823559));
#30929=CARTESIAN_POINT('Ctrl Pts',(-0.00244054231173649,-0.0356750183986191,
-0.0138196364116234));
#30930=CARTESIAN_POINT('Ctrl Pts',(-0.00271448378888876,-0.0355176142299131,
-0.0110401387548681));
#30931=CARTESIAN_POINT('Ctrl Pts',(-0.00054281641465795,-0.0353602100612072,
-0.00928386088033424));
#30932=CARTESIAN_POINT('Ctrl Pts',(0.00211790034487343,-0.0352028058925012,
-0.0101331178982203));
#30933=CARTESIAN_POINT('Ctrl Pts',(0.00287049893807899,-0.0350454017237951,
-0.0128227733620499));
#30934=CARTESIAN_POINT('Ctrl Pts',(0.00103692713691383,-0.0348879975550892,
-0.0149295874514114));
#30935=CARTESIAN_POINT('Ctrl Pts',(-0.00173086213672248,-0.0347305933863832,
-0.0145554301398706));
#30936=CARTESIAN_POINT('Ctrl Pts',(-0.00293923455935166,-0.0345731892176772,
-0.0120373977247868));
#30937=CARTESIAN_POINT('Ctrl Pts',(-0.00149950936434765,-0.0344157850489713,
-0.0096441065760777));
#30938=CARTESIAN_POINT('Ctrl Pts',(0.0012911958547517,-0.0342583808802653,
-0.00953178766741874));
#30939=CARTESIAN_POINT('Ctrl Pts',(0.00291860069797893,-0.0341009767115593,
-0.0118016344952603));
#30940=CARTESIAN_POINT('Ctrl Pts',(0.00191649796096373,-0.0339435725428533,
-0.014408633015419));
#30941=CARTESIAN_POINT('Ctrl Pts',(-0.00081226986010739,-0.0337861683741473,
-0.0150040130026805));
#30942=CARTESIAN_POINT('Ctrl Pts',(-0.00280922474030466,-0.0336287642054413,
-0.0130513680553543));
#30943=CARTESIAN_POINT('Ctrl Pts',(-0.00227521409808231,-0.0334713600367354,
-0.010309929752051));
#30944=CARTESIAN_POINT('Ctrl Pts',(0.000308646235065284,-0.0333139558680293,
-0.00924959167997635));
#30945=CARTESIAN_POINT('Ctrl Pts',(0.0026144323340779,-0.0331565516993234,
-0.0108256631163291));
#30946=CARTESIAN_POINT('Ctrl Pts',(0.00256475076989575,-0.0329991475306174,
-0.0136181860389024));
#30947=CARTESIAN_POINT('Ctrl Pts',(0.000204361973829126,-0.0328417433619114,
-0.0151112415146089));
#30948=CARTESIAN_POINT('Ctrl Pts',(-0.0023401462436483,-0.0326843391932055,
-0.0139596658453702));
#30949=CARTESIAN_POINT('Ctrl Pts',(-0.00277630447953526,-0.0325269350244995,
-0.0112009655499111));
#30950=CARTESIAN_POINT('Ctrl Pts',(-0.000711156260506898,-0.0323695308557934,
-0.00932059272638428));
#30951=CARTESIAN_POINT('Ctrl Pts',(0.00199470607115752,-0.0322121266870875,
-0.0100126529867227));
#30952=CARTESIAN_POINT('Ctrl Pts',(0.00290344329131625,-0.0320547225183815,
-0.0126536605239274));
#30953=CARTESIAN_POINT('Ctrl Pts',(0.00119632621131608,-0.0318973183496755,
-0.0148641570188858));
#30954=CARTESIAN_POINT('Ctrl Pts',(-0.00158861326091204,-0.0317399141809696,
-0.0146526929509304));
#30955=CARTESIAN_POINT('Ctrl Pts',(-0.00294230517095442,-0.0315825100122636,
-0.0122096054708049));
#30956=CARTESIAN_POINT('Ctrl Pts',(-0.00164511267066117,-0.0314251058435576,
-0.00973634180739135));
#30957=CARTESIAN_POINT('Ctrl Pts',(0.00113420127685958,-0.0312677016748516,
-0.00946049802842335));
#30958=CARTESIAN_POINT('Ctrl Pts',(0.00289173597783214,-0.0311102975061456,
-0.0116319307799048));
#30959=CARTESIAN_POINT('Ctrl Pts',(0.0020438155783319,-0.0309528933374397,
-0.0142916889691752));
#30960=CARTESIAN_POINT('Ctrl Pts',(-0.000645171746736182,-0.0307954891687337,
-0.0150485628921055));
#30961=CARTESIAN_POINT('Ctrl Pts',(-0.00275359209284296,-0.0306380850000277,
-0.0132104562352686));
#30962=CARTESIAN_POINT('Ctrl Pts',(-0.00250366401600948,-0.030533148887557,
-0.0113742149202441));
#30963=CARTESIAN_POINT('Ctrl Pts',(-0.00201987106857834,-0.0304806808313217,
-0.0107083310541483));
#30964=CARTESIAN_POINT('',(-0.00112535951647366,-0.0304787743898623,-0.0149567822606029));
#30965=CARTESIAN_POINT('Ctrl Pts',(-0.00202254248593818,-0.0304787743898724,
-0.010706390155828));
#30966=CARTESIAN_POINT('Ctrl Pts',(-0.00207933679775776,-0.0304787743898759,
-0.010768823046726));
#30967=CARTESIAN_POINT('Ctrl Pts',(-0.00213253650680991,-0.0304787743898759,
-0.0108341592693267));
#30968=CARTESIAN_POINT('Ctrl Pts',(-0.00218216719076719,-0.0304787743898759,
-0.0109020191122561));
#30969=CARTESIAN_POINT('Ctrl Pts',(-0.00228485960892478,-0.0304787743898758,
-0.0110424300598912));
#30970=CARTESIAN_POINT('Ctrl Pts',(-0.00237230998742211,-0.0304787743898757,
-0.0111936097303547));
#30971=CARTESIAN_POINT('Ctrl Pts',(-0.00244435095552589,-0.0304787743898755,
-0.0113527208897216));
#30972=CARTESIAN_POINT('Ctrl Pts',(-0.00245258921046642,-0.0304787743898755,
-0.0113709160685101));
#30973=CARTESIAN_POINT('Ctrl Pts',(-0.00246062531162263,-0.0304787743898755,
-0.0113892155623281));
#30974=CARTESIAN_POINT('Ctrl Pts',(-0.00246845849194243,-0.0304787743898755,
-0.0114076155457809));
#30975=CARTESIAN_POINT('Ctrl Pts',(-0.00247483468516254,-0.0304787743898755,
-0.0114225930957609));
#30976=CARTESIAN_POINT('Ctrl Pts',(-0.00248107304918276,-0.0304787743898755,
-0.0114376294063823));
#30977=CARTESIAN_POINT('Ctrl Pts',(-0.00248717124270606,-0.0304787743898755,
-0.0114527162532319));
#30978=CARTESIAN_POINT('Ctrl Pts',(-0.00255536474803799,-0.0304787743898753,
-0.0116214260469026));
#30979=CARTESIAN_POINT('Ctrl Pts',(-0.00260618039173054,-0.030478774389875,
-0.0117966365888452));
#30980=CARTESIAN_POINT('Ctrl Pts',(-0.00263944649157874,-0.0304787743898749,
-0.0119752482167937));
#30981=CARTESIAN_POINT('Ctrl Pts',(-0.00264856017282487,-0.0304787743898748,
-0.0120241811981592));
#30982=CARTESIAN_POINT('Ctrl Pts',(-0.00265635281447305,-0.0304787743898747,
-0.0120733723859067));
#30983=CARTESIAN_POINT('Ctrl Pts',(-0.00266281171147326,-0.0304787743898747,
-0.0121227634589119));
#30984=CARTESIAN_POINT('Ctrl Pts',(-0.00266823331331669,-0.0304787743898746,
-0.0121642223538975));
#30985=CARTESIAN_POINT('Ctrl Pts',(-0.00267271510098182,-0.0304787743898745,
-0.0122058221316629));
#30986=CARTESIAN_POINT('Ctrl Pts',(-0.00267624717494561,-0.0304787743898745,
-0.0122475289422248));
#30987=CARTESIAN_POINT('Ctrl Pts',(-0.00267748798737737,-0.0304787743898745,
-0.0122621804839435));
#30988=CARTESIAN_POINT('Ctrl Pts',(-0.00267861105896926,-0.0304787743898745,
-0.0122768396339577));
#30989=CARTESIAN_POINT('Ctrl Pts',(-0.00267961576376998,-0.0304787743898744,
-0.0122914972696341));
#30990=CARTESIAN_POINT('Ctrl Pts',(-0.00269915394615531,-0.030478774389874,
-0.0125765397607023));
#30991=CARTESIAN_POINT('Ctrl Pts',(-0.00267434900802219,-0.0304787743898735,
-0.0128617661037894));
#30992=CARTESIAN_POINT('Ctrl Pts',(-0.00260324668114919,-0.0304787743898729,
-0.0131363711390872));
#30993=CARTESIAN_POINT('Ctrl Pts',(-0.00260161897333744,-0.0304787743898729,
-0.0131426575263372));
#30994=CARTESIAN_POINT('Ctrl Pts',(-0.00259996681043361,-0.0304787743898729,
-0.0131489383768583));
#30995=CARTESIAN_POINT('Ctrl Pts',(-0.00259829014110119,-0.0304787743898729,
-0.0131552135626665));
#30996=CARTESIAN_POINT('Ctrl Pts',(-0.00258319016612878,-0.0304787743898728,
-0.0132117274779743));
#30997=CARTESIAN_POINT('Ctrl Pts',(-0.0025660879293159,-0.0304787743898726,
-0.0132678257833988));
#30998=CARTESIAN_POINT('Ctrl Pts',(-0.00254710084680293,-0.0304787743898725,
-0.0133233047976962));
#30999=CARTESIAN_POINT('Ctrl Pts',(-0.00243724439375196,-0.0304787743898718,
-0.013644298174394));
#31000=CARTESIAN_POINT('Ctrl Pts',(-0.00226595903811895,-0.0304787743898712,
-0.0139422543456244));
#31001=CARTESIAN_POINT('Ctrl Pts',(-0.00204792614583985,-0.0304787743898704,
-0.0142063722525525));
#31002=CARTESIAN_POINT('Ctrl Pts',(-0.00203805779522129,-0.0304787743898703,
-0.0142183264493847));
#31003=CARTESIAN_POINT('Ctrl Pts',(-0.00202809230240618,-0.0304787743898703,
-0.0142302109176497));
#31004=CARTESIAN_POINT('Ctrl Pts',(-0.00201803066157199,-0.0304787743898703,
-0.014242024505078));
#31005=CARTESIAN_POINT('Ctrl Pts',(-0.00200805701449532,-0.0304787743898702,
-0.0142537347771559));
#31006=CARTESIAN_POINT('Ctrl Pts',(-0.00199799386009692,-0.0304787743898703,
-0.0142653695213677));
#31007=CARTESIAN_POINT('Ctrl Pts',(-0.00198784674813982,-0.0304787743898702,
-0.0142769230298409));
#31008=CARTESIAN_POINT('Ctrl Pts',(-0.00179041923550486,-0.0304787743898696,
-0.0145017141280078));
#31009=CARTESIAN_POINT('Ctrl Pts',(-0.00156103476696635,-0.030478774389869,
-0.0146964800346998));
#31010=CARTESIAN_POINT('Ctrl Pts',(-0.0013081573752397,-0.0304787743898684,
-0.0148540088522852));
#31011=CARTESIAN_POINT('Ctrl Pts',(-0.00124886968763201,-0.0304787743898683,
-0.0148909418468184));
#31012=CARTESIAN_POINT('Ctrl Pts',(-0.00118827577426145,-0.0304787743881383,
-0.0149258181448674));
#31013=CARTESIAN_POINT('Ctrl Pts',(-0.00112646089251171,-0.030478774389873,
-0.0149585221565764));
#31014=CARTESIAN_POINT('',(-0.00299999968372376,-0.0402901830710539,-0.012175061470323));
#31015=CARTESIAN_POINT('Ctrl Pts',(-0.00299999999996642,-0.0402902259228274,
-0.0121758674800884));
#31016=CARTESIAN_POINT('Ctrl Pts',(-0.0029999973909628,-0.0403194684506487,
-0.0127273166757509));
#31017=CARTESIAN_POINT('Ctrl Pts',(-0.00284359154959909,-0.0403487109784699,
-0.0132796810926993));
#31018=CARTESIAN_POINT('Ctrl Pts',(-0.00255417076918103,-0.0403779535062912,
-0.0137494516094668));
#31019=CARTESIAN_POINT('Ctrl Pts',(-0.00236761854760589,-0.0403968023896424,
-0.0140522520283134));
#31020=CARTESIAN_POINT('Ctrl Pts',(-0.00212699904315092,-0.0404156512729936,
-0.0143208130958077));
#31021=CARTESIAN_POINT('Ctrl Pts',(-0.00184856593603868,-0.0404345001563449,
-0.0145386490839383));
#31022=CARTESIAN_POINT('Ctrl Pts',(-0.00141659934526726,-0.0404637426841661,
-0.0148766041142004));
#31023=CARTESIAN_POINT('Ctrl Pts',(-0.000886891013127971,-0.0404929852119873,
-0.015094515020395));
#31024=CARTESIAN_POINT('Ctrl Pts',(-0.000337993503381779,-0.0405222277398086,
-0.0151567525454516));
#31025=CARTESIAN_POINT('Ctrl Pts',(1.58098749104893E-5,-0.0405410766231597,
-0.0151968690448537));
#31026=CARTESIAN_POINT('Ctrl Pts',(0.000376850571609003,-0.0405599255065109,
-0.0151732399838831));
#31027=CARTESIAN_POINT('Ctrl Pts',(0.000721855543562045,-0.0405787743898621,
-0.0150877125850526));
#31028=CARTESIAN_POINT('',(-0.00299999946992021,-0.0392900367108314,-0.0121771409863751));
#31029=CARTESIAN_POINT('Ctrl Pts',(-0.00299999898776283,-0.0392900992552675,
-0.012178317717926));
#31030=CARTESIAN_POINT('Ctrl Pts',(-0.00299954158667841,-0.0393196461574803,
-0.0127351207225248));
#31031=CARTESIAN_POINT('Ctrl Pts',(-0.00283976987755387,-0.039349193059693,
-0.0132919112893292));
#31032=CARTESIAN_POINT('Ctrl Pts',(-0.00254505043098655,-0.0393787399619057,
-0.0137641600276302));
#31033=CARTESIAN_POINT('Ctrl Pts',(-0.00242416025283272,-0.0393908597263596,
-0.0139578704691063));
#31034=CARTESIAN_POINT('Ctrl Pts',(-0.002281166455956,-0.0394029794908136,
-0.0141375264551638));
#31035=CARTESIAN_POINT('Ctrl Pts',(-0.00212000447914795,-0.0394150992552675,
-0.0142984886787988));
#31036=CARTESIAN_POINT('Ctrl Pts',(-0.00173434249492379,-0.039444101954913,
-0.0146836726519771));
#31037=CARTESIAN_POINT('Ctrl Pts',(-0.00123911027380901,-0.0394731046545585,
-0.0149622077535727));
#31038=CARTESIAN_POINT('Ctrl Pts',(-0.000707581479706982,-0.0395021073542039,
-0.0150912140617583));
#31039=CARTESIAN_POINT('Ctrl Pts',(-0.000475490563978323,-0.0395147713212251,
-0.0151475443914296));
#31040=CARTESIAN_POINT('Ctrl Pts',(-0.000236850429755516,-0.0395274352882463,
-0.0151759527300397));
#31041=CARTESIAN_POINT('Ctrl Pts',(1.25624153382951E-6,-0.0395400992552675,
-0.0151758530235343));
#31042=CARTESIAN_POINT('Ctrl Pts',(0.000548578657520092,-0.039569209204134,
-0.0151756238337971));
#31043=CARTESIAN_POINT('Ctrl Pts',(0.0010976461232431,-0.0395983191530005,
-0.0150212816042846));
#31044=CARTESIAN_POINT('Ctrl Pts',(0.00156584391071221,-0.039627429101867,
-0.0147347852605045));
#31045=CARTESIAN_POINT('Ctrl Pts',(0.00176780329988407,-0.0396399858196672,
-0.0146112036714019));
#31046=CARTESIAN_POINT('Ctrl Pts',(0.00195487121302341,-0.0396525425374674,
-0.0144636952428034));
#31047=CARTESIAN_POINT('Ctrl Pts',(0.00212178143067051,-0.0396650992552675,
-0.0142967124427639));
#31048=CARTESIAN_POINT('Ctrl Pts',(0.00250865271321648,-0.0396942037258529,
-0.0139096729258002));
#31049=CARTESIAN_POINT('Ctrl Pts',(0.00278783414274103,-0.0397233081964383,
-0.0134124406496366));
#31050=CARTESIAN_POINT('Ctrl Pts',(0.00291644867266022,-0.0397524126670237,
-0.0128789373069557));
#31051=CARTESIAN_POINT('Ctrl Pts',(0.00297196182618088,-0.039764974863105,
-0.0126486643122587));
#31052=CARTESIAN_POINT('Ctrl Pts',(0.00300000378267172,-0.0397775370591862,
-0.0124119928788954));
#31053=CARTESIAN_POINT('Ctrl Pts',(0.00299999999961518,-0.0397900992552675,
-0.0121758052350621));
#31054=CARTESIAN_POINT('Ctrl Pts',(0.00299999123491694,-0.0398192037258529,
-0.0116285986568405));
#31055=CARTESIAN_POINT('Ctrl Pts',(0.00284593322591044,-0.0398483081964383,
-0.0110795663259316));
#31056=CARTESIAN_POINT('Ctrl Pts',(0.00255972584052127,-0.0398774126670237,
-0.0106113074670412));
#31057=CARTESIAN_POINT('Ctrl Pts',(0.00243619178465802,-0.039889974863105,
-0.0104091955755051));
#31058=CARTESIAN_POINT('Ctrl Pts',(0.00228870187842766,-0.0399025370591862,
-0.010221976464095));
#31059=CARTESIAN_POINT('Ctrl Pts',(0.00212171348927827,-0.0399150992552675,
-0.0100549261615926));
#31060=CARTESIAN_POINT('Ctrl Pts',(0.00173475698597329,-0.039944209204134,
-0.00966782618858453));
#31061=CARTESIAN_POINT('Ctrl Pts',(0.00123753050888079,-0.0399733191530005,
-0.00938841725028805));
#31062=CARTESIAN_POINT('Ctrl Pts',(0.000703965181250702,-0.040002429101867,
-0.00925961718096125));
#31063=CARTESIAN_POINT('Ctrl Pts',(0.000473809186208603,-0.0400149858196672,
-0.00920405864560988));
#31064=CARTESIAN_POINT('Ctrl Pts',(0.00023725032350367,-0.0400275425374673,
-0.00917594480999342));
#31065=CARTESIAN_POINT('Ctrl Pts',(1.16013854950112E-6,-0.0400400992552675,
-0.00917585351087835));
#31066=CARTESIAN_POINT('Ctrl Pts',(-0.000544145795090869,-0.040069101954913,
-0.00917564263405095));
#31067=CARTESIAN_POINT('Ctrl Pts',(-0.00109148312293973,-0.0400981046545585,
-0.00932844585482911));
#31068=CARTESIAN_POINT('Ctrl Pts',(-0.00155873907649531,-0.0401271073542039,
-0.00961258730515731));
#31069=CARTESIAN_POINT('Ctrl Pts',(-0.00176276539330768,-0.0401397713212251,
-0.00973665706418991));
#31070=CARTESIAN_POINT('Ctrl Pts',(-0.00195167937928901,-0.0401524352882463,
-0.00988509065248151));
#31071=CARTESIAN_POINT('Ctrl Pts',(-0.00212007247526431,-0.0401650992552675,
-0.0100532858083312));
#31072=CARTESIAN_POINT('Ctrl Pts',(-0.00251295839574671,-0.0401946461574802,
-0.0104457099053165));
#31073=CARTESIAN_POINT('Ctrl Pts',(-0.00279479323571491,-0.0402241930596929,
-0.0109512266395961));
#31074=CARTESIAN_POINT('Ctrl Pts',(-0.00292147013814697,-0.0402537399619056,
-0.0114939352328922));
#31075=CARTESIAN_POINT('Ctrl Pts',(-0.00297343139649411,-0.0402658597263596,
-0.0117165474130297));
#31076=CARTESIAN_POINT('Ctrl Pts',(-0.00299981876148167,-0.0402779794908135,
-0.0119450914234068));
#31077=CARTESIAN_POINT('Ctrl Pts',(-0.00299999906516995,-0.0402900992552675,
-0.0121734849581512));
#31078=CARTESIAN_POINT('',(-0.00299999999997869,-0.0382901316627664,-0.0121758419798184));
#31079=CARTESIAN_POINT('Ctrl Pts',(-0.00299999999997869,-0.0382901316627664,
-0.0121758419798184));
#31080=CARTESIAN_POINT('Ctrl Pts',(-0.00300000209850155,-0.0383196658629544,
-0.0127326398498295));
#31081=CARTESIAN_POINT('Ctrl Pts',(-0.0028406928257506,-0.0383492000631425,
-0.0132895576126836));
#31082=CARTESIAN_POINT('Ctrl Pts',(-0.00254636805818545,-0.0383787342633305,
-0.0137620467527698));
#31083=CARTESIAN_POINT('Ctrl Pts',(-0.00242552924534037,-0.0383908599084761,
-0.0139560332366208));
#31084=CARTESIAN_POINT('Ctrl Pts',(-0.0022825348872017,-0.0384029855536217,
-0.0141359579429274));
#31085=CARTESIAN_POINT('Ctrl Pts',(-0.00212132786731001,-0.0384151111987673,
-0.0142971661063407));
#31086=CARTESIAN_POINT('Ctrl Pts',(-0.00173591447646292,-0.0384441011646814,
-0.0146825822311167));
#31087=CARTESIAN_POINT('Ctrl Pts',(-0.00124086710218791,-0.0384730911305954,
-0.014961424000368));
#31088=CARTESIAN_POINT('Ctrl Pts',(-0.000709429170937981,-0.0385020810965095,
-0.0150907649921544));
#31089=CARTESIAN_POINT('Ctrl Pts',(-0.000477167617824278,-0.038514750975929,
-0.0151472926464054));
#31090=CARTESIAN_POINT('Ctrl Pts',(-0.000238327411029265,-0.0385274208553486,
-0.0151758524942411));
#31091=CARTESIAN_POINT('Ctrl Pts',(-9.97367769725772E-9,-0.0385400907347681,
-0.0151758532865415));
#31092=CARTESIAN_POINT('Ctrl Pts',(0.000547301483854578,-0.0385691879349098,
-0.0151758551061109));
#31093=CARTESIAN_POINT('Ctrl Pts',(0.0010964252806087,-0.0385982851350515,
-0.0150217505661102));
#31094=CARTESIAN_POINT('Ctrl Pts',(0.0015647392256642,-0.0386273823351932,
-0.0147354609040784));
#31095=CARTESIAN_POINT('Ctrl Pts',(0.00176693262920518,-0.0386399449803851,
-0.0146118560407683));
#31096=CARTESIAN_POINT('Ctrl Pts',(0.00195421808405336,-0.038652507625577,
-0.0144642748528175));
#31097=CARTESIAN_POINT('Ctrl Pts',(0.00212131376240286,-0.0386650702707689,
-0.0142971802112541));
#31098=CARTESIAN_POINT('Ctrl Pts',(0.00250826280330305,-0.038694162007648,
-0.0139102335712741));
#31099=CARTESIAN_POINT('Ctrl Pts',(0.00278755190614221,-0.0387232537445272,
-0.0134130729657069));
#31100=CARTESIAN_POINT('Ctrl Pts',(0.00291628703057831,-0.0387523454814063,
-0.012879607473246));
#31101=CARTESIAN_POINT('Ctrl Pts',(0.00297190272009648,-0.0387649135898608,
-0.0126491416129975));
#31102=CARTESIAN_POINT('Ctrl Pts',(0.00299999931911397,-0.0387774816983152,
-0.0124122595203428));
#31103=CARTESIAN_POINT('Ctrl Pts',(0.00299999999998756,-0.0387900498067697,
-0.0121758619271738));
#31104=CARTESIAN_POINT('Ctrl Pts',(0.00300000157602387,-0.0388191415436489,
-0.0116286660938282));
#31105=CARTESIAN_POINT('Ctrl Pts',(0.00284595972857232,-0.038848233280528,
-0.0110796393911313));
#31106=CARTESIAN_POINT('Ctrl Pts',(0.00255977000054816,-0.0388773250174071,
-0.0106113797187745));
#31107=CARTESIAN_POINT('Ctrl Pts',(0.00243613133451351,-0.0388898931258616,
-0.0104090838444685));
#31108=CARTESIAN_POINT('Ctrl Pts',(0.00228849336430286,-0.0389024612343161,
-0.0102217068524303));
#31109=CARTESIAN_POINT('Ctrl Pts',(0.00212132598208153,-0.0389150293427706,
-0.0100545385815353));
#31110=CARTESIAN_POINT('Ctrl Pts',(0.00173430650375096,-0.0389441265429123,
-0.00966751704578188));
#31111=CARTESIAN_POINT('Ctrl Pts',(0.00123703934374884,-0.038973223743054,
-0.00938820096654016));
#31112=CARTESIAN_POINT('Ctrl Pts',(0.000703460243350564,-0.0390023209431956,
-0.00925949533767302));
#31113=CARTESIAN_POINT('Ctrl Pts',(0.000473088768174648,-0.0390148835883876,
-0.00920392699632787));
#31114=CARTESIAN_POINT('Ctrl Pts',(0.000236307694429044,-0.0390274462335795,
-0.00917585386215959));
#31115=CARTESIAN_POINT('Ctrl Pts',(7.30755370494918E-9,-0.0390400088787714,
-0.009175853286567));
#31116=CARTESIAN_POINT('Ctrl Pts',(-0.000545287099503098,-0.0390689988446854,
-0.00917585195831094));
#31117=CARTESIAN_POINT('Ctrl Pts',(-0.00109255643801982,-0.0390979888105995,
-0.00932885928753787));
#31118=CARTESIAN_POINT('Ctrl Pts',(-0.00155969815203688,-0.0391269787765136,
-0.00961317077119793));
#31119=CARTESIAN_POINT('Ctrl Pts',(-0.00176385945412274,-0.0391396486559331,
-0.00973742728899603));
#31120=CARTESIAN_POINT('Ctrl Pts',(-0.00195287221682881,-0.0391523185353526,
-0.00988608556203413));
#31121=CARTESIAN_POINT('Ctrl Pts',(-0.00212131564764227,-0.0391649884147722,
-0.0100545282470915));
#31122=CARTESIAN_POINT('Ctrl Pts',(-0.0025139667409373,-0.0391945226149602,
-0.0104471776019871));
#31123=CARTESIAN_POINT('Ctrl Pts',(-0.00279550442572559,-0.0392240568151483,
-0.0109528531345857));
#31124=CARTESIAN_POINT('Ctrl Pts',(-0.00292186532648642,-0.0392535910153363,
-0.0114956305187266));
#31125=CARTESIAN_POINT('Ctrl Pts',(-0.0029737444169357,-0.0392657166604818,
-0.0117184747437687));
#31126=CARTESIAN_POINT('Ctrl Pts',(-0.00299999954473676,-0.0392778423056274,
-0.0119472467965074));
#31127=CARTESIAN_POINT('Ctrl Pts',(-0.00299999999999405,-0.039289967950773,
-0.0121758473120664));
#31128=CARTESIAN_POINT('',(-0.00299999975524206,-0.0372901454620687,-0.012175006789073));
#31129=CARTESIAN_POINT('Ctrl Pts',(-0.00299999999992875,-0.0372901916688699,
-0.0121758739623732));
#31130=CARTESIAN_POINT('Ctrl Pts',(-0.00299999616250721,-0.037319729033795,
-0.0127326725489632));
#31131=CARTESIAN_POINT('Ctrl Pts',(-0.00284068056307778,-0.0373492663987202,
-0.0132895892145799));
#31132=CARTESIAN_POINT('Ctrl Pts',(-0.00254635010445755,-0.0373788037636454,
-0.0137620755741108));
#31133=CARTESIAN_POINT('Ctrl Pts',(-0.00242552383528,-0.0373909292148201,
-0.0139560370292964));
#31134=CARTESIAN_POINT('Ctrl Pts',(-0.00228254760308849,-0.0374030546659948,
-0.0141359399142671));
#31135=CARTESIAN_POINT('Ctrl Pts',(-0.00212136282185931,-0.0374151801171696,
-0.0142971311509674));
#31136=CARTESIAN_POINT('Ctrl Pts',(-0.00173595466511071,-0.0374441732252743,
-0.0146825547433621));
#31137=CARTESIAN_POINT('Ctrl Pts',(-0.00124091039930104,-0.037473166333379,
-0.0149614049572775));
#31138=CARTESIAN_POINT('Ctrl Pts',(-0.000709473212190282,-0.0375021594414836,
-0.0150907542730728));
#31139=CARTESIAN_POINT('Ctrl Pts',(-0.000477240298278814,-0.0375148291494789,
-0.0151472786737888));
#31140=CARTESIAN_POINT('Ctrl Pts',(-0.000238429889195819,-0.0375274988574741,
-0.0151758420976629));
#31141=CARTESIAN_POINT('Ctrl Pts',(-1.40823792993672E-7,-0.0375401685654693,
-0.0151758532832529));
#31142=CARTESIAN_POINT('Ctrl Pts',(0.000547172115070815,-0.0375692689151043,
-0.0151758789748142));
#31143=CARTESIAN_POINT('Ctrl Pts',(0.00109630381278015,-0.0375983692647393,
-0.0150217975875743));
#31144=CARTESIAN_POINT('Ctrl Pts',(0.00156463088029391,-0.0376274696143742,
-0.0147355271346158));
#31145=CARTESIAN_POINT('Ctrl Pts',(0.00176680518933334,-0.0376400320808392,
-0.0146119456996743));
#31146=CARTESIAN_POINT('Ctrl Pts',(0.00195407617399039,-0.0376525945473041,
-0.0144643931084875));
#31147=CARTESIAN_POINT('Ctrl Pts',(0.00212116366158087,-0.037665157013769,
-0.0142973303005247));
#31148=CARTESIAN_POINT('Ctrl Pts',(0.00250814109920495,-0.03769425189785,
-0.0139104100213344));
#31149=CARTESIAN_POINT('Ctrl Pts',(0.00278746564107153,-0.037723346781931,
-0.0134132678179795));
#31150=CARTESIAN_POINT('Ctrl Pts',(0.00291623811122977,-0.0377524416660121,
-0.0128798101592506));
#31151=CARTESIAN_POINT('Ctrl Pts',(0.00297186313610854,-0.0377650095980309,
-0.0126493758474594));
#31152=CARTESIAN_POINT('Ctrl Pts',(0.00299997616477368,-0.0377775775300498,
-0.0124125249373827));
#31153=CARTESIAN_POINT('Ctrl Pts',(0.00299999998476676,-0.0377901454620687,
-0.0121761556099587));
#31154=CARTESIAN_POINT('Ctrl Pts',(0.00300005512828093,-0.0378192403461497,
-0.0116289583326836));
#31155=CARTESIAN_POINT('Ctrl Pts',(0.00284606624918581,-0.0378483352302307,
-0.0110799154030114));
#31156=CARTESIAN_POINT('Ctrl Pts',(0.00255992117660712,-0.0378774301143118,
-0.0106116270978122));
#31157=CARTESIAN_POINT('Ctrl Pts',(0.00243631690962701,-0.0378899980463306,
-0.0104093435771565));
#31158=CARTESIAN_POINT('Ctrl Pts',(0.00228871769291662,-0.0379025659783495,
-0.0102219730135154));
#31159=CARTESIAN_POINT('Ctrl Pts',(0.00212159119992591,-0.0379151339103684,
-0.0100548038339529));
#31160=CARTESIAN_POINT('Ctrl Pts',(0.00173461907340646,-0.0379442342600034,
-0.00966773286904355));
#31161=CARTESIAN_POINT('Ctrl Pts',(0.00123738544701644,-0.0379733346096384,
-0.00938835434554213));
#31162=CARTESIAN_POINT('Ctrl Pts',(0.000703821130662529,-0.0380024349592733,
-0.00925958241161645));
#31163=CARTESIAN_POINT('Ctrl Pts',(0.000473484247595724,-0.0380149974257383,
-0.00920399225129686));
#31164=CARTESIAN_POINT('Ctrl Pts',(0.000236735910866754,-0.0380275598922032,
-0.00917588985189061));
#31165=CARTESIAN_POINT('Ctrl Pts',(4.63823007370569E-7,-0.0380401223586681,
-0.00917585332241339));
#31166=CARTESIAN_POINT('Ctrl Pts',(-0.000544832134960051,-0.0380691154667728,
-0.00917576901547534));
#31167=CARTESIAN_POINT('Ctrl Pts',(-0.00109212599337851,-0.0380981085748774,
-0.00932869389979686));
#31168=CARTESIAN_POINT('Ctrl Pts',(-0.00155931164168855,-0.0381271016829821,
-0.0096129355734634));
#31169=CARTESIAN_POINT('Ctrl Pts',(-0.00176346725419761,-0.0381397713909773,
-0.00973714643738421));
#31170=CARTESIAN_POINT('Ctrl Pts',(-0.00195248165559007,-0.0381524410989726,
-0.0098857554706572));
#31171=CARTESIAN_POINT('Ctrl Pts',(-0.00212093523748278,-0.0381651108069678,
-0.0100541479068213));
#31172=CARTESIAN_POINT('Ctrl Pts',(-0.00251365738413268,-0.038194648171893,
-0.0104467275021434));
#31173=CARTESIAN_POINT('Ctrl Pts',(-0.00279528586443748,-0.0382241855368181,
-0.0109523533829576));
#31174=CARTESIAN_POINT('Ctrl Pts',(-0.00292174382330747,-0.0382537229017433,
-0.011495108818373));
#31175=CARTESIAN_POINT('Ctrl Pts',(-0.00297365636898722,-0.038265848352918,
-0.01171791659248));
#31176=CARTESIAN_POINT('Ctrl Pts',(-0.00299995229094424,-0.0382779738040928,
-0.011946655308718));
#31177=CARTESIAN_POINT('Ctrl Pts',(-0.0029999999348286,-0.0382900992552675,
-0.0121752279639453));
#31178=CARTESIAN_POINT('',(-0.00299999945826961,-0.0362900263245557,-0.0121770992877974));
#31179=CARTESIAN_POINT('Ctrl Pts',(-0.00299999885509523,-0.0362900992552675,
-0.0121784742457941));
#31180=CARTESIAN_POINT('Ctrl Pts',(-0.00299951240275064,-0.0363196453473993,
-0.0127352766778096));
#31181=CARTESIAN_POINT('Ctrl Pts',(-0.00283971194097578,-0.0363491914395311,
-0.0132920584481428));
#31182=CARTESIAN_POINT('Ctrl Pts',(-0.00254496835509526,-0.0363787375316629,
-0.0137642915357714));
#31183=CARTESIAN_POINT('Ctrl Pts',(-0.00242405687937795,-0.0363908581061978,
-0.013958013815892));
#31184=CARTESIAN_POINT('Ctrl Pts',(-0.00228103836935438,-0.0364029786807326,
-0.0141376778523285));
#31185=CARTESIAN_POINT('Ctrl Pts',(-0.00211984966677049,-0.0364150992552675,
-0.0142986432880168));
#31186=CARTESIAN_POINT('Ctrl Pts',(-0.00173416044612212,-0.0364441011323918,
-0.0146837982799409));
#31187=CARTESIAN_POINT('Ctrl Pts',(-0.00123890904906828,-0.0364731030095161,
-0.0149622970438916));
#31188=CARTESIAN_POINT('Ctrl Pts',(-0.000707371908332917,-0.0365021048866404,
-0.0150912649184381));
#31189=CARTESIAN_POINT('Ctrl Pts',(-0.000475255690733393,-0.0365147696761827,
-0.0151475837209026));
#31190=CARTESIAN_POINT('Ctrl Pts',(-0.000236591057320712,-0.0365274344657251,
-0.0151759749177501));
#31191=CARTESIAN_POINT('Ctrl Pts',(1.53730189014851E-6,-0.0365400992552675,
-0.0151758528926752));
#31192=CARTESIAN_POINT('Ctrl Pts',(0.000548858560926287,-0.0365692083818778,
-0.0151755724266364));
#31193=CARTESIAN_POINT('Ctrl Pts',(0.00109791066251957,-0.0365983175084881,
-0.0150211793683654));
#31194=CARTESIAN_POINT('Ctrl Pts',(0.00156608112127079,-0.0366274266350983,
-0.014734640093152));
#31195=CARTESIAN_POINT('Ctrl Pts',(0.00176804765113956,-0.0366399841751547,
-0.0146110284000086));
#31196=CARTESIAN_POINT('Ctrl Pts',(0.00195511772629248,-0.0366525417152111,
-0.0144634868178142));
#31197=CARTESIAN_POINT('Ctrl Pts',(0.00212202413257601,-0.0366650992552675,
-0.0142964696075283));
#31198=CARTESIAN_POINT('Ctrl Pts',(0.00250885034003301,-0.0366942029050504,
-0.0139093865981128));
#31199=CARTESIAN_POINT('Ctrl Pts',(0.00278797466275618,-0.0367233065548334,
-0.0134121234152743));
#31200=CARTESIAN_POINT('Ctrl Pts',(0.00291652844246022,-0.0367524102046163,
-0.0128786063330264));
#31201=CARTESIAN_POINT('Ctrl Pts',(0.00297202056516426,-0.0367649732215,
-0.0126483058668639));
#31202=CARTESIAN_POINT('Ctrl Pts',(0.00300003568403275,-0.0367775362383838,
-0.0124116088997408));
#31203=CARTESIAN_POINT('Ctrl Pts',(0.00299999996570114,-0.0367900992552675,
-0.0121753996422144));
#31204=CARTESIAN_POINT('Ctrl Pts',(0.00299991722014538,-0.0368192029050504,
-0.0116281941763492));
#31205=CARTESIAN_POINT('Ctrl Pts',(0.00284578558050993,-0.0368483065548334,
-0.0110791835577832));
#31206=CARTESIAN_POINT('Ctrl Pts',(0.00255951579718336,-0.0368774102046163,
-0.0106109638706667));
#31207=CARTESIAN_POINT('Ctrl Pts',(0.00243594325050775,-0.0368899732215001,
-0.0104088499819136));
#31208=CARTESIAN_POINT('Ctrl Pts',(0.00228841242440986,-0.0369025362383838,
-0.0102216348455878));
#31209=CARTESIAN_POINT('Ctrl Pts',(0.00212138269847324,-0.0369150992552675,
-0.010054595299745));
#31210=CARTESIAN_POINT('Ctrl Pts',(0.00173436662701786,-0.0369442083818778,
-0.0096675564750851));
#31211=CARTESIAN_POINT('Ctrl Pts',(0.00123709764722942,-0.036973317508488,
-0.00938822529176232));
#31212=CARTESIAN_POINT('Ctrl Pts',(0.000703513242994816,-0.0370024266350983,
-0.00925950812232754));
#31213=CARTESIAN_POINT('Ctrl Pts',(0.000473327445277312,-0.0370149841751547,
-0.00920398014195341));
#31214=CARTESIAN_POINT('Ctrl Pts',(0.000236741851205871,-0.0370275417152111,
-0.00917590293724171));
#31215=CARTESIAN_POINT('Ctrl Pts',(6.30013261930167E-7,-0.0370400992552675,
-0.00917585335271088));
#31216=CARTESIAN_POINT('Ctrl Pts',(-0.000544674758284476,-0.0370691011323918,
-0.00917573883629573));
#31217=CARTESIAN_POINT('Ctrl Pts',(-0.00109198412557387,-0.0370981030095161,
-0.00932863813475086));
#31218=CARTESIAN_POINT('Ctrl Pts',(-0.00155918934501321,-0.0371271048866403,
-0.00961286117061289));
#31219=CARTESIAN_POINT('Ctrl Pts',(-0.00176321254502702,-0.0371397696761827,
-0.00973697813438268));
#31220=CARTESIAN_POINT('Ctrl Pts',(-0.00195211634701312,-0.0371524344657251,
-0.0098854607582095));
#31221=CARTESIAN_POINT('Ctrl Pts',(-0.00212049156426993,-0.0371650992552675,
-0.0100537044873783));
#31222=CARTESIAN_POINT('Ctrl Pts',(-0.00251329948777596,-0.0371946453473993,
-0.0104462056581232));
#31223=CARTESIAN_POINT('Ctrl Pts',(-0.00279503440366669,-0.0372241914395311,
-0.0109517773932172));
#31224=CARTESIAN_POINT('Ctrl Pts',(-0.00292160434126632,-0.037253737531663,
-0.011494510441073));
#31225=CARTESIAN_POINT('Ctrl Pts',(-0.00297352661767779,-0.0372658581061978,
-0.0117171536363121));
#31226=CARTESIAN_POINT('Ctrl Pts',(-0.00299986903456971,-0.0372779786807327,
-0.0119457247437539));
#31227=CARTESIAN_POINT('Ctrl Pts',(-0.00299999951055537,-0.0372900992552675,
-0.0121741396157728));
#31228=CARTESIAN_POINT('',(-0.00299999981883512,-0.0352901375595625,-0.0121751042430183));
#31229=CARTESIAN_POINT('Ctrl Pts',(-0.00299999999990529,-0.0352901758638575,
-0.0121758294485129));
#31230=CARTESIAN_POINT('Ctrl Pts',(-0.00300000442417536,-0.03531962354091,
-0.0127326204983985));
#31231=CARTESIAN_POINT('Ctrl Pts',(-0.00284070124558744,-0.0353490857174387,
-0.0132895327727721));
#31232=CARTESIAN_POINT('Ctrl Pts',(-0.00254638511743984,-0.0353785627573661,
-0.0137620193666647));
#31233=CARTESIAN_POINT('Ctrl Pts',(-0.00242551849306003,-0.0353906680753287,
-0.0139560551472655));
#31234=CARTESIAN_POINT('Ctrl Pts',(-0.00228248521019157,-0.0354027758999937,
-0.0141360222982122));
#31235=CARTESIAN_POINT('Ctrl Pts',(-0.00212123128764963,-0.0354148862565662,
-0.0142972626822892));
#31236=CARTESIAN_POINT('Ctrl Pts',(-0.00173579965280455,-0.0354438326192885,
-0.0146826619572847));
#31237=CARTESIAN_POINT('Ctrl Pts',(-0.00124073796889185,-0.0354727934471282,
-0.0149614820143835));
#31238=CARTESIAN_POINT('Ctrl Pts',(-0.0007092914864209,-0.0355017677075181,
-0.0150907984982715));
#31239=CARTESIAN_POINT('Ctrl Pts',(-0.000476980661877979,-0.0355144332054444,
-0.015147326521299));
#31240=CARTESIAN_POINT('Ctrl Pts',(-0.000238089691008945,-0.0355271012700895,
-0.0151758751813239));
#31241=CARTESIAN_POINT('Ctrl Pts',(2.75720825596021E-7,-0.0355397718152056,
-0.0151758532738878));
#31242=CARTESIAN_POINT('Ctrl Pts',(0.000547620237042205,-0.0355688664448895,
-0.0151758029691269));
#31243=CARTESIAN_POINT('Ctrl Pts',(0.00109675921247324,-0.0355979741534132,
-0.0150216280988535));
#31244=CARTESIAN_POINT('Ctrl Pts',(0.00156506425454912,-0.0356270987696597,
-0.0147352621790824));
#31245=CARTESIAN_POINT('Ctrl Pts',(0.00176725681833465,-0.0356396734385167,
-0.0146116225546986));
#31246=CARTESIAN_POINT('Ctrl Pts',(0.00195453657837562,-0.0356522512591675,
-0.0144640047557032));
#31247=CARTESIAN_POINT('Ctrl Pts',(0.00212162119625327,-0.0356648325397757,
-0.0142968727347501));
#31248=CARTESIAN_POINT('Ctrl Pts',(0.00250834357656535,-0.0356939522926649,
-0.0139100406385923));
#31249=CARTESIAN_POINT('Ctrl Pts',(0.00278749542059164,-0.0357230905807174,
-0.0134130907688648));
#31250=CARTESIAN_POINT('Ctrl Pts',(0.00291622194525164,-0.0357522331609794,
-0.0128798771256664));
#31251=CARTESIAN_POINT('Ctrl Pts',(0.00297192783867808,-0.035764844497101,
-0.0126491310346025));
#31252=CARTESIAN_POINT('Ctrl Pts',(0.00300004532431104,-0.0357774566370209,
-0.012411954683267));
#31253=CARTESIAN_POINT('Ctrl Pts',(0.00299999994485589,-0.0357900684264905,
-0.0121752780781935));
#31254=CARTESIAN_POINT('Ctrl Pts',(0.00299989497427525,-0.0358192416913352,
-0.0116278038835947));
#31255=CARTESIAN_POINT('Ctrl Pts',(0.00284559472580302,-0.0358484130809994,
-0.0110785757190366));
#31256=CARTESIAN_POINT('Ctrl Pts',(0.002559075740545,-0.0358775721901715,
-0.0106102443461921));
#31257=CARTESIAN_POINT('Ctrl Pts',(0.00243550281909295,-0.0358901482374588,
-0.010408257465993));
#31258=CARTESIAN_POINT('Ctrl Pts',(0.00228799813798229,-0.0359027220004333,
-0.0102211624528925));
#31259=CARTESIAN_POINT('Ctrl Pts',(0.00212101329930002,-0.0359152926443287,
-0.0100542259431746));
#31260=CARTESIAN_POINT('Ctrl Pts',(0.00173396166844446,-0.0359444299496015,
-0.00966728633329421));
#31261=CARTESIAN_POINT('Ctrl Pts',(0.00123668840944808,-0.0359735504973407,
-0.00938805148393656));
#31262=CARTESIAN_POINT('Ctrl Pts',(0.000703125243084155,-0.0360026570765507,
-0.00925941455198165));
#31263=CARTESIAN_POINT('Ctrl Pts',(0.000472761400329676,-0.0360152237300586,
-0.00920387605188761));
#31264=CARTESIAN_POINT('Ctrl Pts',(0.000235992071111057,-0.0360277877797665,
-0.00917583020942042));
#31265=CARTESIAN_POINT('Ctrl Pts',(-2.93181185161645E-7,-0.0360403494501322,
-0.00917585330088396));
#31266=CARTESIAN_POINT('Ctrl Pts',(-0.000545584584361914,-0.0360693388635356,
-0.00917590659061083));
#31267=CARTESIAN_POINT('Ctrl Pts',(-0.00109283637569486,-0.036098315605061,
-0.00932896709632053));
#31268=CARTESIAN_POINT('Ctrl Pts',(-0.00155994867156055,-0.0361272789223249,
-0.00961332325900789));
#31269=CARTESIAN_POINT('Ctrl Pts',(-0.00176405935357533,-0.0361399348136222,
-0.00973757631510365));
#31270=CARTESIAN_POINT('Ctrl Pts',(-0.00195302492857976,-0.0361525881417386,
-0.00988622044894215));
#31271=CARTESIAN_POINT('Ctrl Pts',(-0.00212142793965345,-0.036165238843901,
-0.01005464054455));
#31272=CARTESIAN_POINT('Ctrl Pts',(-0.00251406372729111,-0.0361947342690484,
-0.0104473161652017));
#31273=CARTESIAN_POINT('Ctrl Pts',(-0.00279557613143336,-0.0362242154194899,
-0.0109530141278591));
#31274=CARTESIAN_POINT('Ctrl Pts',(-0.00292190601481382,-0.0362536825604244,
-0.0114958053172245));
#31275=CARTESIAN_POINT('Ctrl Pts',(-0.00297375949271995,-0.0362657776696774,
-0.0117185998785131));
#31276=CARTESIAN_POINT('Ctrl Pts',(-0.00300000084973987,-0.0362778704186345,
-0.0119473179106401));
#31277=CARTESIAN_POINT('Ctrl Pts',(-0.00299999999997926,-0.0362899608256352,
-0.0121758644408811));
#31278=CARTESIAN_POINT('',(-0.00299999994316498,-0.0342901216939704,-0.0121754481730699));
#31279=CARTESIAN_POINT('Ctrl Pts',(-0.0029999999999601,-0.0342901441326733,
-0.0121758687597579));
#31280=CARTESIAN_POINT('Ctrl Pts',(-0.00299999712813671,-0.0343196842733559,
-0.0127326682745884));
#31281=CARTESIAN_POINT('Ctrl Pts',(-0.00284068199001415,-0.0343492244140385,
-0.0132895859952222));
#31282=CARTESIAN_POINT('Ctrl Pts',(-0.00254635150369563,-0.0343787645547211,
-0.0137620733279228));
#31283=CARTESIAN_POINT('Ctrl Pts',(-0.00242554449866458,-0.0343908892108132,
-0.0139560042397105));
#31284=CARTESIAN_POINT('Ctrl Pts',(-0.00228259454224132,-0.0344030138669054,
-0.0141358810797341));
#31285=CARTESIAN_POINT('Ctrl Pts',(-0.0021214410730114,-0.0344151385229976,
-0.0142970528937946));
#31286=CARTESIAN_POINT('Ctrl Pts',(-0.00173604568796275,-0.0344441344020535,
-0.0146824921501484));
#31287=CARTESIAN_POINT('Ctrl Pts',(-0.00124100978379169,-0.0344731302811094,
-0.0149613609980348));
#31288=CARTESIAN_POINT('Ctrl Pts',(-0.000709575571708124,-0.0345021261601653,
-0.0150907293573431));
#31289=CARTESIAN_POINT('Ctrl Pts',(-0.000477380634872773,-0.0345147950778842,
-0.0151472531515119));
#31290=CARTESIAN_POINT('Ctrl Pts',(-0.000238609269103201,-0.034527463995603,
-0.0151758249166817));
#31291=CARTESIAN_POINT('Ctrl Pts',(-3.56957372812207E-7,-0.0345401329133219,
-0.0151758532653217));
#31292=CARTESIAN_POINT('Ctrl Pts',(0.000546957897806089,-0.03456923603856,
-0.0151759183880131));
#31293=CARTESIAN_POINT('Ctrl Pts',(0.00109610222331674,-0.0345983391637982,
-0.0150218755290798));
#31294=CARTESIAN_POINT('Ctrl Pts',(0.00156445073765424,-0.0346274422890363,
-0.0147356372402255));
#31295=CARTESIAN_POINT('Ctrl Pts',(0.00176660223010131,-0.0346400039605729,
-0.0146120892935233));
#31296=CARTESIAN_POINT('Ctrl Pts',(0.00195385675957504,-0.0346525656321095,
-0.0144645766535138));
#31297=CARTESIAN_POINT('Ctrl Pts',(0.00212093622771983,-0.0346651273036461,
-0.0142975576764168));
#31298=CARTESIAN_POINT('Ctrl Pts',(0.00250795646106377,-0.034694224960607,
-0.0139106775635777));
#31299=CARTESIAN_POINT('Ctrl Pts',(0.00278733463553876,-0.0347233226175679,
-0.013413563544606));
#31300=CARTESIAN_POINT('Ctrl Pts',(0.00291616377405434,-0.0347524202745288,
-0.0128801180399663));
#31301=CARTESIAN_POINT('Ctrl Pts',(0.00297180446698019,-0.0347649874143427,
-0.0126497254606296));
#31302=CARTESIAN_POINT('Ctrl Pts',(0.00299994245192145,-0.0347775545541565,
-0.0124129153826804));
#31303=CARTESIAN_POINT('Ctrl Pts',(0.00299999991133221,-0.0347901216939704,
-0.012176582674498));
#31304=CARTESIAN_POINT('Ctrl Pts',(0.00300013295148676,-0.0348192193509313,
-0.0116293835366518));
#31305=CARTESIAN_POINT('Ctrl Pts',(0.00284622122408974,-0.0348483170078922,
-0.0110803172019551));
#31306=CARTESIAN_POINT('Ctrl Pts',(0.00256014128152566,-0.0348774146648531,
-0.0106119873656339));
#31307=CARTESIAN_POINT('Ctrl Pts',(0.00243658471334654,-0.034889981804667,
-0.0104097179341138));
#31308=CARTESIAN_POINT('Ctrl Pts',(0.0022890386047289,-0.0349025489444808,
-0.0102223534133573));
#31309=CARTESIAN_POINT('Ctrl Pts',(0.00212196767400703,-0.0349151160842947,
-0.0100551804710419));
#31310=CARTESIAN_POINT('Ctrl Pts',(0.00173506291345904,-0.0349442192095328,
-0.00966803947088609));
#31311=CARTESIAN_POINT('Ctrl Pts',(0.00123787708173055,-0.034973322334771,
-0.0093885723356771));
#31312=CARTESIAN_POINT('Ctrl Pts',(0.000704333931740814,-0.0350024254600091,
-0.00925970622020521));
#31313=CARTESIAN_POINT('Ctrl Pts',(0.00047404272603916,-0.0350149871315457,
-0.00920408422766968));
#31314=CARTESIAN_POINT('Ctrl Pts',(0.000237337238801211,-0.0350275488030823,
-0.00917594025174976));
#31315=CARTESIAN_POINT('Ctrl Pts',(1.10181849570871E-6,-0.0350401104746189,
-0.0091758534888921));
#31316=CARTESIAN_POINT('Ctrl Pts',(-0.000544196126601482,-0.0350691063536748,
-0.00917565321575806));
#31317=CARTESIAN_POINT('Ctrl Pts',(-0.00109152410457655,-0.0350981022327307,
-0.00932846278863097));
#31318=CARTESIAN_POINT('Ctrl Pts',(-0.00155877106600548,-0.0351270981117866,
-0.00961260675846444));
#31319=CARTESIAN_POINT('Ctrl Pts',(-0.00176292122463022,-0.0351397670295055,
-0.00973675531651256));
#31320=CARTESIAN_POINT('Ctrl Pts',(-0.00195194004144232,-0.0351524359472243,
-0.00988529763263816));
#31321=CARTESIAN_POINT('Ctrl Pts',(-0.00212040937062949,-0.0351651048649432,
-0.0100536223611057));
#31322=CARTESIAN_POINT('Ctrl Pts',(-0.0025132296411,-0.0351946450056258,
-0.0104461054657901));
#31323=CARTESIAN_POINT('Ctrl Pts',(-0.00279498358199015,-0.0352241851463083,
-0.0109516626246059));
#31324=CARTESIAN_POINT('Ctrl Pts',(-0.0029215756990028,-0.0352537252869909,
-0.011494387634455));
#31325=CARTESIAN_POINT('Ctrl Pts',(-0.00297353502781077,-0.0352658499430831,
-0.0117171473757763));
#31326=CARTESIAN_POINT('Ctrl Pts',(-0.00299988733115571,-0.0352779745991753,
-0.011945842488321));
#31327=CARTESIAN_POINT('Ctrl Pts',(-0.00299999963776494,-0.0352900992552675,
-0.0121743790375236));
#31328=CARTESIAN_POINT('',(-0.00299998807114563,-0.0332900774868462,-0.0121782217945205));
#31329=CARTESIAN_POINT('Ctrl Pts',(-0.0029999990241015,-0.0332900992552675,
-0.012178273077878));
#31330=CARTESIAN_POINT('Ctrl Pts',(-0.00299954990966587,-0.033319643576341,
-0.0127350743431392));
#31331=CARTESIAN_POINT('Ctrl Pts',(-0.00283978743580498,-0.0333491878974145,
-0.0132918658231327));
#31332=CARTESIAN_POINT('Ctrl Pts',(-0.00254507661055699,-0.033378732218488,
-0.0137641180775787));
#31333=CARTESIAN_POINT('Ctrl Pts',(-0.00242415366009201,-0.0333908545640812,
-0.0139578881432805));
#31334=CARTESIAN_POINT('Ctrl Pts',(-0.00228111365948316,-0.0334029769096743,
-0.0141375956861433));
#31335=CARTESIAN_POINT('Ctrl Pts',(-0.0021198956782073,-0.0334150992552675,
-0.0142985973393157));
#31336=CARTESIAN_POINT('Ctrl Pts',(-0.00173421667443884,-0.033444099334134,
-0.0146837588250832));
#31337=CARTESIAN_POINT('Ctrl Pts',(-0.0012389737994231,-0.0334730994130005,
-0.0149622678449037));
#31338=CARTESIAN_POINT('Ctrl Pts',(-0.000707441773154454,-0.033502099491867,
-0.0150912479661163));
#31339=CARTESIAN_POINT('Ctrl Pts',(-0.000475280436272606,-0.0335147660796672,
-0.015147583607041));
#31340=CARTESIAN_POINT('Ctrl Pts',(-0.000236567380074324,-0.0335274326674673,
-0.0151759805508666));
#31341=CARTESIAN_POINT('Ctrl Pts',(1.60841856303651E-6,-0.0335400992552675,
-0.0151758528553897));
#31342=CARTESIAN_POINT('Ctrl Pts',(0.000548927193259567,-0.0335692065841986,
-0.0151755594161218));
#31343=CARTESIAN_POINT('Ctrl Pts',(0.00109797366274001,-0.0335983139131297,
-0.0150211546781943));
#31344=CARTESIAN_POINT('Ctrl Pts',(0.00156613626676192,-0.0336274212420608,
-0.014734606341062));
#31345=CARTESIAN_POINT('Ctrl Pts',(0.00176814079534584,-0.0336399805797964,
-0.0146109654067762));
#31346=CARTESIAN_POINT('Ctrl Pts',(0.00195524231623712,-0.033652539917532,
-0.0144633852168754));
#31347=CARTESIAN_POINT('Ctrl Pts',(0.0021221706331302,-0.0336650992552675,
-0.0142963229995886));
#31348=CARTESIAN_POINT('Ctrl Pts',(0.00250896839453303,-0.0336942011105502,
-0.0139092149710394));
#31349=CARTESIAN_POINT('Ctrl Pts',(0.00278805792401258,-0.033723302965833,
-0.0134119347801851));
#31350=CARTESIAN_POINT('Ctrl Pts',(0.00291657551373059,-0.0337524048211157,
-0.0128784109515986));
#31351=CARTESIAN_POINT('Ctrl Pts',(0.00297206336007698,-0.0337649696324996,
-0.0126480604736002));
#31352=CARTESIAN_POINT('Ctrl Pts',(0.00300006266320082,-0.0337775344438836,
-0.01241131275598));
#31353=CARTESIAN_POINT('Ctrl Pts',(0.00299999989411969,-0.0337900992552675,
-0.0121750562408696));
#31354=CARTESIAN_POINT('Ctrl Pts',(0.00299985451217487,-0.0338192011105503,
-0.0116278532067562));
#31355=CARTESIAN_POINT('Ctrl Pts',(0.00284566133290258,-0.033848302965833,
-0.0110788621567055));
#31356=CARTESIAN_POINT('Ctrl Pts',(0.00255933993882043,-0.0338774048211158,
-0.0106106762749844));
#31357=CARTESIAN_POINT('Ctrl Pts',(0.0024357198370479,-0.0338899696324997,
-0.0104085356472037));
#31358=CARTESIAN_POINT('Ctrl Pts',(0.00228813344676387,-0.0339025344438836,
-0.0102213024932187));
#31359=CARTESIAN_POINT('Ctrl Pts',(0.002121043592747,-0.0339150992552675,
-0.0100542562282864));
#31360=CARTESIAN_POINT('Ctrl Pts',(0.00173396740088748,-0.0339442065841986,
-0.00966728101381411));
#31361=CARTESIAN_POINT('Ctrl Pts',(0.00123665610771317,-0.0339733139131297,
-0.00938802977500934));
#31362=CARTESIAN_POINT('Ctrl Pts',(0.000703053329552393,-0.0340024212420608,
-0.00925939721526106));
#31363=CARTESIAN_POINT('Ctrl Pts',(0.00047281243306158,-0.0340149805797964,
-0.00920389436353972));
#31364=CARTESIAN_POINT('Ctrl Pts',(0.00023617348649114,-0.0340275399175319,
-0.00917585441442896));
#31365=CARTESIAN_POINT('Ctrl Pts',(1.43272443721777E-8,-0.0340400992552675,
-0.0091758532865923));
#31366=CARTESIAN_POINT('Ctrl Pts',(-0.000545287852488846,-0.034069099334134,
-0.00917585068236644));
#31367=CARTESIAN_POINT('Ctrl Pts',(-0.0010925637511624,-0.0340980994130005,
-0.00932886090342198));
#31368=CARTESIAN_POINT('Ctrl Pts',(-0.00155970950087997,-0.034127099491867,
-0.0096131776783578));
#31369=CARTESIAN_POINT('Ctrl Pts',(-0.0017637483478606,-0.0341397660796672,
-0.00973736090590557));
#31370=CARTESIAN_POINT('Ctrl Pts',(-0.00195265675439628,-0.0341524326674673,
-0.00988591653299666));
#31371=CARTESIAN_POINT('Ctrl Pts',(-0.00212102332822392,-0.0341650992552675,
-0.0100542359692433));
#31372=CARTESIAN_POINT('Ctrl Pts',(-0.00251373178244158,-0.034194643576341,
-0.0104468344768953));
#31373=CARTESIAN_POINT('Ctrl Pts',(-0.00279533977602888,-0.0342241878974145,
-0.0109524753987744));
#31374=CARTESIAN_POINT('Ctrl Pts',(-0.00292177413971409,-0.0342537322184881,
-0.0114952389489939));
#31375=CARTESIAN_POINT('Ctrl Pts',(-0.0029736514885835,-0.0342658545640812,
-0.0117179405407735));
#31376=CARTESIAN_POINT('Ctrl Pts',(-0.00299993700613952,-0.0342779769096744,
-0.01194656610685));
#31377=CARTESIAN_POINT('Ctrl Pts',(-0.00299999988636987,-0.0342900992552675,
-0.0121750275863819));
#31378=CARTESIAN_POINT('',(-0.00299999923530355,-0.0322900992552675,-0.0121737112832657));
#31379=CARTESIAN_POINT('Ctrl Pts',(-0.00299928376163152,-0.0322889717262675,
-0.0121758863199214));
#31380=CARTESIAN_POINT('Ctrl Pts',(-0.00299707236492287,-0.0323173669008297,
-0.012733832497412));
#31381=CARTESIAN_POINT('Ctrl Pts',(-0.00284002430592934,-0.0323491139306059,
-0.0132916136153277));
#31382=CARTESIAN_POINT('Ctrl Pts',(-0.00254536692236663,-0.0323804597583334,
-0.0137653979546681));
#31383=CARTESIAN_POINT('Ctrl Pts',(-0.00249618206423861,-0.0323856920727965,
-0.0138444830779797));
#31384=CARTESIAN_POINT('Ctrl Pts',(-0.0024433588192564,-0.0323907730793508,
-0.0139212959050287));
#31385=CARTESIAN_POINT('Ctrl Pts',(-0.00238695367579395,-0.032395720501742,
-0.0139953450637139));
#31386=CARTESIAN_POINT('Ctrl Pts',(-0.00230563882969713,-0.032402852810351,
-0.0141020958947989));
#31387=CARTESIAN_POINT('Ctrl Pts',(-0.00221687403707554,-0.0324097074948069,
-0.0142030993270911));
#31388=CARTESIAN_POINT('Ctrl Pts',(-0.00212192556767052,-0.0324163376568695,
-0.014297658716942));
#31389=CARTESIAN_POINT('Ctrl Pts',(-0.00173712109141055,-0.0324432081904971,
-0.0146808863425696));
#31390=CARTESIAN_POINT('Ctrl Pts',(-0.00124386889560183,-0.0324704443965446,
-0.0149566887355417));
#31391=CARTESIAN_POINT('Ctrl Pts',(-0.000715762144362272,-0.0325008177702179,
-0.0150883592010786));
#31392=CARTESIAN_POINT('Ctrl Pts',(-0.000481664421721094,-0.0325142815965923,
-0.0151467257264998));
#31393=CARTESIAN_POINT('Ctrl Pts',(-0.000240658071332929,-0.0325283955544535,
-0.0151765843830709));
#31394=CARTESIAN_POINT('Ctrl Pts',(-1.19791577169947E-7,-0.032541788645564,
-0.0151769364537194));
#31395=CARTESIAN_POINT('Ctrl Pts',(6.94614908600466E-5,-0.0325456629081396,
-0.0151770382983292));
#31396=CARTESIAN_POINT('Ctrl Pts',(0.000139033018747938,-0.0325494372625684,
-0.0151747452494295));
#31397=CARTESIAN_POINT('Ctrl Pts',(0.000208448528243256,-0.0325531337590053,
-0.0151699393817332));
#31398=CARTESIAN_POINT('Ctrl Pts',(0.000683492535792095,-0.0325784306774321,
-0.0151370504975804));
#31399=CARTESIAN_POINT('Ctrl Pts',(0.00115287566896183,-0.0326000812500363,
-0.0149853965230064));
#31400=CARTESIAN_POINT('Ctrl Pts',(0.00156079505898092,-0.0326251526157813,
-0.0147365832276358));
#31401=CARTESIAN_POINT('Ctrl Pts',(0.00176417689901714,-0.0326376527827804,
-0.0146125290466478));
#31402=CARTESIAN_POINT('Ctrl Pts',(0.00195273924601373,-0.0326508722292597,
-0.0144645794174125));
#31403=CARTESIAN_POINT('Ctrl Pts',(0.00212112665312921,-0.0326644232833442,
-0.0142969471212208));
#31404=CARTESIAN_POINT('Ctrl Pts',(0.00231445119514261,-0.0326799811648364,
-0.0141044895173947));
#31405=CARTESIAN_POINT('Ctrl Pts',(0.00248237593275498,-0.0326956646976751,
-0.0138857000773177));
#31406=CARTESIAN_POINT('Ctrl Pts',(0.00261628761582927,-0.0327103721403783,
-0.0136471685813781));
#31407=CARTESIAN_POINT('Ctrl Pts',(0.00267475686196265,-0.032716793783865,
-0.0135430196645213));
#31408=CARTESIAN_POINT('Ctrl Pts',(0.00272676038214198,-0.0327230293438048,
-0.0134350970847119));
#31409=CARTESIAN_POINT('Ctrl Pts',(0.00277240400992479,-0.0327289871122913,
-0.0133243027587875));
#31410=CARTESIAN_POINT('Ctrl Pts',(0.00284749445580838,-0.0327387885131408,
-0.0131420298821745));
#31411=CARTESIAN_POINT('Ctrl Pts',(0.00290434841955195,-0.0327482951808992,
-0.0129517210769552));
#31412=CARTESIAN_POINT('Ctrl Pts',(0.00294186480225773,-0.0327579060333934,
-0.0127609850341249));
#31413=CARTESIAN_POINT('Ctrl Pts',(0.00296062299361062,-0.0327627114596405,
-0.0126656170127098));
#31414=CARTESIAN_POINT('Ctrl Pts',(0.00297478607666181,-0.0327675320197591,
-0.0125702102217573));
#31415=CARTESIAN_POINT('Ctrl Pts',(0.0029845603754328,-0.0327726924870258,
-0.0124697194406367));
#31416=CARTESIAN_POINT('Ctrl Pts',(0.00299433467420379,-0.0327778529542926,
-0.0123692286595161));
#31417=CARTESIAN_POINT('Ctrl Pts',(0.00299882345649107,-0.0327833774686131,
-0.0122635383972968));
#31418=CARTESIAN_POINT('Ctrl Pts',(0.00299882727697248,-0.0327880563174707,
-0.0121757451535895));
#31419=CARTESIAN_POINT('Ctrl Pts',(0.00299883109745389,-0.0327927351663284,
-0.0120879519098822));
#31420=CARTESIAN_POINT('Ctrl Pts',(0.00299567769338781,-0.0327965359930861,
-0.012018041578474));
#31421=CARTESIAN_POINT('Ctrl Pts',(0.00298989568302409,-0.0328006876304326,
-0.0119428049059826));
#31422=CARTESIAN_POINT('Ctrl Pts',(0.00298411367266037,-0.0328048392677792,
-0.0118675682334912));
#31423=CARTESIAN_POINT('Ctrl Pts',(0.00297496288616724,-0.032809356386336,
-0.0117870879822373));
#31424=CARTESIAN_POINT('Ctrl Pts',(0.00296250651140142,-0.03281391386738,
-0.0117073372799718));
#31425=CARTESIAN_POINT('Ctrl Pts',(0.00293759376186978,-0.032823028829468,
-0.0115478358754407));
#31426=CARTESIAN_POINT('Ctrl Pts',(0.00290023790677386,-0.0328323084983074,
-0.0113910507489261));
#31427=CARTESIAN_POINT('Ctrl Pts',(0.00284915939399223,-0.0328416873337566,
-0.0112351214523587));
#31428=CARTESIAN_POINT('Ctrl Pts',(0.00280089480223856,-0.0328505494881035,
-0.0110877823183193));
#31429=CARTESIAN_POINT('Ctrl Pts',(0.00274055321868181,-0.0328592599446676,
-0.0109411939081582));
#31430=CARTESIAN_POINT('Ctrl Pts',(0.00266693795030175,-0.0328677954873264,
-0.0107985473240077));
#31431=CARTESIAN_POINT('Ctrl Pts',(0.00258473885082951,-0.0328773263079768,
-0.010639267584655));
#31432=CARTESIAN_POINT('Ctrl Pts',(0.00248593869287483,-0.0328866390452035,
-0.0104849338592383));
#31433=CARTESIAN_POINT('Ctrl Pts',(0.00237225614196163,-0.0328957013778296,
-0.0103388482527745));
#31434=CARTESIAN_POINT('Ctrl Pts',(0.00215676260346663,-0.0329128796880359,
-0.0100619323672036));
#31435=CARTESIAN_POINT('Ctrl Pts',(0.00188566631662303,-0.0329304353752007,
-0.0098149684751571));
#31436=CARTESIAN_POINT('Ctrl Pts',(0.00156935168882271,-0.0329504815267945,
-0.00962048083750371));
#31437=CARTESIAN_POINT('Ctrl Pts',(0.00125303706102239,-0.0329705276783882,
-0.00942599319985031));
#31438=CARTESIAN_POINT('Ctrl Pts',(0.000891738231477182,-0.0329932455839496,
-0.00928410707949561));
#31439=CARTESIAN_POINT('Ctrl Pts',(0.00050374597097403,-0.0330150737761611,
-0.00921745827629187));
#31440=CARTESIAN_POINT('Ctrl Pts',(0.000441300376803264,-0.0330185869246723,
-0.00920673145377373));
#31441=CARTESIAN_POINT('Ctrl Pts',(0.000378291871362253,-0.0330220258529512,
-0.00919792040728071));
#31442=CARTESIAN_POINT('Ctrl Pts',(0.000314806651507004,-0.0330254091399757,
-0.00919118498220827));
#31443=CARTESIAN_POINT('Ctrl Pts',(-0.000134903341485572,-0.0330493753164735,
-0.0091434732790901));
#31444=CARTESIAN_POINT('Ctrl Pts',(-0.000611424908498898,-0.0330705494844869,
-0.00920099273624149));
#31445=CARTESIAN_POINT('Ctrl Pts',(-0.00105907198302849,-0.0330955355600564,
-0.00937022262920045));
#31446=CARTESIAN_POINT('Ctrl Pts',(-0.00133351553764533,-0.0331108540280759,
-0.00947397412454952));
#31447=CARTESIAN_POINT('Ctrl Pts',(-0.00159729233888611,-0.033127593814194,
-0.00961938212286541));
#31448=CARTESIAN_POINT('Ctrl Pts',(-0.00183679345966173,-0.0331449433303733,
-0.00980394576024457));
#31449=CARTESIAN_POINT('Ctrl Pts',(-0.00201242281432988,-0.0331576659611506,
-0.00993928872825712));
#31450=CARTESIAN_POINT('Ctrl Pts',(-0.00217675104965253,-0.0331699846688671,
-0.0100954580292239));
#31451=CARTESIAN_POINT('Ctrl Pts',(-0.00232166018894287,-0.0331820424692315,
-0.0102718389100069));
#31452=CARTESIAN_POINT('Ctrl Pts',(-0.00251064840497445,-0.0331977680624638,
-0.0105018720753718));
#31453=CARTESIAN_POINT('Ctrl Pts',(-0.00266639130070364,-0.0332130498792843,
-0.0107665103491488));
#31454=CARTESIAN_POINT('Ctrl Pts',(-0.00278109594182748,-0.0332282051689312,
-0.0110521365491834));
#31455=CARTESIAN_POINT('Ctrl Pts',(-0.00292162366242661,-0.0332467723192073,
-0.0114020648384051));
#31456=CARTESIAN_POINT('Ctrl Pts',(-0.00299867836658016,-0.0332669737194449,
-0.0117854146205141));
#31457=CARTESIAN_POINT('Ctrl Pts',(-0.00299949806419125,-0.0332891036239059,
-0.0121759275095697));
#31458=CARTESIAN_POINT('',(-0.00299999999422887,-0.0312900992552675,-0.012176039369213));
#31459=CARTESIAN_POINT('Ctrl Pts',(-0.00299999999422887,-0.0312900992552675,
-0.012176039369213));
#31460=CARTESIAN_POINT('Ctrl Pts',(-0.00299996545726101,-0.0313196420846964,
-0.012732839805292));
#31461=CARTESIAN_POINT('Ctrl Pts',(-0.0028406181462586,-0.0313491849141254,
-0.0132897492385463));
#31462=CARTESIAN_POINT('Ctrl Pts',(-0.0025462599484267,-0.0313787277435543,
-0.0137622202917111));
#31463=CARTESIAN_POINT('Ctrl Pts',(-0.00242546072407741,-0.031390851580792,
-0.0139561137764863));
#31464=CARTESIAN_POINT('Ctrl Pts',(-0.00228252633754426,-0.0314029754180298,
-0.0141359563616402));
#31465=CARTESIAN_POINT('Ctrl Pts',(-0.002121394537641,-0.0314150992552675,
-0.0142970994334413));
#31466=CARTESIAN_POINT('Ctrl Pts',(-0.00173598925954655,-0.0314440978195793,
-0.0146825316723773));
#31467=CARTESIAN_POINT('Ctrl Pts',(-0.00124094532465347,-0.0314730963838911,
-0.0149613900299818));
#31468=CARTESIAN_POINT('Ctrl Pts',(-0.000709506489134427,-0.0315020949482029,
-0.0150907461734197));
#31469=CARTESIAN_POINT('Ctrl Pts',(-0.000477345976244627,-0.0315147630505578,
-0.0151472557594695));
#31470=CARTESIAN_POINT('Ctrl Pts',(-0.000238611731454913,-0.0315274311529127,
-0.0151758218207988));
#31471=CARTESIAN_POINT('Ctrl Pts',(-3.95938876176992E-7,-0.0315400992552675,
-0.0151758532604302));
#31472=CARTESIAN_POINT('Ctrl Pts',(0.000546920822706506,-0.0315692050701306,
-0.0151759254950919));
#31473=CARTESIAN_POINT('Ctrl Pts',(0.0010960686685288,-0.0315983108849936,
-0.0150218887442718));
#31474=CARTESIAN_POINT('Ctrl Pts',(0.0015644217207454,-0.0316274166998567,
-0.014735654974123));
#31475=CARTESIAN_POINT('Ctrl Pts',(0.00176654330051676,-0.0316399775516603,
-0.0146121284559705));
#31476=CARTESIAN_POINT('Ctrl Pts',(0.00195377283282597,-0.0316525384034639,
-0.0144646445384834));
#31477=CARTESIAN_POINT('Ctrl Pts',(0.0021208345411987,-0.0316650992552675,
-0.0142976593212508));
#31478=CARTESIAN_POINT('Ctrl Pts',(0.00250787462741079,-0.0316941995991603,
-0.0139107964458297));
#31479=CARTESIAN_POINT('Ctrl Pts',(0.00278727696472124,-0.0317232999430531,
-0.0134136940661085));
#31480=CARTESIAN_POINT('Ctrl Pts',(0.00291613115480297,-0.0317524002869459,
-0.0128802530934771));
#31481=CARTESIAN_POINT('Ctrl Pts',(0.00297177391109823,-0.0317649666097197,
-0.0126498987214601));
#31482=CARTESIAN_POINT('Ctrl Pts',(0.00299992281111363,-0.0317775329324936,
-0.0124131275687113));
#31483=CARTESIAN_POINT('Ctrl Pts',(0.00299999984059891,-0.0317900992552675,
-0.0121768312469505));
#31484=CARTESIAN_POINT('Ctrl Pts',(0.00300017822090568,-0.0318191995991603,
-0.0116296302600293));
#31485=CARTESIAN_POINT('Ctrl Pts',(0.00284631098608129,-0.0318482999430531,
-0.011080549694383));
#31486=CARTESIAN_POINT('Ctrl Pts',(0.00256026832300205,-0.0318774002869458,
-0.0106121953590585));
#31487=CARTESIAN_POINT('Ctrl Pts',(0.00243674729367678,-0.0318899666097197,
-0.0104099471735415));
#31488=CARTESIAN_POINT('Ctrl Pts',(0.00228924297230858,-0.0319025329324936,
-0.010222597311479));
#31489=CARTESIAN_POINT('Ctrl Pts',(0.00212221745188226,-0.0319150992552675,
-0.0100554304308695));
#31490=CARTESIAN_POINT('Ctrl Pts',(0.00173535695478928,-0.0319442050701306,
-0.00966824251871701));
#31491=CARTESIAN_POINT('Ctrl Pts',(0.00123820225068015,-0.0319733108849936,
-0.00938871647213873));
#31492=CARTESIAN_POINT('Ctrl Pts',(0.000704672593883375,-0.0320024166998567,
-0.00925978803772882));
#31493=CARTESIAN_POINT('Ctrl Pts',(0.000474423518797268,-0.0320149775516603,
-0.00920414792026393));
#31494=CARTESIAN_POINT('Ctrl Pts',(0.00023775896460552,-0.0320275384034639,
-0.00917597651420902));
#31495=CARTESIAN_POINT('Ctrl Pts',(1.55998187177509E-6,-0.0320400992552675,
-0.00917585369214869));
#31496=CARTESIAN_POINT('Ctrl Pts',(-0.000543739930768506,-0.0320690978195793,
-0.00917557013945089));
#31497=CARTESIAN_POINT('Ctrl Pts',(-0.00109109283963647,-0.0320980963838911,
-0.00932829719717779));
#31498=CARTESIAN_POINT('Ctrl Pts',(-0.00155838406046309,-0.0321270949482029,
-0.00961237145122268));
#31499=CARTESIAN_POINT('Ctrl Pts',(-0.0017625215119349,-0.0321397630505578,
-0.00973647006824121));
#31500=CARTESIAN_POINT('Ctrl Pts',(-0.00195153599591617,-0.0321524311529126,
-0.0098849571721927));
#31501=CARTESIAN_POINT('Ctrl Pts',(-0.0021200110903683,-0.0321650992552675,
-0.010053224497364));
#31502=CARTESIAN_POINT('Ctrl Pts',(-0.00251290584595237,-0.0321946420846964,
-0.0104456347216228));
#31503=CARTESIAN_POINT('Ctrl Pts',(-0.00279475481519703,-0.0322241849141254,
-0.0109511400793834));
#31504=CARTESIAN_POINT('Ctrl Pts',(-0.00292144843250678,-0.0322537277435543,
-0.0114938422483749));
#31505=CARTESIAN_POINT('Ctrl Pts',(-0.00297344117744736,-0.032265851580792,
-0.0117165572994583));
#31506=CARTESIAN_POINT('Ctrl Pts',(-0.0029998360855368,-0.0322779754180298,
-0.0119452106188514));
#31507=CARTESIAN_POINT('Ctrl Pts',(-0.00299999923530355,-0.0322900992552675,
-0.0121737112832657));
#31508=CARTESIAN_POINT('Ctrl Pts',(-0.00112535951647366,-0.0304787743898623,
-0.0149567822606029));
#31509=CARTESIAN_POINT('Ctrl Pts',(-0.000605826549099741,-0.0305085119470451,
-0.0151670218511904));
#31510=CARTESIAN_POINT('Ctrl Pts',(-2.6152100817094E-5,-0.0305382495042279,
-0.0152275772346542));
#31511=CARTESIAN_POINT('Ctrl Pts',(0.000525287215145681,-0.0305679870614107,
-0.015129507521841));
#31512=CARTESIAN_POINT('Ctrl Pts',(0.000600707865615942,-0.0305720542830272,
-0.0151160944747156));
#31513=CARTESIAN_POINT('Ctrl Pts',(0.000675597023227879,-0.0305761215046438,
-0.0150997942648813));
#31514=CARTESIAN_POINT('Ctrl Pts',(0.000749732422933762,-0.0305801887262604,
-0.0150806598711695));
#31515=CARTESIAN_POINT('Ctrl Pts',(0.00128509963884293,-0.0306095600808629,
-0.0149424812529891));
#31516=CARTESIAN_POINT('Ctrl Pts',(0.00178186922311124,-0.0306389314354654,
-0.0146519824220399));
#31517=CARTESIAN_POINT('Ctrl Pts',(0.00216497392884224,-0.0306683027900679,
-0.0142526026425068));
#31518=CARTESIAN_POINT('Ctrl Pts',(0.00222280121312341,-0.0306727362142648,
-0.0141923187365622));
#31519=CARTESIAN_POINT('Ctrl Pts',(0.00227809198190826,-0.0306771696384616,
-0.0141296356243967));
#31520=CARTESIAN_POINT('Ctrl Pts',(0.00233065306415271,-0.0306816030626585,
-0.0140647832202919));
#31521=CARTESIAN_POINT('Ctrl Pts',(0.00267983604782405,-0.0307110559624626,
-0.0136339443753407));
#31522=CARTESIAN_POINT('Ctrl Pts',(0.00290653022343286,-0.0307405088622667,
-0.0131032252539013));
#31523=CARTESIAN_POINT('Ctrl Pts',(0.00297623693573143,-0.0307699617620708,
-0.0125527003409289));
#31524=CARTESIAN_POINT('Ctrl Pts',(0.00298653660670087,-0.0307743136410661,
-0.0124713563027851));
#31525=CARTESIAN_POINT('Ctrl Pts',(0.00299349653931312,-0.0307786655200613,
-0.0123896120634787));
#31526=CARTESIAN_POINT('Ctrl Pts',(0.00299709913212865,-0.0307830173990565,
-0.012307750186422));
#31527=CARTESIAN_POINT('Ctrl Pts',(0.00302147207072706,-0.0308124595494659,
-0.0117539228167411));
#31528=CARTESIAN_POINT('Ctrl Pts',(0.00288808641085541,-0.0308419016998753,
-0.0111926614903797));
#31529=CARTESIAN_POINT('Ctrl Pts',(0.0026168203245709,-0.0308713438502847,
-0.0107087979403245));
#31530=CARTESIAN_POINT('Ctrl Pts',(0.00257662512439674,-0.0308757064786746,
-0.0106371008383467));
#31531=CARTESIAN_POINT('Ctrl Pts',(0.00253349270277464,-0.0308800691070646,
-0.0105670767113343));
#31532=CARTESIAN_POINT('Ctrl Pts',(0.00248757826106265,-0.0308844317354546,
-0.0104989649792792));
#31533=CARTESIAN_POINT('Ctrl Pts',(0.00217771462428059,-0.030913873885864,
-0.0100392980811281));
#31534=CARTESIAN_POINT('Ctrl Pts',(0.00173661880752667,-0.0309433160362734,
-0.00966749296217343));
#31535=CARTESIAN_POINT('Ctrl Pts',(0.00123072528973799,-0.0309727581866828,
-0.00943992286690203));
#31536=CARTESIAN_POINT('Ctrl Pts',(0.00115576386904273,-0.0309771208150727,
-0.00940620237622671));
#31537=CARTESIAN_POINT('Ctrl Pts',(0.00107943649137909,-0.0309814834434627,
-0.00937557394026337));
#31538=CARTESIAN_POINT('Ctrl Pts',(0.00100201033104887,-0.0309858460718527,
-0.00934813772510723));
#31539=CARTESIAN_POINT('Ctrl Pts',(0.000479292203677936,-0.0310152989716568,
-0.00916291083348046));
#31540=CARTESIAN_POINT('Ctrl Pts',(-9.66640762191366E-5,-0.031044751871461,
-0.00912649295579771));
#31541=CARTESIAN_POINT('Ctrl Pts',(-0.000638860917020236,-0.0310742047712651,
-0.00924466637189296));
#31542=CARTESIAN_POINT('Ctrl Pts',(-0.000718974422259154,-0.0310785566502604,
-0.00926212734893491));
#31543=CARTESIAN_POINT('Ctrl Pts',(-0.000798349784612914,-0.0310829085292556,
-0.00928287002814561));
#31544=CARTESIAN_POINT('Ctrl Pts',(-0.000876714771932716,-0.0310872604082508,
-0.00930681665230697));
#31545=CARTESIAN_POINT('Ctrl Pts',(-0.00140560949384823,-0.0311166317628533,
-0.0094684352980799));
#31546=CARTESIAN_POINT('Ctrl Pts',(-0.00188910772167505,-0.0311460031174558,
-0.00978055728136447));
#31547=CARTESIAN_POINT('Ctrl Pts',(-0.00225421567954084,-0.0311753744720583,
-0.0101963301949746));
#31548=CARTESIAN_POINT('Ctrl Pts',(-0.00230932646611429,-0.0311798078962552,
-0.0102590885430504));
#31549=CARTESIAN_POINT('Ctrl Pts',(-0.00236179690657229,-0.031184241320452,
-0.0103241295731634));
#31550=CARTESIAN_POINT('Ctrl Pts',(-0.00241144471782708,-0.0311886747446489,
-0.0103912148433815));
#31551=CARTESIAN_POINT('Ctrl Pts',(-0.00274446149236254,-0.0312184123018317,
-0.0108411948070944));
#31552=CARTESIAN_POINT('Ctrl Pts',(-0.00294825228095729,-0.0312481498590144,
-0.011387140196714));
#31553=CARTESIAN_POINT('Ctrl Pts',(-0.0029911879473685,-0.0312778874161972,
-0.0119460823930198));
#31554=CARTESIAN_POINT('Ctrl Pts',(-0.0029970602814502,-0.0312819546378138,
-0.0120225292164516));
#31555=CARTESIAN_POINT('Ctrl Pts',(-0.00299999988367143,-0.0312860218594304,
-0.0120991943468039));
#31556=CARTESIAN_POINT('Ctrl Pts',(-0.00299999999999654,-0.031290089081047,
-0.0121758487339766));
#31557=CARTESIAN_POINT('Ctrl Pts',(-0.00176573724564316,-0.0405768567115634,
-0.0104108332259136));
#31558=CARTESIAN_POINT('Ctrl Pts',(-0.00118375689512938,-0.0405243778792318,
-0.00982859805607285));
#31559=CARTESIAN_POINT('Ctrl Pts',(0.000590938148187802,-0.0404194309906651,
-0.00929427447494101));
#31560=CARTESIAN_POINT('Ctrl Pts',(0.002736334709133,-0.0402620160458629,
-0.0110892695029399));
#31561=CARTESIAN_POINT('Ctrl Pts',(0.00240943420965453,-0.040104611877157,
-0.0138634638989389));
#31562=CARTESIAN_POINT('Ctrl Pts',(-8.4854924110494E-5,-0.039947207708451,
-0.0151169866770628));
#31563=CARTESIAN_POINT('Ctrl Pts',(-0.00250442120103688,-0.039789803539745,
-0.013720818532592));
#31564=CARTESIAN_POINT('Ctrl Pts',(-0.00266674786335135,-0.039632399371039,
-0.0109326563015306));
#31565=CARTESIAN_POINT('Ctrl Pts',(-0.000426928585076152,-0.039474995202333,
-0.00926458117117055));
#31566=CARTESIAN_POINT('Ctrl Pts',(0.00219776514813444,-0.039317591033627,
-0.0102193949058226));
#31567=CARTESIAN_POINT('Ctrl Pts',(0.00284226643201514,-0.039160186864921,
-0.0129368842307664));
#31568=CARTESIAN_POINT('Ctrl Pts',(0.000926095137602526,-0.0390027826962151,
-0.014968719980181));
#31569=CARTESIAN_POINT('Ctrl Pts',(-0.00182447151375588,-0.0388453785275091,
-0.0144843301313878));
#31570=CARTESIAN_POINT('Ctrl Pts',(-0.00293126780897562,-0.0386879743588031,
-0.0119201214729091));
#31571=CARTESIAN_POINT('Ctrl Pts',(-0.00139715250182972,-0.0385305701900971,
-0.00958631446602781));
#31572=CARTESIAN_POINT('Ctrl Pts',(0.00139572892480361,-0.0383731660213911,
-0.00958554709051689));
#31573=CARTESIAN_POINT('Ctrl Pts',(0.00293112889605655,-0.0382157618526851,
-0.0119185111592916));
#31574=CARTESIAN_POINT('Ctrl Pts',(0.00182573516943588,-0.0380583576839792,
-0.0144833270353835));
#31575=CARTESIAN_POINT('Ctrl Pts',(-0.000924551666121453,-0.0379009535152732,
-0.0149692289983903));
#31576=CARTESIAN_POINT('Ctrl Pts',(-0.00284186518882352,-0.0377435493465672,
-0.0129384445659896));
#31577=CARTESIAN_POINT('Ctrl Pts',(-0.00219880599194375,-0.0375861451778613,
-0.010220605025049));
#31578=CARTESIAN_POINT('Ctrl Pts',(0.000425263234877395,-0.0374287410091553,
-0.00926434256914682));
#31579=CARTESIAN_POINT('Ctrl Pts',(0.00266619234260643,-0.0372713368404493,
-0.010931199992661));
#31580=CARTESIAN_POINT('Ctrl Pts',(0.00250502070384008,-0.0371139326717433,
-0.0137194253613483));
#31581=CARTESIAN_POINT('Ctrl Pts',(8.69555590101293E-5,-0.0369565285030373,
-0.0151169724941598));
#31582=CARTESIAN_POINT('Ctrl Pts',(-0.00240945202080823,-0.0367991243343313,
-0.0138647240387452));
#31583=CARTESIAN_POINT('Ctrl Pts',(-0.00273506852592541,-0.0366417201656253,
-0.0110908907881794));
#31584=CARTESIAN_POINT('Ctrl Pts',(-0.000596530399695241,-0.0364843159969194,
-0.0092945523747685));
#31585=CARTESIAN_POINT('Ctrl Pts',(0.00207945062066594,-0.0363269118282134,
-0.0100941163728396));
#31586=CARTESIAN_POINT('Ctrl Pts',(0.00288195467878527,-0.0361695076595074,
-0.0127692171647587));
#31587=CARTESIAN_POINT('Ctrl Pts',(0.00108796731518194,-0.0360121034908014,
-0.0149097279331455));
#31588=CARTESIAN_POINT('Ctrl Pts',(-0.00168622206938664,-0.0358546993220954,
-0.014587159694891));
#31589=CARTESIAN_POINT('Ctrl Pts',(-0.00294121298424043,-0.0356972951533894,
-0.0120921296722862));
#31590=CARTESIAN_POINT('Ctrl Pts',(-0.00154632382334315,-0.0355398909846835,
-0.00967253027592494));
#31591=CARTESIAN_POINT('Ctrl Pts',(0.00124172275662489,-0.0353824868159775,
-0.00950829484148566));
#31592=CARTESIAN_POINT('Ctrl Pts',(0.00291104165179871,-0.0352250826472715,
-0.0117473909618462));
#31593=CARTESIAN_POINT('Ctrl Pts',(0.00195766327410342,-0.0350676784785655,
-0.0143725093742236));
#31594=CARTESIAN_POINT('Ctrl Pts',(-0.000759467994954353,-0.0349102743098595,
-0.0150185547880869));
#31595=CARTESIAN_POINT('Ctrl Pts',(-0.00279235806187805,-0.0347528701411535,
-0.0131034738536127));
#31596=CARTESIAN_POINT('Ctrl Pts',(-0.00230947860380213,-0.0345954659724475,
-0.0103526549865628));
#31597=CARTESIAN_POINT('Ctrl Pts',(0.000254121077754658,-0.0344380618037416,
-0.00924444305604325));
#31598=CARTESIAN_POINT('Ctrl Pts',(0.0025887708719542,-0.0342806576350356,
-0.0107772794291727));
#31599=CARTESIAN_POINT('Ctrl Pts',(0.00259107262143253,-0.0341232534663297,
-0.0135701581796352));
#31600=CARTESIAN_POINT('Ctrl Pts',(0.000258952568197248,-0.0339658492976236,
-0.0151068406672191));
#31601=CARTESIAN_POINT('Ctrl Pts',(-0.00230647029233221,-0.0338084451289177,
-0.0140028558188922));
#31602=CARTESIAN_POINT('Ctrl Pts',(-0.00279388326509801,-0.0336510409602117,
-0.011252836614041));
#31603=CARTESIAN_POINT('Ctrl Pts',(-0.000764152577578523,-0.0334936367915057,
-0.00933440748064133));
#31604=CARTESIAN_POINT('Ctrl Pts',(0.00195403986518134,-0.0333362326227997,
-0.00997597336214831));
#31605=CARTESIAN_POINT('Ctrl Pts',(0.00291174394389237,-0.0331788284540937,
-0.0125995167845713));
#31606=CARTESIAN_POINT('Ctrl Pts',(0.00124611797408996,-0.0330214242853877,
-0.014841361344239));
#31607=CARTESIAN_POINT('Ctrl Pts',(-0.00154219545170772,-0.0328640201166818,
-0.0146817217666492));
#31608=CARTESIAN_POINT('Ctrl Pts',(-0.00294107108454518,-0.0327066159479758,
-0.0122644246480997));
#31609=CARTESIAN_POINT('Ctrl Pts',(-0.00169019413996331,-0.0325492117792698,
-0.00976732980836716));
#31610=CARTESIAN_POINT('Ctrl Pts',(0.00108345923042443,-0.0323918076105638,
-0.00944018855622451));
#31611=CARTESIAN_POINT('Ctrl Pts',(0.00288097343976189,-0.0322344034418578,
-0.011577740875895));
#31612=CARTESIAN_POINT('Ctrl Pts',(0.00208287772409016,-0.0320769992731518,
-0.0142541579117125));
#31613=CARTESIAN_POINT('Ctrl Pts',(-0.000591777636590497,-0.0319195951044459,
-0.0150581372552976));
#31614=CARTESIAN_POINT('Ctrl Pts',(-0.0027332817459633,-0.0317621909357399,
-0.013265315295727));
#31615=CARTESIAN_POINT('Ctrl Pts',(-0.00241222224189072,-0.0316047867670339,
-0.0104909703753948));
#31616=CARTESIAN_POINT('Ctrl Pts',(8.20876226880905E-5,-0.0314473825983279,
-0.00923456740040116));
#31617=CARTESIAN_POINT('Ctrl Pts',(0.00250251191094569,-0.0312899784296219,
-0.0106282074995115));
#31618=CARTESIAN_POINT('Ctrl Pts',(0.00266816463044997,-0.031132574260916,
-0.0134160066702516));
#31619=CARTESIAN_POINT('Ctrl Pts',(0.000430208913922906,-0.03097517009221,
-0.0150868605785511));
#31620=CARTESIAN_POINT('Ctrl Pts',(-0.00219586682886496,-0.030817765923504,
-0.0141343309731242));
#31621=CARTESIAN_POINT('Ctrl Pts',(-0.00284255863625992,-0.030660361754798,
-0.011418711827452));
#31622=CARTESIAN_POINT('Ctrl Pts',(-0.000930263045673305,-0.0305029575860921,
-0.00938250357249028));
#31623=CARTESIAN_POINT('Ctrl Pts',(0.00182468775185338,-0.0303455303363401,
-0.00986851078086045));
#31624=CARTESIAN_POINT('Ctrl Pts',(0.00255836733623353,-0.0302405711428233,
-0.0115708398779804));
#31625=CARTESIAN_POINT('Ctrl Pts',(0.00248731861744851,-0.0301880800055419,
-0.0123911899040882));
#31626=CARTESIAN_POINT('Ctrl Pts',(-0.00188644671560341,-0.0406753955675595,
-0.0102901727842112));
#31627=CARTESIAN_POINT('Ctrl Pts',(-0.00126468097810125,-0.0406229167352281,
-0.00966813480740289));
#31628=CARTESIAN_POINT('Ctrl Pts',(0.000631335908853008,-0.0405179698466612,
-0.00909728375513973));
#31629=CARTESIAN_POINT('Ctrl Pts',(0.0029233962400536,-0.0403605549018591,
-0.0110149883759423));
#31630=CARTESIAN_POINT('Ctrl Pts',(0.00257414814264154,-0.0402031507331532,
-0.0139788324697851));
#31631=CARTESIAN_POINT('Ctrl Pts',(-9.0655783178371E-5,-0.0400457465644472,
-0.0153180486717205));
#31632=CARTESIAN_POINT('Ctrl Pts',(-0.00267562864228014,-0.0398883423957412,
-0.0138264355695641));
#31633=CARTESIAN_POINT('Ctrl Pts',(-0.00284905229278846,-0.0397309382270353,
-0.0108476687704077));
#31634=CARTESIAN_POINT('Ctrl Pts',(-0.000456114310949391,-0.0395735340583293,
-0.00906556055537634));
#31635=CARTESIAN_POINT('Ctrl Pts',(0.00234800894391053,-0.0394161298896233,
-0.0100856473424632));
#31636=CARTESIAN_POINT('Ctrl Pts',(0.00303656967579679,-0.0392587257209173,
-0.0129889098886754));
#31637=CARTESIAN_POINT('Ctrl Pts',(0.00098940492702264,-0.0391013215522113,
-0.0151596461551195));
#31638=CARTESIAN_POINT('Ctrl Pts',(-0.00194919618042227,-0.0389439173835053,
-0.0146421424089747));
#31639=CARTESIAN_POINT('Ctrl Pts',(-0.00313165537196454,-0.0387865132147993,
-0.0119026391143341));
#31640=CARTESIAN_POINT('Ctrl Pts',(-0.0014926647522315,-0.0386291090460934,
-0.00940928820731397));
#31641=CARTESIAN_POINT('Ctrl Pts',(0.00149114385651963,-0.0384717048773874,
-0.00940846837241741));
#31642=CARTESIAN_POINT('Ctrl Pts',(0.00313150696266941,-0.0383143007086814,
-0.0119009187163291));
#31643=CARTESIAN_POINT('Ctrl Pts',(0.00195054622223225,-0.0381568965399754,
-0.0146410707392416));
#31644=CARTESIAN_POINT('Ctrl Pts',(-0.000987755940621543,-0.0379994923712694,
-0.0151601899708721));
#31645=CARTESIAN_POINT('Ctrl Pts',(-0.00303614100278615,-0.0378420882025634,
-0.012990576891659));
#31646=CARTESIAN_POINT('Ctrl Pts',(-0.00234912094196705,-0.0376846840338575,
-0.0100869401879562));
#31647=CARTESIAN_POINT('Ctrl Pts',(0.00045433511394796,-0.0375272798651515,
-0.00906530564202212));
#31648=CARTESIAN_POINT('Ctrl Pts',(0.00284845879549029,-0.0373698756964455,
-0.0108461129052353));
#31649=CARTESIAN_POINT('Ctrl Pts',(0.00267626912834154,-0.0372124715277395,
-0.0138249471582369));
#31650=CARTESIAN_POINT('Ctrl Pts',(9.29000218480465E-5,-0.0370550673590335,
-0.0153180335192447));
#31651=CARTESIAN_POINT('Ctrl Pts',(-0.00257416717140274,-0.0368976631903275,
-0.0139801787553691));
#31652=CARTESIAN_POINT('Ctrl Pts',(-0.00292204349792889,-0.0367402590216216,
-0.0110167204956124));
#31653=CARTESIAN_POINT('Ctrl Pts',(-0.000637310458302599,-0.0365828548529156,
-0.00909758065277731));
#31654=CARTESIAN_POINT('Ctrl Pts',(0.00222160618930928,-0.0364254506842097,
-0.00995180450844874));
#31655=CARTESIAN_POINT('Ctrl Pts',(0.00307897109364783,-0.0362680465155037,
-0.0128097807533718));
#31656=CARTESIAN_POINT('Ctrl Pts',(0.00116234302327428,-0.0361106423467977,
-0.0150966212890749));
#31657=CARTESIAN_POINT('Ctrl Pts',(-0.00180149571654633,-0.0359532381780916,
-0.0147520016152729));
#31658=CARTESIAN_POINT('Ctrl Pts',(-0.00314228042009149,-0.0357958340093857,
-0.0120864061519114));
#31659=CARTESIAN_POINT('Ctrl Pts',(-0.00165203373548518,-0.0356384298406797,
-0.00950139790926134));
#31660=CARTESIAN_POINT('Ctrl Pts',(0.00132660950642858,-0.0354810256719738,
-0.00932593499899645));
#31661=CARTESIAN_POINT('Ctrl Pts',(0.0031100465126227,-0.0353236215032677,
-0.0117181003863419));
#31662=CARTESIAN_POINT('Ctrl Pts',(0.00209149320647923,-0.0351662173345617,
-0.0145226773523198));
#31663=CARTESIAN_POINT('Ctrl Pts',(-0.000811386806402,-0.0350088131658558,
-0.0152128877741252));
#31664=CARTESIAN_POINT('Ctrl Pts',(-0.00298324946569276,-0.0348514089971498,
-0.0131668879245621));
#31665=CARTESIAN_POINT('Ctrl Pts',(-0.00246735936371563,-0.0346940048284438,
-0.0102280173594368));
#31666=CARTESIAN_POINT('Ctrl Pts',(0.000271493323074386,-0.0345366006597379,
-0.00904404575682176));
#31667=CARTESIAN_POINT('Ctrl Pts',(0.00276574463210646,-0.0343791964910318,
-0.0106816700119495));
#31668=CARTESIAN_POINT('Ctrl Pts',(0.00276820373396548,-0.0342217923223258,
-0.0136654757615811));
#31669=CARTESIAN_POINT('Ctrl Pts',(0.00027665510425068,-0.0340643881536199,
-0.0153072090595452));
#31670=CARTESIAN_POINT('Ctrl Pts',(-0.00246414539781781,-0.0339069839849139,
-0.0141277535112517));
#31671=CARTESIAN_POINT('Ctrl Pts',(-0.00298487893497639,-0.0337495798162079,
-0.0111897372748958));
#31672=CARTESIAN_POINT('Ctrl Pts',(-0.000816391636836017,-0.033592175647502,
-0.00914016033656626));
#31673=CARTESIAN_POINT('Ctrl Pts',(0.00208762209378833,-0.0334347714787959,
-0.00982558499586843));
#31674=CARTESIAN_POINT('Ctrl Pts',(0.00311079681486421,-0.0332773673100899,
-0.012628479302303));
#31675=CARTESIAN_POINT('Ctrl Pts',(0.00133130519009939,-0.033119963141384,
-0.0150235810179823));
#31676=CARTESIAN_POINT('Ctrl Pts',(-0.00164762313977976,-0.032962558972678,
-0.0148530281468983));
#31677=CARTESIAN_POINT('Ctrl Pts',(-0.00314212881983791,-0.0328051548039721,
-0.0122704795705587));
#31678=CARTESIAN_POINT('Ctrl Pts',(-0.00180573932612758,-0.0326477506352661,
-0.0096026781348768));
#31679=CARTESIAN_POINT('Ctrl Pts',(0.00115752675646824,-0.03249034646656,
-0.00925317282644791));
#31680=CARTESIAN_POINT('Ctrl Pts',(0.00307792277508429,-0.032332942297854,
-0.0115368526677282));
#31681=CARTESIAN_POINT('Ctrl Pts',(0.00222526757665021,-0.0321755381291481,
-0.0143962351377196));
#31682=CARTESIAN_POINT('Ctrl Pts',(-0.000632232786428663,-0.0320181339604421,
-0.0152551761811062));
#31683=CARTESIAN_POINT('Ctrl Pts',(-0.00292013456997303,-0.0318607297917362,
-0.0133397931842086));
#31684=CARTESIAN_POINT('Ctrl Pts',(-0.00257712677055912,-0.0317033256230302,
-0.0103757882758759));
#31685=CARTESIAN_POINT('Ctrl Pts',(8.76993032760954E-5,-0.0315459214543242,
-0.00903349498082356));
#31686=CARTESIAN_POINT('Ctrl Pts',(0.00267358882914799,-0.0313885172856182,
-0.0105224072151816));
#31687=CARTESIAN_POINT('Ctrl Pts',(0.00285056591303206,-0.0312311131169122,
-0.0135007861344581));
#31688=CARTESIAN_POINT('Ctrl Pts',(0.000459618889897568,-0.0310737089482062,
-0.0152858630904674));
#31689=CARTESIAN_POINT('Ctrl Pts',(-0.00234598085158822,-0.0309163047795002,
-0.0142682165804294));
#31690=CARTESIAN_POINT('Ctrl Pts',(-0.00303688185573135,-0.0307589006107943,
-0.0113669520628329));
#31691=CARTESIAN_POINT('Ctrl Pts',(-0.000993857761956247,-0.0306014964420883,
-0.00919154437726977));
#31692=CARTESIAN_POINT('Ctrl Pts',(0.00194942720100573,-0.0304440691923362,
-0.00971077604905543));
#31693=CARTESIAN_POINT('Ctrl Pts',(0.00273326264745976,-0.0303391099988195,
-0.0115294799032454));
#31694=CARTESIAN_POINT('Ctrl Pts',(0.00265735689051292,-0.0302866188615381,
-0.0124059107630547));
#31695=CARTESIAN_POINT('Ctrl Pts',(-0.00200715618556375,-0.0407739344235557,
-0.0101695123425088));
#31696=CARTESIAN_POINT('Ctrl Pts',(-0.00134560506107313,-0.0407214555912242,
-0.00950767155873293));
#31697=CARTESIAN_POINT('Ctrl Pts',(0.000671733669518215,-0.0406165087026574,
-0.00890029303533848));
#31698=CARTESIAN_POINT('Ctrl Pts',(0.0031104577709741,-0.0404590937578553,
-0.0109407072489448));
#31699=CARTESIAN_POINT('Ctrl Pts',(0.00273886207562857,-0.0403016895891492,
-0.0140942010406314));
#31700=CARTESIAN_POINT('Ctrl Pts',(-9.64566422462461E-5,-0.0401442854204432,
-0.0155191106663781));
#31701=CARTESIAN_POINT('Ctrl Pts',(-0.00284683608352339,-0.0399868812517372,
-0.013932052606536));
#31702=CARTESIAN_POINT('Ctrl Pts',(-0.00303135672222567,-0.0398294770830313,
-0.0107626812392848));
#31703=CARTESIAN_POINT('Ctrl Pts',(-0.000485300036822523,-0.0396720729143253,
-0.00886653993958215));
#31704=CARTESIAN_POINT('Ctrl Pts',(0.00249825273968653,-0.0395146687456193,
-0.00995189977910353));
#31705=CARTESIAN_POINT('Ctrl Pts',(0.00323087291957833,-0.0393572645769133,
-0.0130409355465842));
#31706=CARTESIAN_POINT('Ctrl Pts',(0.00105271471644265,-0.0391998604082073,
-0.0153505723300579));
#31707=CARTESIAN_POINT('Ctrl Pts',(-0.00207392084708856,-0.0390424562395013,
-0.0147999546865617));
#31708=CARTESIAN_POINT('Ctrl Pts',(-0.00333204293495346,-0.0388850520707954,
-0.0118851567557591));
#31709=CARTESIAN_POINT('Ctrl Pts',(-0.00158817700263329,-0.0387276479020894,
-0.00923226194860017));
#31710=CARTESIAN_POINT('Ctrl Pts',(0.00158655878823555,-0.0385702437333834,
-0.00923138965431788));
#31711=CARTESIAN_POINT('Ctrl Pts',(0.00333188502928228,-0.0384128395646775,
-0.0118833262733665));
#31712=CARTESIAN_POINT('Ctrl Pts',(0.00207535727502861,-0.0382554353959714,
-0.0147988144430997));
#31713=CARTESIAN_POINT('Ctrl Pts',(-0.00105096021512142,-0.0380980312272654,
-0.0153511509433537));
#31714=CARTESIAN_POINT('Ctrl Pts',(-0.00323041681674889,-0.0379406270585595,
-0.0130427092173285));
#31715=CARTESIAN_POINT('Ctrl Pts',(-0.00249943589199024,-0.0377832228898535,
-0.00995327535086339));
#31716=CARTESIAN_POINT('Ctrl Pts',(0.000483406993018524,-0.0376258187211476,
-0.0088662687148974));
#31717=CARTESIAN_POINT('Ctrl Pts',(0.00303072524837413,-0.0374684145524415,
-0.0107610258178098));
#31718=CARTESIAN_POINT('Ctrl Pts',(0.00284751755284311,-0.0373110103837356,
-0.0139304689551257));
#31719=CARTESIAN_POINT('Ctrl Pts',(9.88444846859617E-5,-0.0371536062150296,
-0.0155190945443297));
#31720=CARTESIAN_POINT('Ctrl Pts',(-0.00273888232199736,-0.0369962020463236,
-0.014095633471993));
#31721=CARTESIAN_POINT('Ctrl Pts',(-0.00310901846993227,-0.0368387978776176,
-0.0109425502030451));
#31722=CARTESIAN_POINT('Ctrl Pts',(-0.000678090516909955,-0.0366813937089118,
-0.00890060893078614));
#31723=CARTESIAN_POINT('Ctrl Pts',(0.00236376175795272,-0.0365239895402056,
-0.00980949264405794));
#31724=CARTESIAN_POINT('Ctrl Pts',(0.00327598750851028,-0.0363665853714997,
-0.0128503443419849));
#31725=CARTESIAN_POINT('Ctrl Pts',(0.00123671873136661,-0.0362091812027937,
-0.0152835146450041));
#31726=CARTESIAN_POINT('Ctrl Pts',(-0.00191676936370603,-0.0360517770340877,
-0.0149168435356549));
#31727=CARTESIAN_POINT('Ctrl Pts',(-0.00334334785594242,-0.0358943728653817,
-0.0120806826315366));
#31728=CARTESIAN_POINT('Ctrl Pts',(-0.0017577436476271,-0.0357369686966757,
-0.00933026554259774));
#31729=CARTESIAN_POINT('Ctrl Pts',(0.00141149625623215,-0.0355795645279697,
-0.00914357515650723));
#31730=CARTESIAN_POINT('Ctrl Pts',(0.00330905137344668,-0.0354221603592638,
-0.0116888098108379));
#31731=CARTESIAN_POINT('Ctrl Pts',(0.00222532313885494,-0.0352647561905578,
-0.0146728453304159));
#31732=CARTESIAN_POINT('Ctrl Pts',(-0.000863305617849753,-0.0351073520218518,
-0.0154072207601635));
#31733=CARTESIAN_POINT('Ctrl Pts',(-0.00317414086950739,-0.0349499478531458,
-0.0132303019955118));
#31734=CARTESIAN_POINT('Ctrl Pts',(-0.00262524012362902,-0.0347925436844399,
-0.0101033797323109));
#31735=CARTESIAN_POINT('Ctrl Pts',(0.000288865568394113,-0.0346351395157338,
-0.00884364845760027));
#31736=CARTESIAN_POINT('Ctrl Pts',(0.00294271839225862,-0.0344777353470279,
-0.0105860605947262));
#31737=CARTESIAN_POINT('Ctrl Pts',(0.00294533484649854,-0.0343203311783219,
-0.013760793343527));
#31738=CARTESIAN_POINT('Ctrl Pts',(0.00029435764030422,-0.0341629270096159,
-0.0155075774518714));
#31739=CARTESIAN_POINT('Ctrl Pts',(-0.00262182050330342,-0.03400552284091,
-0.0142526512036113));
#31740=CARTESIAN_POINT('Ctrl Pts',(-0.0031758746048549,-0.0338481186722039,
-0.0111266379357506));
#31741=CARTESIAN_POINT('Ctrl Pts',(-0.000868630696093512,-0.033690714503498,
-0.00894591319249119));
#31742=CARTESIAN_POINT('Ctrl Pts',(0.00222120432239532,-0.033533310334792,
-0.00967519662958854));
#31743=CARTESIAN_POINT('Ctrl Pts',(0.00330984968583626,-0.033375906166086,
-0.0126574418200349));
#31744=CARTESIAN_POINT('Ctrl Pts',(0.00141649240610871,-0.0332185019973801,
-0.0152058006917256));
#31745=CARTESIAN_POINT('Ctrl Pts',(-0.00175305082785179,-0.0330610978286742,
-0.0150243345271474));
#31746=CARTESIAN_POINT('Ctrl Pts',(-0.00334318655513065,-0.032903693659968,
-0.0122765344930177));
#31747=CARTESIAN_POINT('Ctrl Pts',(-0.00192128451229188,-0.0327462894912621,
-0.00943802646138645));
#31748=CARTESIAN_POINT('Ctrl Pts',(0.00123159428251195,-0.0325888853225561,
-0.00906615709667131));
#31749=CARTESIAN_POINT('Ctrl Pts',(0.00327487211040667,-0.0324314811538501,
-0.0114959644595614));
#31750=CARTESIAN_POINT('Ctrl Pts',(0.00236765742921036,-0.0322740769851443,
-0.0145383123637269));
#31751=CARTESIAN_POINT('Ctrl Pts',(-0.000672687936266725,-0.0321166728164382,
-0.0154522151069147));
#31752=CARTESIAN_POINT('Ctrl Pts',(-0.00310698739398267,-0.0319592686477321,
-0.0134142710726901));
#31753=CARTESIAN_POINT('Ctrl Pts',(-0.00274203129922751,-0.0318018644790262,
-0.010260606176357));
#31754=CARTESIAN_POINT('Ctrl Pts',(9.33109838642071E-5,-0.0316444603103202,
-0.00883242256124597));
#31755=CARTESIAN_POINT('Ctrl Pts',(0.00284466574735029,-0.0314870561416142,
-0.0104166069308519));
#31756=CARTESIAN_POINT('Ctrl Pts',(0.00303296719561427,-0.0313296519729082,
-0.0135855655986646));
#31757=CARTESIAN_POINT('Ctrl Pts',(0.000489028865872123,-0.0311722478042024,
-0.0154848656023836));
#31758=CARTESIAN_POINT('Ctrl Pts',(-0.0024960948743115,-0.0310148436354963,
-0.0144021021877348));
#31759=CARTESIAN_POINT('Ctrl Pts',(-0.00323120507520287,-0.0308574394667903,
-0.0113151922982138));
#31760=CARTESIAN_POINT('Ctrl Pts',(-0.00105745247823908,-0.0307000352980843,
-0.00900058518204926));
#31761=CARTESIAN_POINT('Ctrl Pts',(0.00207416665015809,-0.0305426080483322,
-0.00955304131725042));
#31762=CARTESIAN_POINT('Ctrl Pts',(0.00290815795868601,-0.0304376488548157,
-0.0114881199285106));
#31763=CARTESIAN_POINT('Ctrl Pts',(0.0028273951635772,-0.0303851577175343,
-0.0124206316220213));
#31764=CARTESIAN_POINT('Ctrl Pts',(-0.00212786565552399,-0.0408724732795518,
-0.0100488519008064));
#31765=CARTESIAN_POINT('Ctrl Pts',(-0.00142652914404491,-0.0408199944472204,
-0.00934720831006298));
#31766=CARTESIAN_POINT('Ctrl Pts',(0.000712131430183422,-0.0407150475586535,
-0.00870330231553719));
#31767=CARTESIAN_POINT('Ctrl Pts',(0.00329751930189471,-0.0405576326138514,
-0.0108664261219471));
#31768=CARTESIAN_POINT('Ctrl Pts',(0.0029035760086157,-0.0404002284451454,
-0.0142095696114775));
#31769=CARTESIAN_POINT('Ctrl Pts',(-0.000102257501314122,-0.0402428242764393,
-0.0157201726610358));
#31770=CARTESIAN_POINT('Ctrl Pts',(-0.00301804352476665,-0.0400854201077334,
-0.0140376696435079));
#31771=CARTESIAN_POINT('Ctrl Pts',(-0.00321366115166276,-0.0399280159390274,
-0.010677693708162));
#31772=CARTESIAN_POINT('Ctrl Pts',(-0.000514485762695765,-0.0397706117703215,
-0.00866751932378795));
#31773=CARTESIAN_POINT('Ctrl Pts',(0.00264849653546252,-0.0396132076016156,
-0.00981815221574397));
#31774=CARTESIAN_POINT('Ctrl Pts',(0.00342517616335999,-0.0394558034329095,
-0.0130929612044931));
#31775=CARTESIAN_POINT('Ctrl Pts',(0.00111602450586276,-0.0392983992642035,
-0.0155414985049964));
#31776=CARTESIAN_POINT('Ctrl Pts',(-0.00219864551375484,-0.0391409950954976,
-0.0149577669641485));
#31777=CARTESIAN_POINT('Ctrl Pts',(-0.00353243049794239,-0.0389835909267915,
-0.0118676743971841));
#31778=CARTESIAN_POINT('Ctrl Pts',(-0.00168368925303498,-0.0388261867580856,
-0.00905523568988633));
#31779=CARTESIAN_POINT('Ctrl Pts',(0.00168197371995147,-0.0386687825893795,
-0.00905431093621841));
#31780=CARTESIAN_POINT('Ctrl Pts',(0.00353226309589514,-0.0385113784206737,
-0.011865733830404));
#31781=CARTESIAN_POINT('Ctrl Pts',(0.00220016832782498,-0.0383539742519676,
-0.0149565581469579));
#31782=CARTESIAN_POINT('Ctrl Pts',(-0.00111416448962141,-0.0381965700832616,
-0.0155421119158356));
#31783=CARTESIAN_POINT('Ctrl Pts',(-0.00342469263071152,-0.0380391659145558,
-0.013094841542998));
#31784=CARTESIAN_POINT('Ctrl Pts',(-0.00264975084201354,-0.0378817617458498,
-0.00981961051377058));
#31785=CARTESIAN_POINT('Ctrl Pts',(0.000512478872088983,-0.0377243575771436,
-0.00866723178777268));
#31786=CARTESIAN_POINT('Ctrl Pts',(0.00321299170125789,-0.0375669534084378,
-0.0106759387303842));
#31787=CARTESIAN_POINT('Ctrl Pts',(0.0030187659773448,-0.0374095492397318,
-0.0140359907520142));
#31788=CARTESIAN_POINT('Ctrl Pts',(0.000104788947523881,-0.0372521450710258,
-0.0157201555694146));
#31789=CARTESIAN_POINT('Ctrl Pts',(-0.00290359747259187,-0.0370947409023197,
-0.0142110881886168));
#31790=CARTESIAN_POINT('Ctrl Pts',(-0.00329599344193575,-0.0369373367336139,
-0.0108683799104779));
#31791=CARTESIAN_POINT('Ctrl Pts',(-0.000718870575517203,-0.0367799325649078,
-0.00870363720879496));
#31792=CARTESIAN_POINT('Ctrl Pts',(0.00250591732659617,-0.0366225283962018,
-0.00966718077966711));
#31793=CARTESIAN_POINT('Ctrl Pts',(0.00347300392337274,-0.0364651242274959,
-0.012890907930598));
#31794=CARTESIAN_POINT('Ctrl Pts',(0.00131109443945905,-0.0363077200587899,
-0.0154704080009334));
#31795=CARTESIAN_POINT('Ctrl Pts',(-0.00203204301086584,-0.0361503158900839,
-0.0150816854560369));
#31796=CARTESIAN_POINT('Ctrl Pts',(-0.00354441529179335,-0.0359929117213779,
-0.0120749591111619));
#31797=CARTESIAN_POINT('Ctrl Pts',(-0.00186345355976913,-0.035835507552672,
-0.00915913317593414));
#31798=CARTESIAN_POINT('Ctrl Pts',(0.00149638300603574,-0.0356781033839659,
-0.00896121531401801));
#31799=CARTESIAN_POINT('Ctrl Pts',(0.00350805623427067,-0.0355206992152599,
-0.0116595192353337));
#31800=CARTESIAN_POINT('Ctrl Pts',(0.00235915307123073,-0.0353632950465541,
-0.0148230133085119));
#31801=CARTESIAN_POINT('Ctrl Pts',(-0.000915224429297398,-0.0352058908778481,
-0.0156015537462018));
#31802=CARTESIAN_POINT('Ctrl Pts',(-0.00336503227332211,-0.035048486709142,
-0.0132937160664613));
#31803=CARTESIAN_POINT('Ctrl Pts',(-0.00278312088354253,-0.0348910825404361,
-0.00997874210518484));
#31804=CARTESIAN_POINT('Ctrl Pts',(0.000306237813713841,-0.0347336783717301,
-0.00864325115837878));
#31805=CARTESIAN_POINT('Ctrl Pts',(0.0031196921524109,-0.034576274203024,
-0.0104904511775031));
#31806=CARTESIAN_POINT('Ctrl Pts',(0.0031224659590316,-0.0344188700343182,
-0.0138561109254727));
#31807=CARTESIAN_POINT('Ctrl Pts',(0.000312060176357651,-0.0342614658656122,
-0.0157079458441975));
#31808=CARTESIAN_POINT('Ctrl Pts',(-0.00277949560878902,-0.0341040616969062,
-0.0143775488959709));
#31809=CARTESIAN_POINT('Ctrl Pts',(-0.00336687027473339,-0.0339466575282002,
-0.0110635385966054));
#31810=CARTESIAN_POINT('Ctrl Pts',(-0.000920869755351007,-0.0337892533594942,
-0.00875166604841612));
#31811=CARTESIAN_POINT('Ctrl Pts',(0.00235478655100232,-0.0336318491907882,
-0.00952480826330864));
#31812=CARTESIAN_POINT('Ctrl Pts',(0.0035089025568082,-0.0334744450220822,
-0.0126864043377667));
#31813=CARTESIAN_POINT('Ctrl Pts',(0.00150167962211813,-0.0333170408533761,
-0.015388020365469));
#31814=CARTESIAN_POINT('Ctrl Pts',(-0.00185847851592382,-0.0331596366846703,
-0.0151956409073963));
#31815=CARTESIAN_POINT('Ctrl Pts',(-0.00354424429042339,-0.0330022325159643,
-0.0122825894154766));
#31816=CARTESIAN_POINT('Ctrl Pts',(-0.00203682969845604,-0.0328448283472583,
-0.00927337478789609));
#31817=CARTESIAN_POINT('Ctrl Pts',(0.00130566180855576,-0.0326874241785523,
-0.00887914136689471));
#31818=CARTESIAN_POINT('Ctrl Pts',(0.00347182144572907,-0.0325300200098464,
-0.0114550762513946));
#31819=CARTESIAN_POINT('Ctrl Pts',(0.0025100472817705,-0.0323726158411403,
-0.0146803895897339));
#31820=CARTESIAN_POINT('Ctrl Pts',(-0.000713143086104787,-0.0322152116724343,
-0.0156492540327232));
#31821=CARTESIAN_POINT('Ctrl Pts',(-0.00329384021799231,-0.0320578075037284,
-0.0134887489611716));
#31822=CARTESIAN_POINT('Ctrl Pts',(-0.00290693582789601,-0.0319004033350224,
-0.0101454240768384));
#31823=CARTESIAN_POINT('Ctrl Pts',(9.89226644522099E-5,-0.0317429991663165,
-0.0086313501416684));
#31824=CARTESIAN_POINT('Ctrl Pts',(0.00301574266555261,-0.0315855949976104,
-0.0103108066465221));
#31825=CARTESIAN_POINT('Ctrl Pts',(0.00321536847819648,-0.0314281908289045,
-0.0136703450628712));
#31826=CARTESIAN_POINT('Ctrl Pts',(0.000518438841846787,-0.0312707866601984,
-0.0156838681142999));
#31827=CARTESIAN_POINT('Ctrl Pts',(-0.00264620889703467,-0.0311133824914924,
-0.0145359877950401));
#31828=CARTESIAN_POINT('Ctrl Pts',(-0.0034255282946743,-0.0309559783227865,
-0.0112634325335946));
#31829=CARTESIAN_POINT('Ctrl Pts',(-0.00112104719452203,-0.0307985741540806,
-0.00880962598682875));
#31830=CARTESIAN_POINT('Ctrl Pts',(0.00219890609931043,-0.0306411469043285,
-0.00939530658544539));
#31831=CARTESIAN_POINT('Ctrl Pts',(0.00308305326991214,-0.0305361877108118,
-0.0114467599537756));
#31832=CARTESIAN_POINT('Ctrl Pts',(0.00299743343664159,-0.0304836965735304,
-0.0124353524809878));
#31833=CARTESIAN_POINT('',(0.00298893256437761,-0.0304787743898623,-0.0124333064388995));
#31834=CARTESIAN_POINT('Ctrl Pts',(0.00298893256437029,-0.0304787743898723,
-0.012433306438892));
#31835=CARTESIAN_POINT('Ctrl Pts',(0.00298837300754948,-0.030478774389874,
-0.0123352674302941));
#31836=CARTESIAN_POINT('Ctrl Pts',(0.00298261840524365,-0.0304787743898738,
-0.0122375191512274));
#31837=CARTESIAN_POINT('Ctrl Pts',(0.00297189591856322,-0.0304787743898736,
-0.0121403782556776));
#31838=CARTESIAN_POINT('Ctrl Pts',(0.0029506659422511,-0.0304787743898733,
-0.0119480442409175));
#31839=CARTESIAN_POINT('Ctrl Pts',(0.0029099981664046,-0.0304787743898729,
-0.0117580651785402));
#31840=CARTESIAN_POINT('Ctrl Pts',(0.00285112369699802,-0.0304787743898726,
-0.0115730963590973));
#31841=CARTESIAN_POINT('Ctrl Pts',(0.00284398971481766,-0.0304787743898726,
-0.0115506831760126));
#31842=CARTESIAN_POINT('Ctrl Pts',(0.00283658767728467,-0.0304787743898725,
-0.0115283440580714));
#31843=CARTESIAN_POINT('Ctrl Pts',(0.00282891920321681,-0.0304787743898725,
-0.0115060841919811));
#31844=CARTESIAN_POINT('Ctrl Pts',(0.00282186171808973,-0.0304787743898724,
-0.011485597890212));
#31845=CARTESIAN_POINT('Ctrl Pts',(0.00281457673346536,-0.0304787743898724,
-0.011465174083367));
#31846=CARTESIAN_POINT('Ctrl Pts',(0.00280707621326217,-0.0304787743898724,
-0.0114448451703835));
#31847=CARTESIAN_POINT('Ctrl Pts',(0.00270641710168845,-0.0304787743898717,
-0.0111720253839232));
#31848=CARTESIAN_POINT('Ctrl Pts',(0.00256690712160261,-0.0304787743898713,
-0.0109151889309775));
#31849=CARTESIAN_POINT('Ctrl Pts',(0.0023924314614952,-0.0304787743898706,
-0.0106839334442482));
#31850=CARTESIAN_POINT('Ctrl Pts',(0.00238354432219219,-0.0304787743898706,
-0.0106721541523751));
#31851=CARTESIAN_POINT('Ctrl Pts',(0.00237456589083953,-0.0304787743898706,
-0.0106604419288824));
#31852=CARTESIAN_POINT('Ctrl Pts',(0.00236549651133127,-0.0304787743898705,
-0.0106487982886585));
#31853=CARTESIAN_POINT('Ctrl Pts',(0.00235654131236866,-0.0304787743898705,
-0.0106373012380874));
#31854=CARTESIAN_POINT('Ctrl Pts',(0.00234750304637241,-0.0304787743898705,
-0.0106258782674));
#31855=CARTESIAN_POINT('Ctrl Pts',(0.00233838354414271,-0.0304787743898705,
-0.0106145320289449));
#31856=CARTESIAN_POINT('Ctrl Pts',(0.0021652597390184,-0.0304787743898699,
-0.0103991360648103));
#31857=CARTESIAN_POINT('Ctrl Pts',(0.00196289502114972,-0.0304787743898692,
-0.0102109270530416));
#31858=CARTESIAN_POINT('Ctrl Pts',(0.00173430499794,-0.0304787743898686,
-0.0100590786561608));
#31859=CARTESIAN_POINT('Ctrl Pts',(0.00172022400467282,-0.0304787743898685,
-0.0100497248959919));
#31860=CARTESIAN_POINT('Ctrl Pts',(0.00170604292827687,-0.0304787743898685,
-0.0100405103160519));
#31861=CARTESIAN_POINT('Ctrl Pts',(0.00169176227320023,-0.0304787743898685,
-0.0100314375701239));
#31862=CARTESIAN_POINT('Ctrl Pts',(0.00166701763122726,-0.0304787743898684,
-0.0100157168732445));
#31863=CARTESIAN_POINT('Ctrl Pts',(0.00164197401157139,-0.0304787743898683,
-0.0100004219931363));
#31864=CARTESIAN_POINT('Ctrl Pts',(0.00161664364654793,-0.0304787743898682,
-0.00998555579774938));
#31865=CARTESIAN_POINT('Ctrl Pts',(0.00160269290467747,-0.0304787743898682,
-0.00997736821520777));
#31866=CARTESIAN_POINT('Ctrl Pts',(0.00158865518509774,-0.0304787743898682,
-0.00996931067307717));
#31867=CARTESIAN_POINT('Ctrl Pts',(0.00157453253482917,-0.0304787743898681,
-0.00996138371355764));
#31868=CARTESIAN_POINT('Ctrl Pts',(0.0015624910192888,-0.0304787743898681,
-0.00995462488257144));
#31869=CARTESIAN_POINT('Ctrl Pts',(0.00155038831353741,-0.0304787743898681,
-0.00994796137764227));
#31870=CARTESIAN_POINT('Ctrl Pts',(0.00153823739716388,-0.030478774389868,
-0.00994139960184977));
#31871=CARTESIAN_POINT('Ctrl Pts',(0.00125129790158513,-0.0304787743898672,
-0.00978644563968585));
#31872=CARTESIAN_POINT('Ctrl Pts',(0.000935868208510309,-0.0304787743898666,
-0.00968658593292551));
#31873=CARTESIAN_POINT('Ctrl Pts',(0.000609871031302533,-0.030478774389866,
-0.00964440028463229));
#31874=CARTESIAN_POINT('Ctrl Pts',(0.000593206497894966,-0.030478774389866,
-0.00964224381152622));
#31875=CARTESIAN_POINT('Ctrl Pts',(0.000576512109012424,-0.030478774389866,
-0.00964023965127942));
#31876=CARTESIAN_POINT('Ctrl Pts',(0.000559813525617774,-0.030478774389866,
-0.0096383909861675));
#31877=CARTESIAN_POINT('Ctrl Pts',(0.000296852526983212,-0.0304787743898655,
-0.00960927912604843));
#31878=CARTESIAN_POINT('Ctrl Pts',(3.15475597085231E-5,-0.0304787743898651,
-0.00961823760304827));
#31879=CARTESIAN_POINT('Ctrl Pts',(-0.000226290956562403,-0.0304787743898647,
-0.00966738870262534));
#31880=CARTESIAN_POINT('Ctrl Pts',(-0.000282359974600194,-0.0304787743898646,
-0.00967807699671196));
#31881=CARTESIAN_POINT('Ctrl Pts',(-0.00033806990970888,-0.0304787743898646,
-0.00969068022176533));
#31882=CARTESIAN_POINT('Ctrl Pts',(-0.000393306057963943,-0.0304787743898718,
-0.00970524382248907));
#31883=CARTESIAN_POINT('',(-0.00299999910843776,-0.0309924495244571,-0.0121735404154808));
#31884=CARTESIAN_POINT('Ctrl Pts',(-0.00299999910843776,-0.0309924495244571,
-0.0121735404154808));
#31885=CARTESIAN_POINT('Ctrl Pts',(-0.00299957015955796,-0.0309629253341015,
-0.0116171556391684));
#31886=CARTESIAN_POINT('Ctrl Pts',(-0.00284005225347564,-0.0309334011437459,
-0.0110606943513532));
#31887=CARTESIAN_POINT('Ctrl Pts',(-0.00254572450208166,-0.0309038769533902,
-0.0105886271654584));
#31888=CARTESIAN_POINT('Ctrl Pts',(-0.00241331504383175,-0.0308905948825296,
-0.0103762579272678));
#31889=CARTESIAN_POINT('Ctrl Pts',(-0.002254325614464,-0.030877312811669,
-0.0101807858430437));
#31890=CARTESIAN_POINT('Ctrl Pts',(-0.00207401368765223,-0.0308640307408084,
-0.0100082584850716));
#31891=CARTESIAN_POINT('Ctrl Pts',(-0.00168100707884367,-0.0308350812324804,
-0.00963221906781163));
#31892=CARTESIAN_POINT('Ctrl Pts',(-0.00118098993580744,-0.0308061317241523,
-0.00936454502561941));
#31893=CARTESIAN_POINT('Ctrl Pts',(-0.000647803879971564,-0.0307771822158243,
-0.00924662981725879));
#31894=CARTESIAN_POINT('Ctrl Pts',(-0.000392593071710581,-0.0307633254629361,
-0.00919018941469651));
#31895=CARTESIAN_POINT('Ctrl Pts',(-0.000130218005705817,-0.0307494687100479,
-0.00916738448966662));
#31896=CARTESIAN_POINT('Ctrl Pts',(0.000130000822421629,-0.0307356119571597,
-0.00917867131240808));
#31897=CARTESIAN_POINT('Ctrl Pts',(0.000673649626204348,-0.0307066624488317,
-0.00920225172634686));
#31898=CARTESIAN_POINT('Ctrl Pts',(0.00121291501584666,-0.0306777129405036,
-0.00937818640396837));
#31899=CARTESIAN_POINT('Ctrl Pts',(0.00166686823158946,-0.0306487634321756,
-0.00968154971671783));
#31900=CARTESIAN_POINT('Ctrl Pts',(0.00188415404736492,-0.0306349066792874,
-0.00982675530751699));
#31901=CARTESIAN_POINT('Ctrl Pts',(0.002082085130544,-0.0306210499263992,
-0.0100003750833504));
#31902=CARTESIAN_POINT('Ctrl Pts',(0.00225390745583324,-0.030607193173511,
-0.0101959792550754));
#31903=CARTESIAN_POINT('Ctrl Pts',(0.00262000441087861,-0.0305776689831554,
-0.0106127475157898));
#31904=CARTESIAN_POINT('Ctrl Pts',(0.00286825892999133,-0.0305481447927997,
-0.0111350521502138));
#31905=CARTESIAN_POINT('Ctrl Pts',(0.00295948265647319,-0.0305186206024441,
-0.0116844650428705));
#31906=CARTESIAN_POINT('Ctrl Pts',(0.00300052154643768,-0.0305053385315835,
-0.0119316298553198));
#31907=CARTESIAN_POINT('Ctrl Pts',(0.00301041285349739,-0.030492056460723,
-0.0121839285032162));
#31908=CARTESIAN_POINT('Ctrl Pts',(0.00298893256436973,-0.0304787743898624,
-0.0124333064388988));
#31909=CARTESIAN_POINT('',(-0.00299999981352153,-0.0319945472736604,-0.0121769110534293));
#31910=CARTESIAN_POINT('Ctrl Pts',(-0.00299999981352153,-0.0319945472736604,
-0.0121769110534293));
#31911=CARTESIAN_POINT('Ctrl Pts',(-0.00300001642542353,-0.0319922152497922,
-0.0121297969829771));
#31912=CARTESIAN_POINT('Ctrl Pts',(-0.00299892317095584,-0.0319898566084726,
-0.0120826905849812));
#31913=CARTESIAN_POINT('Ctrl Pts',(-0.00299515512313883,-0.0319857664535245,
-0.0120021629381566));
#31914=CARTESIAN_POINT('Ctrl Pts',(-0.00299302858819974,-0.031984050903241,
-0.0119687245641428));
#31915=CARTESIAN_POINT('Ctrl Pts',(-0.00298877904546892,-0.0319813101095438,
-0.0119158915587133));
#31916=CARTESIAN_POINT('Ctrl Pts',(-0.00298702610746423,-0.0319802960930753,
-0.011896469513365));
#31917=CARTESIAN_POINT('Ctrl Pts',(-0.00298320600118927,-0.0319782901614954,
-0.0118583040786077));
#31918=CARTESIAN_POINT('Ctrl Pts',(-0.00298115121742591,-0.0319772986694851,
-0.0118395603452952));
#31919=CARTESIAN_POINT('Ctrl Pts',(-0.0029764027823879,-0.0319751770471325,
-0.0117997164611982));
#31920=CARTESIAN_POINT('Ctrl Pts',(-0.00297366114976589,-0.0319740454863181,
-0.0117786231650717));
#31921=CARTESIAN_POINT('Ctrl Pts',(-0.00296601432529667,-0.0319711098676958,
-0.0117243156949625));
#31922=CARTESIAN_POINT('Ctrl Pts',(-0.00296077554499708,-0.0319692956207431,
-0.0116911521179402));
#31923=CARTESIAN_POINT('Ctrl Pts',(-0.00293534004140591,-0.0319612568581492,
-0.0115459880653948));
#31924=CARTESIAN_POINT('Ctrl Pts',(-0.00290933809512656,-0.0319548560777858,
-0.0114351112327025));
#31925=CARTESIAN_POINT('Ctrl Pts',(-0.00283030627595261,-0.0319388149721708,
-0.0111675597328889));
#31926=CARTESIAN_POINT('Ctrl Pts',(-0.00277050385213032,-0.0319290335683348,
-0.0110132731158511));
#31927=CARTESIAN_POINT('Ctrl Pts',(-0.00266259098944409,-0.0319145847252816,
-0.0107911910668462));
#31928=CARTESIAN_POINT('Ctrl Pts',(-0.00262387856782943,-0.0319098400276056,
-0.0107191642974873));
#31929=CARTESIAN_POINT('Ctrl Pts',(-0.00256546348083541,-0.0319033297703317,
-0.0106203831154059));
#31930=CARTESIAN_POINT('Ctrl Pts',(-0.00254818702925803,-0.0319014746892419,
-0.0105922392738789));
#31931=CARTESIAN_POINT('Ctrl Pts',(-0.00251689521595761,-0.0318982430011514,
-0.0105431024978857));
#31932=CARTESIAN_POINT('Ctrl Pts',(-0.00250307315484794,-0.0318968568820697,
-0.0105219906775617));
#31933=CARTESIAN_POINT('Ctrl Pts',(-0.00248160693976785,-0.031894769038704,
-0.0104900888591791));
#31934=CARTESIAN_POINT('Ctrl Pts',(-0.00247415540277629,-0.0318940557475992,
-0.0104791712998327));
#31935=CARTESIAN_POINT('Ctrl Pts',(-0.00246030964179461,-0.0318927517986779,
-0.0104591704848017));
#31936=CARTESIAN_POINT('Ctrl Pts',(-0.0024539369867617,-0.0318921598417614,
-0.0104500732760709));
#31937=CARTESIAN_POINT('Ctrl Pts',(-0.00243920990448888,-0.0318908102733566,
-0.0104292963211079));
#31938=CARTESIAN_POINT('Ctrl Pts',(-0.00243082198851743,-0.0318900548883533,
-0.0104176409364644));
#31939=CARTESIAN_POINT('Ctrl Pts',(-0.00240349380418427,-0.0318876346538313,
-0.0103802366141087));
#31940=CARTESIAN_POINT('Ctrl Pts',(-0.00238422506486495,-0.0318859902850841,
-0.0103547292669735));
#31941=CARTESIAN_POINT('Ctrl Pts',(-0.00224440813997212,-0.031874453183327,
-0.0101756679812831));
#31942=CARTESIAN_POINT('Ctrl Pts',(-0.00210952066103542,-0.0318653282790874,
-0.0100338805378428));
#31943=CARTESIAN_POINT('Ctrl Pts',(-0.00182762110192053,-0.0318476390290283,
-0.00979021793073736));
#31944=CARTESIAN_POINT('Ctrl Pts',(-0.00168343109687408,-0.0318391306117249,
-0.00968637407129882));
#31945=CARTESIAN_POINT('Ctrl Pts',(-0.00149723877718005,-0.0318281472838993,
-0.00957588973391417));
#31946=CARTESIAN_POINT('Ctrl Pts',(-0.00146316413035672,-0.0318261387297483,
-0.009556562355812));
#31947=CARTESIAN_POINT('Ctrl Pts',(-0.00140897504517393,-0.031822942057075,
-0.00952721332681065));
#31948=CARTESIAN_POINT('Ctrl Pts',(-0.00138910921764175,-0.0318217696587595,
-0.00951674067893614));
#31949=CARTESIAN_POINT('Ctrl Pts',(-0.00135157780893566,-0.0318195529749003,
-0.00949749064022305));
#31950=CARTESIAN_POINT('Ctrl Pts',(-0.00133393953136627,-0.0318185105134473,
-0.00948866249676546));
#31951=CARTESIAN_POINT('Ctrl Pts',(-0.00129394467084666,-0.031816144615133,
-0.00946913545393362));
#31952=CARTESIAN_POINT('Ctrl Pts',(-0.00127154016664873,-0.0318148177994003,
-0.00945853847382943));
#31953=CARTESIAN_POINT('Ctrl Pts',(-0.00121314042737946,-0.0318113546597345,
-0.00943179671227953));
#31954=CARTESIAN_POINT('Ctrl Pts',(-0.00117695424730294,-0.0318092042269369,
-0.00941608252075385));
#31955=CARTESIAN_POINT('Ctrl Pts',(-0.0009009913001464,-0.0317927662081466,
-0.00930265768544881));
#31956=CARTESIAN_POINT('Ctrl Pts',(-0.000649805607183565,-0.0317774500921903,
-0.00923565791379496));
#31957=CARTESIAN_POINT('Ctrl Pts',(-0.000310970476071452,-0.0317574426099795,
-0.00919086122100353));
#31958=CARTESIAN_POINT('Ctrl Pts',(-0.000228318885291927,-0.0317526247646428,
-0.00918340410543012));
#31959=CARTESIAN_POINT('Ctrl Pts',(-9.66138540080629E-5,-0.0317451418381697,
-0.00917701060556102));
#31960=CARTESIAN_POINT('Ctrl Pts',(-4.77133307582583E-5,-0.031742406153735,
-0.00917583401678422));
#31961=CARTESIAN_POINT('Ctrl Pts',(1.8263743597101E-5,-0.031738791577688,
-0.009175860332671));
#31962=CARTESIAN_POINT('Ctrl Pts',(3.53309251822941E-5,-0.0317378634542682,
-0.00917601278406565));
#31963=CARTESIAN_POINT('Ctrl Pts',(6.38725522234893E-5,-0.0317363239422441,
-0.00917651135165962));
#31964=CARTESIAN_POINT('Ctrl Pts',(7.53478726622746E-5,-0.0317357083833803,
-0.00917677768611424));
#31965=CARTESIAN_POINT('Ctrl Pts',(9.88576639912124E-5,-0.0317344546351368,
-0.00917745835791557));
#31966=CARTESIAN_POINT('Ctrl Pts',(0.00011089162661713,-0.0317338167977515,
-0.00917787929685429));
#31967=CARTESIAN_POINT('Ctrl Pts',(0.000142654880958706,-0.0317321428488871,
-0.00917918186822764));
#31968=CARTESIAN_POINT('Ctrl Pts',(0.000162378861661807,-0.0317311131642323,
-0.00918018589020346));
#31969=CARTESIAN_POINT('Ctrl Pts',(0.000250653753600739,-0.0317265430617562,
-0.00918555383768674));
#31970=CARTESIAN_POINT('Ctrl Pts',(0.000319056744679814,-0.0317231049958787,
-0.00919207679906972));
#31971=CARTESIAN_POINT('Ctrl Pts',(0.000550364637773504,-0.0317116562800663,
-0.00922218113501574));
#31972=CARTESIAN_POINT('Ctrl Pts',(0.000711533127640449,-0.0317039669075692,
-0.00925681122974356));
#31973=CARTESIAN_POINT('Ctrl Pts',(0.000975195187799041,-0.0316908606773177,
-0.0093366117995718));
#31974=CARTESIAN_POINT('Ctrl Pts',(0.00107946837399842,-0.0316855340704567,
-0.00937459572977345));
#31975=CARTESIAN_POINT('Ctrl Pts',(0.00122609970636494,-0.0316776467731615,
-0.0094374148967181));
#31976=CARTESIAN_POINT('Ctrl Pts',(0.00127033040785503,-0.0316752139754418,
-0.00945765063389414));
#31977=CARTESIAN_POINT('Ctrl Pts',(0.00134939760217658,-0.0316707531341619,
-0.00949617563153442));
#31978=CARTESIAN_POINT('Ctrl Pts',(0.00138440366752245,-0.0316687372427017,
-0.00951409211620556));
#31979=CARTESIAN_POINT('Ctrl Pts',(0.00143884485791577,-0.031665532423469,
-0.0095433202040005));
#31980=CARTESIAN_POINT('Ctrl Pts',(0.00145852280510933,-0.0316643594058127,
-0.0095541713556147));
#31981=CARTESIAN_POINT('Ctrl Pts',(0.00149521458475665,-0.0316621437523772,
-0.00957494552087175));
#31982=CARTESIAN_POINT('Ctrl Pts',(0.00151225627130588,-0.0316611029706844,
-0.00958481704496393));
#31983=CARTESIAN_POINT('Ctrl Pts',(0.00155043989818843,-0.031658743935678,
-0.00960744022355745));
#31984=CARTESIAN_POINT('Ctrl Pts',(0.00157152392498763,-0.0316574223525361,
-0.00962028641323898));
#31985=CARTESIAN_POINT('Ctrl Pts',(0.00162564777565868,-0.031653979468501,
-0.00965418636345596));
#31986=CARTESIAN_POINT('Ctrl Pts',(0.00165843731727481,-0.0316518442906599,
-0.00967562925045361));
#31987=CARTESIAN_POINT('Ctrl Pts',(0.00190574893413454,-0.03163535362645,
-0.00984436573858123));
#31988=CARTESIAN_POINT('Ctrl Pts',(0.00210068014239803,-0.031619955545076,
-0.0100183516693828));
#31989=CARTESIAN_POINT('Ctrl Pts',(0.00234356759871333,-0.0315982011335395,
-0.0102996531862232));
#31990=CARTESIAN_POINT('Ctrl Pts',(0.00241169036278049,-0.0315917429710965,
-0.010388064348014));
#31991=CARTESIAN_POINT('Ctrl Pts',(0.00249048120709294,-0.0315839850065132,
-0.0105030474825988));
#31992=CARTESIAN_POINT('Ctrl Pts',(0.00250590632681066,-0.0315824508338868,
-0.0105262443964411));
#31993=CARTESIAN_POINT('Ctrl Pts',(0.00252845151920646,-0.0315801890589914,
-0.010561194949764));
#31994=CARTESIAN_POINT('Ctrl Pts',(0.00253581719650946,-0.031579446888502,
-0.0105727875393121));
#31995=CARTESIAN_POINT('Ctrl Pts',(0.00254897232253479,-0.0315781160616994,
-0.0105938095097945));
#31996=CARTESIAN_POINT('Ctrl Pts',(0.00255478946401977,-0.0315775256986796,
-0.0106032207120483));
#31997=CARTESIAN_POINT('Ctrl Pts',(0.00256782252689628,-0.0315761986505758,
-0.0106245692958359));
#31998=CARTESIAN_POINT('Ctrl Pts',(0.00257500739135149,-0.0315754639056578,
-0.0106365250243147));
#31999=CARTESIAN_POINT('Ctrl Pts',(0.00259684262389686,-0.0315732197606075,
-0.0106734399130476));
#32000=CARTESIAN_POINT('Ctrl Pts',(0.00261121580047175,-0.0315717266550666,
-0.0106985619415731));
#32001=CARTESIAN_POINT('Ctrl Pts',(0.00270767657634611,-0.0315615671502975,
-0.0108729678100802));
#32002=CARTESIAN_POINT('Ctrl Pts',(0.0027772896014038,-0.0315535054335339,
-0.0110288148879857));
#32003=CARTESIAN_POINT('Ctrl Pts',(0.00285808667288348,-0.0315418533076306,
-0.0112609613874801));
#32004=CARTESIAN_POINT('Ctrl Pts',(0.00288017974912521,-0.0315382818902255,
-0.0113330893767142));
#32005=CARTESIAN_POINT('Ctrl Pts',(0.0029235356635223,-0.0315301929040391,
-0.0114963767211787));
#32006=CARTESIAN_POINT('Ctrl Pts',(0.00294329748342001,-0.0315256579285381,
-0.01158785019842));
#32007=CARTESIAN_POINT('Ctrl Pts',(0.00296928999080422,-0.031517839414608,
-0.01174297656792));
#32008=CARTESIAN_POINT('Ctrl Pts',(0.0029778186060514,-0.0315146195824636,
-0.0118061764811226));
#32009=CARTESIAN_POINT('Ctrl Pts',(0.00298708176151363,-0.0315099498587432,
-0.0118964418428674));
#32010=CARTESIAN_POINT('Ctrl Pts',(0.00298947417383292,-0.0315085504569989,
-0.0119233214907006));
#32011=CARTESIAN_POINT('Ctrl Pts',(0.00299300791378566,-0.0315060943842574,
-0.0119701746278096));
#32012=CARTESIAN_POINT('Ctrl Pts',(0.00299431269243673,-0.0315050427904204,
-0.0119901342597551));
#32013=CARTESIAN_POINT('Ctrl Pts',(0.00299659741348077,-0.0315028558999542,
-0.0120314239748961));
#32014=CARTESIAN_POINT('Ctrl Pts',(0.00299754941927381,-0.0315017198077756,
-0.0120527544163292));
#32015=CARTESIAN_POINT('Ctrl Pts',(0.00299942465819,-0.031498759956318,
-0.0121080065268212));
#32016=CARTESIAN_POINT('Ctrl Pts',(0.00300000016225006,-0.0314969256987105,
-0.0121419363032316));
#32017=CARTESIAN_POINT('Ctrl Pts',(0.00299999937983027,-0.0314879988457174,
-0.0123055290472804));
#32018=CARTESIAN_POINT('Ctrl Pts',(0.00299159289392699,-0.0314806719372835,
-0.0124350397607784));
#32019=CARTESIAN_POINT('Ctrl Pts',(0.00295954566551207,-0.0314663367216377,
-0.0126809167156226));
#32020=CARTESIAN_POINT('Ctrl Pts',(0.00293732611516207,-0.0314593704234008,
-0.0127972332192756));
#32021=CARTESIAN_POINT('Ctrl Pts',(0.0028744531151376,-0.0314443185765894,
-0.0130456498495619));
#32022=CARTESIAN_POINT('Ctrl Pts',(0.00283142401875427,-0.0314362555019756,
-0.0131768879571909));
#32023=CARTESIAN_POINT('Ctrl Pts',(0.00276838468732164,-0.0314269139106782,
-0.0133321061977503));
#32024=CARTESIAN_POINT('Ctrl Pts',(0.0027568518141252,-0.031425282738302,
-0.0133593408339047));
#32025=CARTESIAN_POINT('Ctrl Pts',(0.00273923638612753,-0.0314229068615499,
-0.0133992838132518));
#32026=CARTESIAN_POINT('Ctrl Pts',(0.00273346434505124,-0.0314221455117122,
-0.0134121262833714));
#32027=CARTESIAN_POINT('Ctrl Pts',(0.00272297990476607,-0.0314207934097788,
-0.0134350211369915));
#32028=CARTESIAN_POINT('Ctrl Pts',(0.00271830189775692,-0.0314202007195567,
-0.0134450885044606));
#32029=CARTESIAN_POINT('Ctrl Pts',(0.00270772252782384,-0.0314188837085149,
-0.0134675291809873));
#32030=CARTESIAN_POINT('Ctrl Pts',(0.00270179214476104,-0.0314181611189366,
-0.0134798882265156));
#32031=CARTESIAN_POINT('Ctrl Pts',(0.00268369992440968,-0.0314160018911859,
-0.0135169395259518));
#32032=CARTESIAN_POINT('Ctrl Pts',(0.00267128248936854,-0.03141457968553,
-0.0135415060786094));
#32033=CARTESIAN_POINT('Ctrl Pts',(0.00260836656966896,-0.0314076439463513,
-0.0136618357521572));
#32034=CARTESIAN_POINT('Ctrl Pts',(0.00255304433699022,-0.0314023686725732,
-0.0137549949500218));
#32035=CARTESIAN_POINT('Ctrl Pts',(0.00234555301063521,-0.0313844856593905,
-0.0140648811823205));
#32036=CARTESIAN_POINT('Ctrl Pts',(0.00216986257507423,-0.031372258725037,
-0.0142643313843433));
#32037=CARTESIAN_POINT('Ctrl Pts',(0.00194162326719827,-0.0313569468116363,
-0.0144631100612533));
#32038=CARTESIAN_POINT('Ctrl Pts',(0.00191249201525883,-0.0313550042851653,
-0.0144875233746481));
#32039=CARTESIAN_POINT('Ctrl Pts',(0.00186391953869556,-0.0313517796866947,
-0.0145266826544384));
#32040=CARTESIAN_POINT('Ctrl Pts',(0.00184474790698277,-0.0313505104817068,
-0.0145417568936433));
#32041=CARTESIAN_POINT('Ctrl Pts',(0.0018097362839726,-0.0313481979203354,
-0.0145686014810363));
#32042=CARTESIAN_POINT('Ctrl Pts',(0.00179395978156127,-0.0313471577603407,
-0.0145804525498803));
#32043=CARTESIAN_POINT('Ctrl Pts',(0.0017596852443438,-0.0313449015345491,
-0.0146056740082139));
#32044=CARTESIAN_POINT('Ctrl Pts',(0.00174114931429377,-0.0313436835206924,
-0.0146189905985285));
#32045=CARTESIAN_POINT('Ctrl Pts',(0.00168906324631621,-0.0313402661006848,
-0.0146555164768901));
#32046=CARTESIAN_POINT('Ctrl Pts',(0.00165518982470938,-0.0313380494875459,
-0.0146782542558063));
#32047=CARTESIAN_POINT('Ctrl Pts',(0.00150954489042835,-0.031328539967362,
-0.0147717683267744));
#32048=CARTESIAN_POINT('Ctrl Pts',(0.0013936315773998,-0.0313210145901129,
-0.0148357941041013));
#32049=CARTESIAN_POINT('Ctrl Pts',(0.00110419203668995,-0.0313024486817675,
-0.0149715444243269));
#32050=CARTESIAN_POINT('Ctrl Pts',(0.000927422306658285,-0.0312912761316168,
-0.0150350515790807));
#32051=CARTESIAN_POINT('Ctrl Pts',(0.000677576093376061,-0.0312764320854631,
-0.0150991843095618));
#32052=CARTESIAN_POINT('Ctrl Pts',(0.000608664657924585,-0.0312724369399736,
-0.0151143056568378));
#32053=CARTESIAN_POINT('Ctrl Pts',(0.000519680685953666,-0.0312674566004465,
-0.0151305662917295));
#32054=CARTESIAN_POINT('Ctrl Pts',(0.00050004570725103,-0.0312663687127424,
-0.0151339525564994));
#32055=CARTESIAN_POINT('Ctrl Pts',(0.000468444621791647,-0.0312646371653898,
-0.0151390788581003));
#32056=CARTESIAN_POINT('Ctrl Pts',(0.000456499499758228,-0.0312639870672388,
-0.0151409425547589));
#32057=CARTESIAN_POINT('Ctrl Pts',(0.000433288890776407,-0.0312627328709774,
-0.0151444203215003));
#32058=CARTESIAN_POINT('Ctrl Pts',(0.000422025082156765,-0.0312621283866448,
-0.0151460425626311));
#32059=CARTESIAN_POINT('Ctrl Pts',(0.000394099656790599,-0.0312606395336177,
-0.0151499023892932));
#32060=CARTESIAN_POINT('Ctrl Pts',(0.000377427687005065,-0.03125975925898,
-0.0151520641277922));
#32061=CARTESIAN_POINT('Ctrl Pts',(0.000313582607630233,-0.0312564181606006,
-0.0151597973557237));
#32062=CARTESIAN_POINT('Ctrl Pts',(0.000266295691851007,-0.0312540058774051,
-0.0151643886013324));
#32063=CARTESIAN_POINT('Ctrl Pts',(0.000139661459569341,-0.0312476659085832,
-0.0151736541142784));
#32064=CARTESIAN_POINT('Ctrl Pts',(6.02021837856961E-5,-0.0312438128450981,
-0.0151763019387494));
#32065=CARTESIAN_POINT('Ctrl Pts',(-0.000288572217971681,-0.0312271127560565,
-0.0151740613578506));
#32066=CARTESIAN_POINT('Ctrl Pts',(-0.000556394659976168,-0.0312147155435352,
-0.0151360813573633));
#32067=CARTESIAN_POINT('Ctrl Pts',(-0.000851726205064238,-0.0311991931166643,
-0.0150526527310513));
#32068=CARTESIAN_POINT('Ctrl Pts',(-0.000887698667210124,-0.0311972724847522,
-0.0150417568947233));
#32069=CARTESIAN_POINT('Ctrl Pts',(-0.000946434687803124,-0.0311940824632114,
-0.0150227541753678));
#32070=CARTESIAN_POINT('Ctrl Pts',(-0.000969322326243007,-0.0311928257654935,
-0.0150150428667718));
#32071=CARTESIAN_POINT('Ctrl Pts',(-0.00101056608453178,-0.0311905353697205,
-0.015000590173402));
#32072=CARTESIAN_POINT('Ctrl Pts',(-0.00102895427187244,-0.0311895048288794,
-0.0149939440184654));
#32073=CARTESIAN_POINT('Ctrl Pts',(-0.00106847473170203,-0.031187269128904,
-0.0149792215291683));
#32074=CARTESIAN_POINT('Ctrl Pts',(-0.00108958315579977,-0.0311860620337089,
-0.0149710849879555));
#32075=CARTESIAN_POINT('Ctrl Pts',(-0.00114815581022576,-0.031182675446898,
-0.014947743060055));
#32076=CARTESIAN_POINT('Ctrl Pts',(-0.0011854067107046,-0.0311804789028494,
-0.0149320182660841));
#32077=CARTESIAN_POINT('Ctrl Pts',(-0.00134182742489207,-0.031171069675751,
-0.0148622304006374));
#32078=CARTESIAN_POINT('Ctrl Pts',(-0.00145769855270647,-0.0311636277363491,
-0.0148011592425416));
#32079=CARTESIAN_POINT('Ctrl Pts',(-0.00171305811342673,-0.0311462287398832,
-0.0146444400279809));
#32080=CARTESIAN_POINT('Ctrl Pts',(-0.00184920007179521,-0.0311361912019695,
-0.0145441745032702));
#32081=CARTESIAN_POINT('Ctrl Pts',(-0.00204258170369307,-0.0311212761457188,
-0.0143748638842227));
#32082=CARTESIAN_POINT('Ctrl Pts',(-0.00210638558295247,-0.0311162334913952,
-0.0143138265843286));
#32083=CARTESIAN_POINT('Ctrl Pts',(-0.00218204905555556,-0.0311101946113171,
-0.0142347632501576));
#32084=CARTESIAN_POINT('Ctrl Pts',(-0.0021965265517318,-0.0311090363285574,
-0.0142193110122424));
#32085=CARTESIAN_POINT('Ctrl Pts',(-0.00221916517892087,-0.0311072225151594,
-0.0141946295525209));
#32086=CARTESIAN_POINT('Ctrl Pts',(-0.00222743489747744,-0.0311065593823568,
-0.0141855013879904));
#32087=CARTESIAN_POINT('Ctrl Pts',(-0.00224318690042803,-0.0311052956349731,
-0.0141678975476417));
#32088=CARTESIAN_POINT('Ctrl Pts',(-0.00225067781662052,-0.0311046944215979,
-0.0141594301508696));
#32089=CARTESIAN_POINT('Ctrl Pts',(-0.00226874273178424,-0.0311032434619999,
-0.0141387762921927));
#32090=CARTESIAN_POINT('Ctrl Pts',(-0.00227926679560667,-0.0311023972457476,
-0.0141265462931545));
#32091=CARTESIAN_POINT('Ctrl Pts',(-0.00231679023185935,-0.0310993742522334,
-0.0140822220752352));
#32092=CARTESIAN_POINT('Ctrl Pts',(-0.00234321561369952,-0.0310972343076884,
-0.0140496461915277));
#32093=CARTESIAN_POINT('Ctrl Pts',(-0.00248316577396171,-0.031085775467706,
-0.0138695299299743));
#32094=CARTESIAN_POINT('Ctrl Pts',(-0.00258346125922145,-0.0310770765415037,
-0.0137122102260625));
#32095=CARTESIAN_POINT('Ctrl Pts',(-0.00273862325436582,-0.0310609522218785,
-0.0134101444924896));
#32096=CARTESIAN_POINT('Ctrl Pts',(-0.00279814150714647,-0.0310535972509047,
-0.0132685248418041));
#32097=CARTESIAN_POINT('Ctrl Pts',(-0.0028630507036099,-0.0310432847386282,
-0.0130734427079798));
#32098=CARTESIAN_POINT('Ctrl Pts',(-0.00287823778146051,-0.0310406300511755,
-0.0130234811346886));
#32099=CARTESIAN_POINT('Ctrl Pts',(-0.00289878162064657,-0.031036638817784,
-0.0129489604864606));
#32100=CARTESIAN_POINT('Ctrl Pts',(-0.00290514642074537,-0.0310353339747879,
-0.0129246882828097));
#32101=CARTESIAN_POINT('Ctrl Pts',(-0.0029159950978677,-0.0310329806480193,
-0.0128810950030002));
#32102=CARTESIAN_POINT('Ctrl Pts',(-0.00292059329966039,-0.0310319358267159,
-0.0128618037529944));
#32103=CARTESIAN_POINT('Ctrl Pts',(-0.00292998490398528,-0.0310296961654827,
-0.0128205949190631));
#32104=CARTESIAN_POINT('Ctrl Pts',(-0.00293472436702019,-0.0310284997103785,
-0.012798666391128));
#32105=CARTESIAN_POINT('Ctrl Pts',(-0.0029439065293226,-0.0310260388579148,
-0.0127537481998373));
#32106=CARTESIAN_POINT('Ctrl Pts',(-0.00294832691177362,-0.0310247738605681,
-0.01273075558765));
#32107=CARTESIAN_POINT('Ctrl Pts',(-0.00296272745672576,-0.0310203565785813,
-0.0126508149482916));
#32108=CARTESIAN_POINT('Ctrl Pts',(-0.00297132983262019,-0.0310171630659669,
-0.0125936343075038));
#32109=CARTESIAN_POINT('Ctrl Pts',(-0.00299283479013691,-0.0310071339804914,
-0.0124159166586095));
#32110=CARTESIAN_POINT('Ctrl Pts',(-0.00300008853944841,-0.031000148781098,
-0.0122948279177128));
#32111=CARTESIAN_POINT('Ctrl Pts',(-0.00299999918450973,-0.0309930707801491,
-0.0121736412872464));
#32112=CARTESIAN_POINT('',(-0.00299999972093215,-0.0369945846061161,-0.0121745592977555));
#32113=CARTESIAN_POINT('Ctrl Pts',(-0.00299999981352154,-0.0319945472736604,
-0.0121769110534288));
#32114=CARTESIAN_POINT('Ctrl Pts',(-0.00299992166945358,-0.0320055173499198,
-0.0123985404084296));
#32115=CARTESIAN_POINT('Ctrl Pts',(-0.00297528701221253,-0.0320157939746235,
-0.0126194602075733));
#32116=CARTESIAN_POINT('Ctrl Pts',(-0.00290221263423182,-0.0320317016547023,
-0.0129435765333841));
#32117=CARTESIAN_POINT('Ctrl Pts',(-0.00287193455456266,-0.0320370815248905,
-0.0130500529918593));
#32118=CARTESIAN_POINT('Ctrl Pts',(-0.00282675542114908,-0.0320441503505141,
-0.0131809557000143));
#32119=CARTESIAN_POINT('Ctrl Pts',(-0.00281729432308356,-0.0320455899518007,
-0.0132071775153452));
#32120=CARTESIAN_POINT('Ctrl Pts',(-0.00280259606184744,-0.0320477731400695,
-0.0132462020566344));
#32121=CARTESIAN_POINT('Ctrl Pts',(-0.00279763329257718,-0.0320485018376998,
-0.0132591072369983));
#32122=CARTESIAN_POINT('Ctrl Pts',(-0.0027884946320194,-0.0320498294736284,
-0.0132823896872612));
#32123=CARTESIAN_POINT('Ctrl Pts',(-0.00278434967702218,-0.0320504266391192,
-0.0132927785238499));
#32124=CARTESIAN_POINT('Ctrl Pts',(-0.00277481854911974,-0.0320517886265605,
-0.0133162843788565));
#32125=CARTESIAN_POINT('Ctrl Pts',(-0.00276939743826002,-0.0320525554163635,
-0.0133293864979761));
#32126=CARTESIAN_POINT('Ctrl Pts',(-0.00275232871801576,-0.0320549446140336,
-0.0133698254784093));
#32127=CARTESIAN_POINT('Ctrl Pts',(-0.00274036799482192,-0.0320565838122045,
-0.0133970273486267));
#32128=CARTESIAN_POINT('Ctrl Pts',(-0.00266562925274479,-0.0320666026904978,
-0.0135603736836576));
#32129=CARTESIAN_POINT('Ctrl Pts',(-0.00259312580604794,-0.0320753989577528,
-0.0136918243278081));
#32130=CARTESIAN_POINT('Ctrl Pts',(-0.00246031502295989,-0.0320896669141343,
-0.0138950008108519));
#32131=CARTESIAN_POINT('Ctrl Pts',(-0.00240594014769667,-0.0320951245132674,
-0.0139703089356163));
#32132=CARTESIAN_POINT('Ctrl Pts',(-0.00226686810629769,-0.0321080957540019,
-0.0141452108714532));
#32133=CARTESIAN_POINT('Ctrl Pts',(-0.00217898026176169,-0.0321155239350369,
-0.0142420361567347));
#32134=CARTESIAN_POINT('Ctrl Pts',(-0.00205580627442135,-0.0321249357397831,
-0.0143611027083987));
#32135=CARTESIAN_POINT('Ctrl Pts',(-0.00202598825148812,-0.0321271458988904,
-0.0143887758558819));
#32136=CARTESIAN_POINT('Ctrl Pts',(-0.00197851292600666,-0.0321305613644986,
-0.0144310719609503));
#32137=CARTESIAN_POINT('Ctrl Pts',(-0.00196123594672582,-0.0321317837147886,
-0.0144461128021712));
#32138=CARTESIAN_POINT('Ctrl Pts',(-0.00192863706421125,-0.0321340525430364,
-0.0144738425658064));
#32139=CARTESIAN_POINT('Ctrl Pts',(-0.00191335802319091,-0.032135100934317,
-0.0144865797423342));
#32140=CARTESIAN_POINT('Ctrl Pts',(-0.00187882236376268,-0.0321374378502508,
-0.0145147925241981));
#32141=CARTESIAN_POINT('Ctrl Pts',(-0.0018594988906304,-0.0321387230276193,
-0.0145301842222729));
#32142=CARTESIAN_POINT('Ctrl Pts',(-0.00180938542209416,-0.0321420006718816,
-0.0145690991062663));
#32143=CARTESIAN_POINT('Ctrl Pts',(-0.00177832543406964,-0.0321439796091278,
-0.0145922679819327));
#32144=CARTESIAN_POINT('Ctrl Pts',(-0.00153333466509974,-0.0321592102277868,
-0.0147677333599231));
#32145=CARTESIAN_POINT('Ctrl Pts',(-0.00130070754058425,-0.0321713400748168,
-0.0148919384817944));
#32146=CARTESIAN_POINT('Ctrl Pts',(-0.000978870743146697,-0.0321878039105082,
-0.0150128242086367));
#32147=CARTESIAN_POINT('Ctrl Pts',(-0.000901740788853144,-0.0321917386608914,
-0.0150382743173766));
#32148=CARTESIAN_POINT('Ctrl Pts',(-0.000777222210865428,-0.032198202836921,
-0.0150738283954862));
#32149=CARTESIAN_POINT('Ctrl Pts',(-0.000730455062710333,-0.0322006553988329,
-0.0150859682357734));
#32150=CARTESIAN_POINT('Ctrl Pts',(-0.000666774969706172,-0.0322040525418524,
-0.0151008666680006));
#32151=CARTESIAN_POINT('Ctrl Pts',(-0.000650099628271567,-0.0322049474242707,
-0.0151046179730234));
#32152=CARTESIAN_POINT('Ctrl Pts',(-0.000622088780710364,-0.0322064608534237,
-0.0151106683247944));
#32153=CARTESIAN_POINT('Ctrl Pts',(-0.000610770112324474,-0.032207075195398,
-0.0151130447387011));
#32154=CARTESIAN_POINT('Ctrl Pts',(-0.000587450282326003,-0.0322083471450999,
-0.0151178002350297));
#32155=CARTESIAN_POINT('Ctrl Pts',(-0.000575447915660388,-0.032209005132621,
-0.0151201714364311));
#32156=CARTESIAN_POINT('Ctrl Pts',(-0.000543547495604881,-0.0322107621833263,
-0.015126271215151));
#32157=CARTESIAN_POINT('Ctrl Pts',(-0.000523625946324464,-0.0322118679167358,
-0.0151298718474032));
#32158=CARTESIAN_POINT('Ctrl Pts',(-0.000432001044636205,-0.0322169875534955,
-0.015145476245953));
#32159=CARTESIAN_POINT('Ctrl Pts',(-0.000359916816942563,-0.032221110388206,
-0.0151550719481401));
#32160=CARTESIAN_POINT('Ctrl Pts',(-6.04147719155483E-5,-0.032238446194825,
-0.0151839130931893));
#32161=CARTESIAN_POINT('Ctrl Pts',(0.00016849004050524,-0.0322521145788547,
-0.0151798002863055));
#32162=CARTESIAN_POINT('Ctrl Pts',(0.000498703642215855,-0.0322711847942824,
-0.0151359707762295));
#32163=CARTESIAN_POINT('Ctrl Pts',(0.000601888687158601,-0.0322770618066293,
-0.0151167263528632));
#32164=CARTESIAN_POINT('Ctrl Pts',(0.000735151277624789,-0.0322845272222606,
-0.0150845623862352));
#32165=CARTESIAN_POINT('Ctrl Pts',(0.000766317425899855,-0.0322862644083889,
-0.0150765073058159));
#32166=CARTESIAN_POINT('Ctrl Pts',(0.000817715459811999,-0.0322891156359211,
-0.0150623369186903));
#32167=CARTESIAN_POINT('Ctrl Pts',(0.000838022619209465,-0.0322902385815438,
-0.0150565067631455));
#32168=CARTESIAN_POINT('Ctrl Pts',(0.000877620389305425,-0.0322924217567312,
-0.0150446841287081));
#32169=CARTESIAN_POINT('Ctrl Pts',(0.000896915375805811,-0.032293482515093,
-0.0150387103880561));
#32170=CARTESIAN_POINT('Ctrl Pts',(0.000943240260131015,-0.032296022587275,
-0.0150238538555277));
#32171=CARTESIAN_POINT('Ctrl Pts',(0.000970207238362803,-0.0322974957037417,
-0.0150147804456876));
#32172=CARTESIAN_POINT('Ctrl Pts',(0.0010609398053361,-0.0323024367613863,
-0.0149828083417565));
#32173=CARTESIAN_POINT('Ctrl Pts',(0.00112405938926173,-0.0323058476588138,
-0.014958133157303));
#32174=CARTESIAN_POINT('Ctrl Pts',(0.00140089283297222,-0.03232077438795,
-0.0148389508221372));
#32175=CARTESIAN_POINT('Ctrl Pts',(0.00160395511914783,-0.0323315630356229,
-0.0147218138867613));
#32176=CARTESIAN_POINT('Ctrl Pts',(0.00185109379034802,-0.0323463686431329,
-0.0145378430138683));
#32177=CARTESIAN_POINT('Ctrl Pts',(0.00190913996170871,-0.0323499928684846,
-0.0144911777132555));
#32178=CARTESIAN_POINT('Ctrl Pts',(0.0019998457344721,-0.0323560011650617,
-0.0144125243050791));
#32179=CARTESIAN_POINT('Ctrl Pts',(0.00203361676734141,-0.0323583210968015,
-0.0143818638576635));
#32180=CARTESIAN_POINT('Ctrl Pts',(0.00207880516695753,-0.0323615617791868,
-0.0143389180477261));
#32181=CARTESIAN_POINT('Ctrl Pts',(0.00209083931783159,-0.0323624385407105,
-0.0143272879254064));
#32182=CARTESIAN_POINT('Ctrl Pts',(0.00211097734140315,-0.0323639303524099,
-0.0143074974665686));
#32183=CARTESIAN_POINT('Ctrl Pts',(0.00211913293054328,-0.0323645414725223,
-0.0142993899277437));
#32184=CARTESIAN_POINT('Ctrl Pts',(0.00213595447204794,-0.0323658169319017,
-0.0142824740809798));
#32185=CARTESIAN_POINT('Ctrl Pts',(0.00214461287168771,-0.0323664817657812,
-0.0142736588776297));
#32186=CARTESIAN_POINT('Ctrl Pts',(0.00216770254568187,-0.0323682765492183,
-0.0142498587067067));
#32187=CARTESIAN_POINT('Ctrl Pts',(0.00218203257340995,-0.0323694136597469,
-0.0142347769399615));
#32188=CARTESIAN_POINT('Ctrl Pts',(0.00225038940708793,-0.0323749456846762,
-0.014161319011261));
#32189=CARTESIAN_POINT('Ctrl Pts',(0.00230223365563165,-0.0323794710952268,
-0.0141009623659906));
#32190=CARTESIAN_POINT('Ctrl Pts',(0.00244882559842434,-0.0323931170667211,
-0.0139159003603096));
#32191=CARTESIAN_POINT('Ctrl Pts',(0.00253627997155106,-0.0324024102409782,
-0.0137857584550647));
#32192=CARTESIAN_POINT('Ctrl Pts',(0.0026659965369315,-0.0324178222284253,
-0.0135557177743364));
#32193=CARTESIAN_POINT('Ctrl Pts',(0.00271374348830112,-0.0324240166117465,
-0.0134592717120003));
#32194=CARTESIAN_POINT('Ctrl Pts',(0.00278391722210011,-0.0324340017272394,
-0.0132959997482678));
#32195=CARTESIAN_POINT('Ctrl Pts',(0.00280935476756636,-0.0324378775121089,
-0.0132305807779069));
#32196=CARTESIAN_POINT('Ctrl Pts',(0.00284173914581808,-0.0324432025059446,
-0.0131377830954056));
#32197=CARTESIAN_POINT('Ctrl Pts',(0.00285062870797352,-0.0324447135945916,
-0.0131111106693456));
#32198=CARTESIAN_POINT('Ctrl Pts',(0.00286530169601771,-0.0324472971696995,
-0.0130649314129799));
#32199=CARTESIAN_POINT('Ctrl Pts',(0.00287126392981967,-0.0324483753352332,
-0.0130454837809158));
#32200=CARTESIAN_POINT('Ctrl Pts',(0.00288233821074679,-0.0324504346642358,
-0.0130080056730721));
#32201=CARTESIAN_POINT('Ctrl Pts',(0.00288747998499075,-0.0324514167348727,
-0.0129899850404862));
#32202=CARTESIAN_POINT('Ctrl Pts',(0.0029005917386521,-0.032453992290725,
-0.01294234423061));
#32203=CARTESIAN_POINT('Ctrl Pts',(0.0029082769902684,-0.0324555767292192,
-0.0129126475847428));
#32204=CARTESIAN_POINT('Ctrl Pts',(0.00293497830326661,-0.0324613792018762,
-0.0128025350550199));
#32205=CARTESIAN_POINT('Ctrl Pts',(0.00295112583945495,-0.0324655084800149,
-0.0127214588180163));
#32206=CARTESIAN_POINT('Ctrl Pts',(0.00300123153964023,-0.0324814029094778,
-0.0124013705008864));
#32207=CARTESIAN_POINT('Ctrl Pts',(0.00300964554019078,-0.0324924682081842,
-0.0121593119664037));
#32208=CARTESIAN_POINT('Ctrl Pts',(0.00298408003833383,-0.0325069813386115,
-0.0118619600557041));
#32209=CARTESIAN_POINT('Ctrl Pts',(0.0029775629986748,-0.0325097976698275,
-0.0118052043441688));
#32210=CARTESIAN_POINT('Ctrl Pts',(0.00296402610454635,-0.0325145922894124,
-0.0117111064459493));
#32211=CARTESIAN_POINT('Ctrl Pts',(0.00295790980565575,-0.032516534315531,
-0.0116736484394402));
#32212=CARTESIAN_POINT('Ctrl Pts',(0.00294827786134798,-0.0325193253770335,
-0.011620964776072));
#32213=CARTESIAN_POINT('Ctrl Pts',(0.00294535114104303,-0.0325201447529038,
-0.0116056338180784));
#32214=CARTESIAN_POINT('Ctrl Pts',(0.00294009660696255,-0.0325215694117716,
-0.0115792294792531));
#32215=CARTESIAN_POINT('Ctrl Pts',(0.00293782550315667,-0.0325221716079568,
-0.0115681450205364));
#32216=CARTESIAN_POINT('Ctrl Pts',(0.0029328430745997,-0.0325234649045223,
-0.0115445083735146));
#32217=CARTESIAN_POINT('Ctrl Pts',(0.00293011382399383,-0.0325241569266596,
-0.0115319605424998));
#32218=CARTESIAN_POINT('Ctrl Pts',(0.00292239195393721,-0.032526070355148,
-0.0114975250005768));
#32219=CARTESIAN_POINT('Ctrl Pts',(0.00291723416172802,-0.0325273003337825,
-0.0114756756069955));
#32220=CARTESIAN_POINT('Ctrl Pts',(0.00288134451692469,-0.0325355453891919,
-0.0113309256608267));
#32221=CARTESIAN_POINT('Ctrl Pts',(0.00284310164768706,-0.0325428910871948,
-0.011210029056896));
#32222=CARTESIAN_POINT('Ctrl Pts',(0.00273179299120794,-0.032560942920508,
-0.0109227708690137));
#32223=CARTESIAN_POINT('Ctrl Pts',(0.00265103524736783,-0.0325716738933144,
-0.0107598978359552));
#32224=CARTESIAN_POINT('Ctrl Pts',(0.00250625269746859,-0.0325874331740844,
-0.010524264173937));
#32225=CARTESIAN_POINT('Ctrl Pts',(0.00245262243289094,-0.0325927436274197,
-0.0104456235235701));
#32226=CARTESIAN_POINT('Ctrl Pts',(0.00237654438931704,-0.0325996170188491,
-0.0103447302704393));
#32227=CARTESIAN_POINT('Ctrl Pts',(0.00235735903153334,-0.032601300519603,
-0.0103200965054498));
#32228=CARTESIAN_POINT('Ctrl Pts',(0.00232467622422405,-0.0326040876941123,
-0.010279457109224));
#32229=CARTESIAN_POINT('Ctrl Pts',(0.00231138980330054,-0.0326051994718929,
-0.0102632855842512));
#32230=CARTESIAN_POINT('Ctrl Pts',(0.00228486449201811,-0.0326073781131245,
-0.0102316805503514));
#32231=CARTESIAN_POINT('Ctrl Pts',(0.00227163578727992,-0.032608445294884,
-0.0102162399951401));
#32232=CARTESIAN_POINT('Ctrl Pts',(0.00223902535675638,-0.0326110301620434,
-0.0101789510957121));
#32233=CARTESIAN_POINT('Ctrl Pts',(0.00221947940071062,-0.0326125410703105,
-0.010157248774908));
#32234=CARTESIAN_POINT('Ctrl Pts',(0.00215033974763172,-0.0326177579253327,
-0.0100826999844979));
#32235=CARTESIAN_POINT('Ctrl Pts',(0.00209914915478378,-0.0326213975309861,
-0.0100313660262812));
#32236=CARTESIAN_POINT('Ctrl Pts',(0.00189354722922503,-0.0326352770896497,
-0.00983961252477843));
#32237=CARTESIAN_POINT('Ctrl Pts',(0.00172652019459439,-0.0326449848259004,
-0.00971360406131355));
#32238=CARTESIAN_POINT('Ctrl Pts',(0.00144757581956135,-0.0326605420522651,
-0.00954560551421155));
#32239=CARTESIAN_POINT('Ctrl Pts',(0.00134395058867059,-0.032666210434021,
-0.00949117986156228));
#32240=CARTESIAN_POINT('Ctrl Pts',(0.0012113819371863,-0.0326736318921978,
-0.00943115458018942));
#32241=CARTESIAN_POINT('Ctrl Pts',(0.00118517422587893,-0.0326751071197383,
-0.00941973661116304));
#32242=CARTESIAN_POINT('Ctrl Pts',(0.00114592700423578,-0.0326773338713265,
-0.00940330097383683));
#32243=CARTESIAN_POINT('Ctrl Pts',(0.00113300847073552,-0.032678069619199,
-0.00939799677189846));
#32244=CARTESIAN_POINT('Ctrl Pts',(0.00110967773246729,-0.0326794041848032,
-0.00938860725748957));
#32245=CARTESIAN_POINT('Ctrl Pts',(0.00109927907879504,-0.032680001124699,
-0.00938448971386351));
#32246=CARTESIAN_POINT('Ctrl Pts',(0.0010757778988961,-0.0326813550277411,
-0.00937533566589626));
#32247=CARTESIAN_POINT('Ctrl Pts',(0.00106266297292496,-0.0326821138494114,
-0.0093703329387648));
#32248=CARTESIAN_POINT('Ctrl Pts',(0.00102238496414359,-0.0326844532311081,
-0.00935529171375322));
#32249=CARTESIAN_POINT('Ctrl Pts',(0.000995111938646888,-0.0326860496282743,
-0.00934555459038613));
#32250=CARTESIAN_POINT('Ctrl Pts',(0.000805473912642518,-0.0326972141969443,
-0.0092809290075445));
#32251=CARTESIAN_POINT('Ctrl Pts',(0.000638816061479365,-0.0327073312237352,
-0.00923965144348039));
#32252=CARTESIAN_POINT('Ctrl Pts',(0.000268469143708647,-0.0327293653127623,
-0.00918096143610414));
#32253=CARTESIAN_POINT('Ctrl Pts',(6.46302958511912E-5,-0.0327411840007304,
-0.00916964339219376));
#32254=CARTESIAN_POINT('Ctrl Pts',(-0.000179255189209165,-0.0327545947917013,
-0.00918093972414194));
#32255=CARTESIAN_POINT('Ctrl Pts',(-0.00021966381359147,-0.0327567947543597,
-0.0091836320890782));
#32256=CARTESIAN_POINT('Ctrl Pts',(-0.000282790289156459,-0.0327601982062204,
-0.00918912386090277));
#32257=CARTESIAN_POINT('Ctrl Pts',(-0.000305550639576867,-0.0327614185395813,
-0.00919136642020448));
#32258=CARTESIAN_POINT('Ctrl Pts',(-0.000348061143262737,-0.0327636856364911,
-0.0091960463575681));
#32259=CARTESIAN_POINT('Ctrl Pts',(-0.000367816883783583,-0.0327647342841296,
-0.00919842038909919));
#32260=CARTESIAN_POINT('Ctrl Pts',(-0.000412099716339356,-0.0327670743331952,
-0.00920418930028557));
#32261=CARTESIAN_POINT('Ctrl Pts',(-0.000436611481917395,-0.032768362348695,
-0.00920769165267517));
#32262=CARTESIAN_POINT('Ctrl Pts',(-0.000499547970773524,-0.0327716523320715,
-0.00921748082835111));
#32263=CARTESIAN_POINT('Ctrl Pts',(-0.000537899259255123,-0.0327736405948655,
-0.00922421300765051));
#32264=CARTESIAN_POINT('Ctrl Pts',(-0.000832889335224644,-0.0327888299829616,
-0.00928193625555256));
#32265=CARTESIAN_POINT('Ctrl Pts',(-0.0010819778461849,-0.032800919810724,
-0.00936555331976436));
#32266=CARTESIAN_POINT('Ctrl Pts',(-0.00141634338670296,-0.0328187387356199,
-0.00952893421971835));
#32267=CARTESIAN_POINT('Ctrl Pts',(-0.00151285702359624,-0.0328241128642027,
-0.00958288802923117));
#32268=CARTESIAN_POINT('Ctrl Pts',(-0.00162969908636198,-0.0328311746570709,
-0.00965695329224874));
#32269=CARTESIAN_POINT('Ctrl Pts',(-0.00165302178684557,-0.0328326135581808,
-0.00967219692814457));
#32270=CARTESIAN_POINT('Ctrl Pts',(-0.00168759364462411,-0.0328347959268218,
-0.00969548661783823));
#32271=CARTESIAN_POINT('Ctrl Pts',(-0.00169900555087693,-0.0328355245242688,
-0.00970328958785137));
#32272=CARTESIAN_POINT('Ctrl Pts',(-0.0017195536696144,-0.0328368521303197,
-0.00971754892674381));
#32273=CARTESIAN_POINT('Ctrl Pts',(-0.00172870824484938,-0.0328374493685929,
-0.00972397789350106));
#32274=CARTESIAN_POINT('Ctrl Pts',(-0.00174938946421828,-0.0328388117345902,
-0.00973867505776245));
#32275=CARTESIAN_POINT('Ctrl Pts',(-0.00176089351910897,-0.0328395788335015,
-0.00974697387109865));
#32276=CARTESIAN_POINT('Ctrl Pts',(-0.00179633299833518,-0.032841969710869,
-0.00977292336533869));
#32277=CARTESIAN_POINT('Ctrl Pts',(-0.0018200644900702,-0.0328436103089866,
-0.00979084813585035));
#32278=CARTESIAN_POINT('Ctrl Pts',(-0.00195506528379238,-0.0328531547718727,
-0.00989600468785276));
#32279=CARTESIAN_POINT('Ctrl Pts',(-0.00206031650086878,-0.0328614287151167,
-0.0099906576487612));
#32280=CARTESIAN_POINT('Ctrl Pts',(-0.00224502743731311,-0.0328770569085845,
-0.0101820185758428));
#32281=CARTESIAN_POINT('Ctrl Pts',(-0.00232589572411779,-0.0328843895324159,
-0.0102769755549302));
#32282=CARTESIAN_POINT('Ctrl Pts',(-0.0024489312183982,-0.0328962135913298,
-0.0104411419692128));
#32283=CARTESIAN_POINT('Ctrl Pts',(-0.00249462283158707,-0.0329007898126726,
-0.0105075170366111));
#32284=CARTESIAN_POINT('Ctrl Pts',(-0.00256824451806549,-0.032908478129321,
-0.0106242660786101));
#32285=CARTESIAN_POINT('Ctrl Pts',(-0.00259749695443269,-0.0329116327346472,
-0.0106737504437575));
#32286=CARTESIAN_POINT('Ctrl Pts',(-0.00263794261370985,-0.0329161475994535,
-0.010746888606416));
#32287=CARTESIAN_POINT('Ctrl Pts',(-0.00265027569224967,-0.0329175472222114,
-0.0107698945020977));
#32288=CARTESIAN_POINT('Ctrl Pts',(-0.00267154137063943,-0.0329200026785584,
-0.0108108375164946));
#32289=CARTESIAN_POINT('Ctrl Pts',(-0.00268059734261315,-0.0329210627237353,
-0.0108287084315491));
#32290=CARTESIAN_POINT('Ctrl Pts',(-0.00269924922945755,-0.0329232773528835,
-0.0108664486919383));
#32291=CARTESIAN_POINT('Ctrl Pts',(-0.00270880634880097,-0.0329244305671278,
-0.0108863359373756));
#32292=CARTESIAN_POINT('Ctrl Pts',(-0.00273365435223098,-0.0329274801698911,
-0.0109395372340126));
#32293=CARTESIAN_POINT('Ctrl Pts',(-0.0027485557856385,-0.0329293634497668,
-0.0109730296335553));
#32294=CARTESIAN_POINT('Ctrl Pts',(-0.00282912690062542,-0.0329398794232708,
-0.0111634424770784));
#32295=CARTESIAN_POINT('Ctrl Pts',(-0.00288197279446224,-0.0329480801035526,
-0.0113254561754642));
#32296=CARTESIAN_POINT('Ctrl Pts',(-0.00294890414246313,-0.0329620206730747,
-0.011610946592213));
#32297=CARTESIAN_POINT('Ctrl Pts',(-0.0029695988553946,-0.0329678079904462,
-0.0117324161747555));
#32298=CARTESIAN_POINT('Ctrl Pts',(-0.00299010405574497,-0.0329770485944898,
-0.0119229274919511));
#32299=CARTESIAN_POINT('Ctrl Pts',(-0.00299509980891963,-0.0329803971854066,
-0.0119912728145086));
#32300=CARTESIAN_POINT('Ctrl Pts',(-0.00299941996449915,-0.0329859960547779,
-0.012102794483972));
#32301=CARTESIAN_POINT('Ctrl Pts',(-0.00300015994582249,-0.0329881925506409,
-0.0121458923110202));
#32302=CARTESIAN_POINT('Ctrl Pts',(-0.00299989950004612,-0.0329912869608121,
-0.0122053736321074));
#32303=CARTESIAN_POINT('Ctrl Pts',(-0.00299969353153812,-0.0329921458709777,
-0.0122217570393376));
#32304=CARTESIAN_POINT('Ctrl Pts',(-0.00299911592893773,-0.0329936164888288,
-0.01224957198816));
#32305=CARTESIAN_POINT('Ctrl Pts',(-0.0029988131011394,-0.0329942245314662,
-0.0122610048264721));
#32306=CARTESIAN_POINT('Ctrl Pts',(-0.00299804286267508,-0.032995504184675,
-0.0122849172308662));
#32307=CARTESIAN_POINT('Ctrl Pts',(-0.00299756289825817,-0.0329961764108415,
-0.0122973959137909));
#32308=CARTESIAN_POINT('Ctrl Pts',(-0.00299604856014054,-0.0329980120866952,
-0.0123312606805601));
#32309=CARTESIAN_POINT('Ctrl Pts',(-0.00299486313982953,-0.0329991832445347,
-0.0123526389055684));
#32310=CARTESIAN_POINT('Ctrl Pts',(-0.00298757625331354,-0.0330052711742289,
-0.0124627225053163));
#32311=CARTESIAN_POINT('Ctrl Pts',(-0.00297776251179711,-0.0330103511285655,
-0.0125511315738183));
#32312=CARTESIAN_POINT('Ctrl Pts',(-0.00293115631127013,-0.0330278680810998,
-0.0128494225515542));
#32313=CARTESIAN_POINT('Ctrl Pts',(-0.00287594820590763,-0.0330405784405571,
-0.0130558001791282));
#32314=CARTESIAN_POINT('Ctrl Pts',(-0.00276260918550312,-0.0330586007414142,
-0.013349917944923));
#32315=CARTESIAN_POINT('Ctrl Pts',(-0.0027210254768088,-0.033064319410711,
-0.01344331568927));
#32316=CARTESIAN_POINT('Ctrl Pts',(-0.0026602938011974,-0.0330716203207372,
-0.0135628847842095));
#32317=CARTESIAN_POINT('Ctrl Pts',(-0.00264538053097433,-0.0330733431747509,
-0.0135911205535627));
#32318=CARTESIAN_POINT('Ctrl Pts',(-0.00261988110033155,-0.0330761772561545,
-0.0136375875585848));
#32319=CARTESIAN_POINT('Ctrl Pts',(-0.00260954873224065,-0.0330772971725537,
-0.0136559544676992));
#32320=CARTESIAN_POINT('Ctrl Pts',(-0.00258891961630967,-0.0330794789079732,
-0.0136917373424804));
#32321=CARTESIAN_POINT('Ctrl Pts',(-0.00257863854166791,-0.0330805412011469,
-0.0137091610014726));
#32322=CARTESIAN_POINT('Ctrl Pts',(-0.00255337899631024,-0.0330830924035305,
-0.0137509964225757));
#32323=CARTESIAN_POINT('Ctrl Pts',(-0.00253822553245452,-0.0330845749708349,
-0.0137753005087406));
#32324=CARTESIAN_POINT('Ctrl Pts',(-0.00248535592403487,-0.0330895913838888,
-0.0138574520198853));
#32325=CARTESIAN_POINT('Ctrl Pts',(-0.00244599060993135,-0.0330930656584217,
-0.0139142143502755));
#32326=CARTESIAN_POINT('Ctrl Pts',(-0.00227790742465114,-0.0331069760118501,
-0.0141395506315653));
#32327=CARTESIAN_POINT('Ctrl Pts',(-0.00213345448280931,-0.033116842293934,
-0.014295603992161));
#32328=CARTESIAN_POINT('Ctrl Pts',(-0.00188478915500416,-0.0331326118771023,
-0.014512843740485));
#32329=CARTESIAN_POINT('Ctrl Pts',(-0.00179132123783731,-0.0331383334318685,
-0.0145852345641472));
#32330=CARTESIAN_POINT('Ctrl Pts',(-0.00167013892449132,-0.0331458199071841,
-0.0146681334670934));
#32331=CARTESIAN_POINT('Ctrl Pts',(-0.00164620846690638,-0.0331473015546009,
-0.0146840044173829));
#32332=CARTESIAN_POINT('Ctrl Pts',(-0.00161028606276926,-0.0331495361484292,
-0.0147070930053033));
#32333=CARTESIAN_POINT('Ctrl Pts',(-0.00159846485418756,-0.0331502731562743,
-0.0147145745813318));
#32334=CARTESIAN_POINT('Ctrl Pts',(-0.00157709953040147,-0.0331516089681638,
-0.0147278881935737));
#32335=CARTESIAN_POINT('Ctrl Pts',(-0.00156757454384238,-0.0331522058755729,
-0.0147337499100779));
#32336=CARTESIAN_POINT('Ctrl Pts',(-0.00154604276038328,-0.0331535583738044,
-0.0147468352225556));
#32337=CARTESIAN_POINT('Ctrl Pts',(-0.00153401806878773,-0.0331543158040819,
-0.0147540280054991));
#32338=CARTESIAN_POINT('Ctrl Pts',(-0.00149710022190958,-0.0331566466073993,
-0.0147757613656154));
#32339=CARTESIAN_POINT('Ctrl Pts',(-0.00147204812588664,-0.0331582356568215,
-0.0147900272076437));
#32340=CARTESIAN_POINT('Ctrl Pts',(-0.00129101856542265,-0.0331697496668045,
-0.0148896866967588));
#32341=CARTESIAN_POINT('Ctrl Pts',(-0.00112793567096009,-0.0331802654276589,
-0.0149614185908662));
#32342=CARTESIAN_POINT('Ctrl Pts',(-0.00077233170150796,-0.0332023115359165,
-0.0150814541759144));
#32343=CARTESIAN_POINT('Ctrl Pts',(-0.000579384430463109,-0.033213755814049,
-0.015125996809585));
#32344=CARTESIAN_POINT('Ctrl Pts',(-0.000343359078784814,-0.0332268266714737,
-0.0151564132071683));
#32345=CARTESIAN_POINT('Ctrl Pts',(-0.000303179887337522,-0.0332290219563693,
-0.0151607678696518));
#32346=CARTESIAN_POINT('Ctrl Pts',(-0.000240159612160641,-0.0332324198479801,
-0.0151663123768961));
#32347=CARTESIAN_POINT('Ctrl Pts',(-0.000217373075255318,-0.033233639209211,
-0.0151680550169615));
#32348=CARTESIAN_POINT('Ctrl Pts',(-0.000174711645488774,-0.0332359054017205,
-0.0151708277101129));
#32349=CARTESIAN_POINT('Ctrl Pts',(-0.000154842220985072,-0.0332369541039347,
-0.0151719206871323));
#32350=CARTESIAN_POINT('Ctrl Pts',(-0.000110204933870383,-0.033239295422961,
-0.0151739308507323));
#32351=CARTESIAN_POINT('Ctrl Pts',(-8.54334777083388E-5,-0.0332405846366736,
-0.0151747389757358));
#32352=CARTESIAN_POINT('Ctrl Pts',(-2.16470892373925E-5,-0.0332438799663497,
-0.0151760288802137));
#32353=CARTESIAN_POINT('Ctrl Pts',(1.73728845334115E-5,-0.0332458722988661,
-0.0151760567039553));
#32354=CARTESIAN_POINT('Ctrl Pts',(0.000317576084153704,-0.0332610438022461,
-0.0151704135419899));
#32355=CARTESIAN_POINT('Ctrl Pts',(0.000576993607931816,-0.0332731161602666,
-0.0151314117228422));
#32356=CARTESIAN_POINT('Ctrl Pts',(0.000934497588884458,-0.0332909244266531,
-0.0150287415744288));
#32357=CARTESIAN_POINT('Ctrl Pts',(0.00103912771924805,-0.0332963084976614,
-0.0149923168412694));
#32358=CARTESIAN_POINT('Ctrl Pts',(0.00116728565105564,-0.0333033824397116,
-0.0149395866110209));
#32359=CARTESIAN_POINT('Ctrl Pts',(0.00119292487951236,-0.0333048225880542,
-0.0149286169536524));
#32360=CARTESIAN_POINT('Ctrl Pts',(0.00123104408750131,-0.0333070064780859,
-0.0149116752302599));
#32361=CARTESIAN_POINT('Ctrl Pts',(0.0012436423648252,-0.033307735318794,
-0.0149059713988036));
#32362=CARTESIAN_POINT('Ctrl Pts',(0.00126635932555961,-0.0333090631555048,
-0.01489549649891));
#32363=CARTESIAN_POINT('Ctrl Pts',(0.00127649136085391,-0.0333096603774527,
-0.0148907556679226));
#32364=CARTESIAN_POINT('Ctrl Pts',(0.00129940624072964,-0.0333110224300769,
-0.0148798770447648));
#32365=CARTESIAN_POINT('Ctrl Pts',(0.00131217218915115,-0.033311789227905,
-0.014873705245706));
#32366=CARTESIAN_POINT('Ctrl Pts',(0.00135155033166291,-0.0333141782228819,
-0.0148543219627419));
#32367=CARTESIAN_POINT('Ctrl Pts',(0.00137800965682989,-0.0333158172033075,
-0.014840805819731));
#32368=CARTESIAN_POINT('Ctrl Pts',(0.00152738606777894,-0.0333252451031987,
-0.0147616809253467));
#32369=CARTESIAN_POINT('Ctrl Pts',(0.00164580754532204,-0.0333333934480495,
-0.0146879688496514));
#32370=CARTESIAN_POINT('Ctrl Pts',(0.00185498249976198,-0.0333485631073666,
-0.0145366102096565));
#32371=CARTESIAN_POINT('Ctrl Pts',(0.00194707191897057,-0.0333555622518051,
-0.0144612517746332));
#32372=CARTESIAN_POINT('Ctrl Pts',(0.00209695039410642,-0.0333673462252851,
-0.0143229517386088));
#32373=CARTESIAN_POINT('Ctrl Pts',(0.00215697483423139,-0.0333721903951545,
-0.0142626436339962));
#32374=CARTESIAN_POINT('Ctrl Pts',(0.00225466401188813,-0.0333802691525081,
-0.0141557671987391));
#32375=CARTESIAN_POINT('Ctrl Pts',(0.00229364461872961,-0.0333835522967017,
-0.0141104757181992));
#32376=CARTESIAN_POINT('Ctrl Pts',(0.00234791883705563,-0.0333882133296866,
-0.0140434663717243));
#32377=CARTESIAN_POINT('Ctrl Pts',(0.00236431604857692,-0.0333896342497562,
-0.0140226643717949));
#32378=CARTESIAN_POINT('Ctrl Pts',(0.0023926595887327,-0.0333921138242862,
-0.013985710599464));
#32379=CARTESIAN_POINT('Ctrl Pts',(0.00240472301958964,-0.0333931769662321,
-0.0139696511084833));
#32380=CARTESIAN_POINT('Ctrl Pts',(0.00242958983414122,-0.0333953854682937,
-0.013935845336898));
#32381=CARTESIAN_POINT('Ctrl Pts',(0.00244236219473859,-0.0333965296130096,
-0.0139180776470631));
#32382=CARTESIAN_POINT('Ctrl Pts',(0.00247551106089169,-0.0333995263092527,
-0.0138708830792354));
#32383=CARTESIAN_POINT('Ctrl Pts',(0.00249555760827842,-0.0334013665769486,
-0.0138412281309592));
#32384=CARTESIAN_POINT('Ctrl Pts',(0.00259379487779923,-0.0334105408202969,
-0.0136901467714854));
#32385=CARTESIAN_POINT('Ctrl Pts',(0.00266367878286712,-0.0334175734428608,
-0.0135635411664959));
#32386=CARTESIAN_POINT('Ctrl Pts',(0.00279927504774821,-0.0334330493966487,
-0.0132695664113552));
#32387=CARTESIAN_POINT('Ctrl Pts',(0.00285962265991561,-0.0334413873851521,
-0.0131003539904685));
#32388=CARTESIAN_POINT('Ctrl Pts',(0.00292339910848192,-0.0334538454397706,
-0.0128536725389161));
#32389=CARTESIAN_POINT('Ctrl Pts',(0.00293953111900778,-0.033457612076349,
-0.0127798868024211));
#32390=CARTESIAN_POINT('Ctrl Pts',(0.00295636485685824,-0.0334625383779,
-0.0126860497290093));
#32391=CARTESIAN_POINT('Ctrl Pts',(0.00295967400567624,-0.0334635726975199,
-0.0126664889116386));
#32392=CARTESIAN_POINT('Ctrl Pts',(0.00296469589355574,-0.033465256872757,
-0.0126349020633047));
#32393=CARTESIAN_POINT('Ctrl Pts',(0.00296653006756486,-0.033465900280923,
-0.0126228956433011));
#32394=CARTESIAN_POINT('Ctrl Pts',(0.00296995666212803,-0.0334671600741279,
-0.0125995150956484));
#32395=CARTESIAN_POINT('Ctrl Pts',(0.00297155675805709,-0.0334677760411439,
-0.0125881424124412));
#32396=CARTESIAN_POINT('Ctrl Pts',(0.00297539876266702,-0.0334693267225163,
-0.0125596504977695));
#32397=CARTESIAN_POINT('Ctrl Pts',(0.00297755824133778,-0.0334702657784238,
-0.0125425206941243));
#32398=CARTESIAN_POINT('Ctrl Pts',(0.00298491514385364,-0.0334737261871321,
-0.0124798050174858));
#32399=CARTESIAN_POINT('Ctrl Pts',(0.00298921425821311,-0.0334762898220594,
-0.0124341220556221));
#32400=CARTESIAN_POINT('Ctrl Pts',(0.00300674610335933,-0.0334903128407513,
-0.0121872443109676));
#32401=CARTESIAN_POINT('Ctrl Pts',(0.0030007171964696,-0.033502352356114,
-0.0119852056927177));
#32402=CARTESIAN_POINT('Ctrl Pts',(0.00296081193949715,-0.0335202244195151,
-0.011681283651093));
#32403=CARTESIAN_POINT('Ctrl Pts',(0.00294170641447226,-0.0335262604735305,
-0.0115780467182088));
#32404=CARTESIAN_POINT('Ctrl Pts',(0.00290112723839275,-0.0335360270841346,
-0.0114088947946929));
#32405=CARTESIAN_POINT('Ctrl Pts',(0.0028827124027571,-0.0335398378952589,
-0.0113423457405591));
#32406=CARTESIAN_POINT('Ctrl Pts',(0.00285363918138549,-0.0335450908644545,
-0.0112498271658951));
#32407=CARTESIAN_POINT('Ctrl Pts',(0.00284488913388691,-0.0335465926810205,
-0.0112232847372945));
#32408=CARTESIAN_POINT('Ctrl Pts',(0.00282914100414081,-0.0335491654528002,
-0.0111776680614974));
#32409=CARTESIAN_POINT('Ctrl Pts',(0.00282231779646004,-0.0335502419624426,
-0.0111585358101415));
#32410=CARTESIAN_POINT('Ctrl Pts',(0.00280881402419867,-0.0335523015193921,
-0.0111218531205161));
#32411=CARTESIAN_POINT('Ctrl Pts',(0.00280216197203806,-0.0335532854343438,
-0.011104293266727));
#32412=CARTESIAN_POINT('Ctrl Pts',(0.0027841343290008,-0.0335558735425907,
-0.0110580206559875));
#32413=CARTESIAN_POINT('Ctrl Pts',(0.00277247933953992,-0.0335574685142712,
-0.011029418746871));
#32414=CARTESIAN_POINT('Ctrl Pts',(0.00272736382179645,-0.0335633667010298,
-0.0109234171679631));
#32415=CARTESIAN_POINT('Ctrl Pts',(0.00269108552334449,-0.0335675770946644,
-0.0108472563310091));
#32416=CARTESIAN_POINT('Ctrl Pts',(0.00253966399166702,-0.0335834446059485,
-0.0105610994439099));
#32417=CARTESIAN_POINT('Ctrl Pts',(0.00240276269478221,-0.0335944255477463,
-0.0103636596378104));
#32418=CARTESIAN_POINT('Ctrl Pts',(0.0022060431227533,-0.0336088396303959,
-0.0101419851959459));
#32419=CARTESIAN_POINT('Ctrl Pts',(0.0021670241508855,-0.0336116489773119,
-0.0101004614159256));
#32420=CARTESIAN_POINT('Ctrl Pts',(0.00210013203456061,-0.0336164329165445,
-0.0100332192825171));
#32421=CARTESIAN_POINT('Ctrl Pts',(0.00207291032358271,-0.0336183714553603,
-0.0100068725162208));
#32422=CARTESIAN_POINT('Ctrl Pts',(0.00203378756486346,-0.033621158348103,
-0.0099704165036299));
#32423=CARTESIAN_POINT('Ctrl Pts',(0.00202229436459781,-0.0336219771625735,
-0.0099598729741601));
#32424=CARTESIAN_POINT('Ctrl Pts',(0.00200232348771699,-0.033623401188328,
-0.00994183702763557));
#32425=CARTESIAN_POINT('Ctrl Pts',(0.00199388458581984,-0.0336240033210849,
-0.00993430198201933));
#32426=CARTESIAN_POINT('Ctrl Pts',(0.00197577171573472,-0.0336252968914373,
-0.00991831232699575));
#32427=CARTESIAN_POINT('Ctrl Pts',(0.00196608590752573,-0.0336259892557443,
-0.00990987198721579));
#32428=CARTESIAN_POINT('Ctrl Pts',(0.00193930637832258,-0.0336279045058861,
-0.00988683691036074));
#32429=CARTESIAN_POINT('Ctrl Pts',(0.00192210269609774,-0.0336291359892139,
-0.00987237192864144));
#32430=CARTESIAN_POINT('Ctrl Pts',(0.00180433424706328,-0.0336375638991048,
-0.00977558927594874));
#32431=CARTESIAN_POINT('Ctrl Pts',(0.00169868243732296,-0.0336451082024506,
-0.00969969465232878));
#32432=CARTESIAN_POINT('Ctrl Pts',(0.00143670790868342,-0.0336632129203722,
-0.00953618132325929));
#32433=CARTESIAN_POINT('Ctrl Pts',(0.00127678122121681,-0.0336737864989685,
-0.00945522166658635));
#32434=CARTESIAN_POINT('Ctrl Pts',(0.00105170143166814,-0.0336875887114654,
-0.00936552548481514));
#32435=CARTESIAN_POINT('Ctrl Pts',(0.000992083855422767,-0.0336911516953911,
-0.00934393015321076));
#32436=CARTESIAN_POINT('Ctrl Pts',(0.000886003690370446,-0.0336973235974966,
-0.00930926626875169));
#32437=CARTESIAN_POINT('Ctrl Pts',(0.000839827654198565,-0.0336999557687732,
-0.00929539958195612));
#32438=CARTESIAN_POINT('Ctrl Pts',(0.000769789795029305,-0.03370386807312,
-0.00927619472699345));
#32439=CARTESIAN_POINT('Ctrl Pts',(0.000746165595508288,-0.0337051742124621,
-0.00927002585839427));
#32440=CARTESIAN_POINT('Ctrl Pts',(0.000703177438411757,-0.0337075271116816,
-0.00925935940932528));
#32441=CARTESIAN_POINT('Ctrl Pts',(0.000683839249905239,-0.0337085768828414,
-0.00925476462794435));
#32442=CARTESIAN_POINT('Ctrl Pts',(0.000641900235454159,-0.0337108353247436,
-0.00924523916667989));
#32443=CARTESIAN_POINT('Ctrl Pts',(0.00061928507236787,-0.0337120417901303,
-0.00924037699300135));
#32444=CARTESIAN_POINT('Ctrl Pts',(0.00055680987881161,-0.0337153447562834,
-0.00922769920398575));
#32445=CARTESIAN_POINT('Ctrl Pts',(0.000516843203733572,-0.0337174242612458,
-0.00922043063716578));
#32446=CARTESIAN_POINT('Ctrl Pts',(0.000241871781243092,-0.0337315262754025,
-0.00917617159201931));
#32447=CARTESIAN_POINT('Ctrl Pts',(3.34695343856238E-6,-0.0337426496684483,
-0.00916643671368752));
#32448=CARTESIAN_POINT('Ctrl Pts',(-0.000333825716125148,-0.0337587366901328,
-0.00919279787667365));
#32449=CARTESIAN_POINT('Ctrl Pts',(-0.000433356153499485,-0.0337635446163017,
-0.00920562441907331));
#32450=CARTESIAN_POINT('Ctrl Pts',(-0.000586446892030909,-0.0337712629618868,
-0.00923321246590553));
#32451=CARTESIAN_POINT('Ctrl Pts',(-0.000640558066760292,-0.0337740552886763,
-0.00924451577164478));
#32452=CARTESIAN_POINT('Ctrl Pts',(-0.000711769609780924,-0.0337778511464565,
-0.00926145701357161));
#32453=CARTESIAN_POINT('Ctrl Pts',(-0.000729178299210887,-0.0337787887940389,
-0.00926576383929829));
#32454=CARTESIAN_POINT('Ctrl Pts',(-0.000757912779704372,-0.0337803540745094,
-0.00927314663084856));
#32455=CARTESIAN_POINT('Ctrl Pts',(-0.000769261276142269,-0.0337809768430059,
-0.00927613350812632));
#32456=CARTESIAN_POINT('Ctrl Pts',(-0.000790773216982359,-0.0337821665316029,
-0.00928193053228682));
#32457=CARTESIAN_POINT('Ctrl Pts',(-0.00080093991319622,-0.0337827326834863,
-0.00928472782455402));
#32458=CARTESIAN_POINT('Ctrl Pts',(-0.000828213949647178,-0.0337842615729003,
-0.00929238697802385));
#32459=CARTESIAN_POINT('Ctrl Pts',(-0.000845292902179561,-0.0337852296521758,
-0.00929734739321175));
#32460=CARTESIAN_POINT('Ctrl Pts',(-0.000909809334555627,-0.0337889245323163,
-0.00931670924097599));
#32461=CARTESIAN_POINT('Ctrl Pts',(-0.00095692933637723,-0.0337917010404217,
-0.00933213329153598));
#32462=CARTESIAN_POINT('Ctrl Pts',(-0.0011913284390104,-0.0338058334777848,
-0.00941534575192511));
#32463=CARTESIAN_POINT('Ctrl Pts',(-0.00137190836009119,-0.0338177236633955,
-0.00950049690718562));
#32464=CARTESIAN_POINT('Ctrl Pts',(-0.00163142865392247,-0.0338353566708339,
-0.00965610335911827));
#32465=CARTESIAN_POINT('Ctrl Pts',(-0.00171733566480339,-0.0338413037589557,
-0.0097138500123255));
#32466=CARTESIAN_POINT('Ctrl Pts',(-0.00185479268939082,-0.0338509470172707,
-0.00981695112819509));
#32467=CARTESIAN_POINT('Ctrl Pts',(-0.00190807610539897,-0.0338547208060546,
-0.00985983905829571));
#32468=CARTESIAN_POINT('Ctrl Pts',(-0.00198093519528966,-0.0338599326517222,
-0.00992270630495153));
#32469=CARTESIAN_POINT('Ctrl Pts',(-0.00200176617419573,-0.0338614291184264,
-0.00994119272548116));
#32470=CARTESIAN_POINT('Ctrl Pts',(-0.00203732798046824,-0.033863995664781,
-0.00997364834525282));
#32471=CARTESIAN_POINT('Ctrl Pts',(-0.00205217976855487,-0.0338650712272053,
-0.00998748171660667));
#32472=CARTESIAN_POINT('Ctrl Pts',(-0.00208051597644032,-0.033867130956198,
-0.0100144170309272));
#32473=CARTESIAN_POINT('Ctrl Pts',(-0.00209401981935827,-0.0338681159673373,
-0.0100274970701287));
#32474=CARTESIAN_POINT('Ctrl Pts',(-0.00212946847877434,-0.0338707115076103,
-0.0100624850143133));
#32475=CARTESIAN_POINT('Ctrl Pts',(-0.00215119840209031,-0.0338723127110495,
-0.0100846079680464));
#32476=CARTESIAN_POINT('Ctrl Pts',(-0.00223145296532613,-0.0338782701821735,
-0.0101688889773073));
#32477=CARTESIAN_POINT('Ctrl Pts',(-0.00228766076905602,-0.0338825310445765,
-0.0102332010149176));
#32478=CARTESIAN_POINT('Ctrl Pts',(-0.00249003748671433,-0.033898383086564,
-0.0104857424734329));
#32479=CARTESIAN_POINT('Ctrl Pts',(-0.00261633580989301,-0.0339093124469644,
-0.0106887287250801));
#32480=CARTESIAN_POINT('Ctrl Pts',(-0.00274139680927863,-0.0339236659461116,
-0.0109560259422959));
#32481=CARTESIAN_POINT('Ctrl Pts',(-0.00276402999804866,-0.0339264709775133,
-0.0110082177245521));
#32482=CARTESIAN_POINT('Ctrl Pts',(-0.00279922615419709,-0.0339312483159769,
-0.0110961474561313));
#32483=CARTESIAN_POINT('Ctrl Pts',(-0.0028126208690476,-0.0339331846975033,
-0.0111315375564136));
#32484=CARTESIAN_POINT('Ctrl Pts',(-0.00283058386373906,-0.0339359690065269,
-0.0111818522620625));
#32485=CARTESIAN_POINT('Ctrl Pts',(-0.0028357109981554,-0.0339367874682492,
-0.0111965748987347));
#32486=CARTESIAN_POINT('Ctrl Pts',(-0.00284436007607873,-0.0339382110910635,
-0.0112220484163447));
#32487=CARTESIAN_POINT('Ctrl Pts',(-0.00284793642681659,-0.033938813178737,
-0.0112327806067025));
#32488=CARTESIAN_POINT('Ctrl Pts',(-0.00285544579098707,-0.0339401069030581,
-0.011255747594637));
#32489=CARTESIAN_POINT('Ctrl Pts',(-0.0028593609577176,-0.0339407994694376,
-0.0112679876296553));
#32490=CARTESIAN_POINT('Ctrl Pts',(-0.00286991213315692,-0.0339427158115958,
-0.011301719274122));
#32491=CARTESIAN_POINT('Ctrl Pts',(-0.00287638514432946,-0.0339439482001548,
-0.0113232605548196));
#32492=CARTESIAN_POINT('Ctrl Pts',(-0.00291998431332457,-0.0339526509141746,
-0.0114745029682231));
#32493=CARTESIAN_POINT('Ctrl Pts',(-0.00294856360960901,-0.0339604960759037,
-0.0116064965794291));
#32494=CARTESIAN_POINT('Ctrl Pts',(-0.00299285361193743,-0.0339783784021183,
-0.0119080783278752));
#32495=CARTESIAN_POINT('Ctrl Pts',(-0.00300321674425717,-0.0339884119842963,
-0.0120780118217047));
#32496=CARTESIAN_POINT('Ctrl Pts',(-0.00299756163315046,-0.0340018445421147,
-0.0123133716365926));
#32497=CARTESIAN_POINT('Ctrl Pts',(-0.00299384633835027,-0.0340055299811987,
-0.0123787620566068));
#32498=CARTESIAN_POINT('Ctrl Pts',(-0.00298358001203221,-0.0340118886751861,
-0.0124931688365766));
#32499=CARTESIAN_POINT('Ctrl Pts',(-0.00297795217245256,-0.0340145872062452,
-0.0125422411890859));
#32500=CARTESIAN_POINT('Ctrl Pts',(-0.00296770404967998,-0.0340185768175463,
-0.0126155575365401));
#32501=CARTESIAN_POINT('Ctrl Pts',(-0.00296399238586176,-0.0340198954622457,
-0.0126399183029434));
#32502=CARTESIAN_POINT('Ctrl Pts',(-0.00295674317914521,-0.0340222616794114,
-0.0126838546037975));
#32503=CARTESIAN_POINT('Ctrl Pts',(-0.00295331030968823,-0.0340233124237095,
-0.0127034457484575));
#32504=CARTESIAN_POINT('Ctrl Pts',(-0.00294549598158082,-0.0340255629870533,
-0.0127455728784517));
#32505=CARTESIAN_POINT('Ctrl Pts',(-0.00294105014067019,-0.0340267607318689,
-0.0127680957192668));
#32506=CARTESIAN_POINT('Ctrl Pts',(-0.0029281874507338,-0.0340300144000641,
-0.0128295379599495));
#32507=CARTESIAN_POINT('Ctrl Pts',(-0.00291925347711313,-0.0340320541772108,
-0.0128683449632596));
#32508=CARTESIAN_POINT('Ctrl Pts',(-0.00285012500560406,-0.0340464281526899,
-0.0131434506976239));
#32509=CARTESIAN_POINT('Ctrl Pts',(-0.002762094528966,-0.0340578070819802,
-0.0133718038516003));
#32510=CARTESIAN_POINT('Ctrl Pts',(-0.00260169779295154,-0.0340740405498672,
-0.0136727183546661));
#32511=CARTESIAN_POINT('Ctrl Pts',(-0.00255186997835265,-0.0340787050510572,
-0.0137561678377765));
#32512=CARTESIAN_POINT('Ctrl Pts',(-0.00246807827385146,-0.0340862200455918,
-0.0138821727938511));
#32513=CARTESIAN_POINT('Ctrl Pts',(-0.00243685568229249,-0.0340889597593756,
-0.0139264732776887));
#32514=CARTESIAN_POINT('Ctrl Pts',(-0.00239380159778495,-0.0340926940815064,
-0.0139841760222617));
#32515=CARTESIAN_POINT('Ctrl Pts',(-0.00238302410811179,-0.034093625465097,
-0.0139983552142524));
#32516=CARTESIAN_POINT('Ctrl Pts',(-0.00236495278188501,-0.03409518310916,
-0.0140216960348236));
#32517=CARTESIAN_POINT('Ctrl Pts',(-0.00235773023633278,-0.0340958046034524,
-0.0140309126491647));
#32518=CARTESIAN_POINT('Ctrl Pts',(-0.00234388749453897,-0.0340969942700964,
-0.0140483657900979));
#32519=CARTESIAN_POINT('Ctrl Pts',(-0.00233727740221758,-0.0340975617001701,
-0.0140566100494666));
#32520=CARTESIAN_POINT('Ctrl Pts',(-0.00231934997860591,-0.0340990984959883,
-0.0140787290754456));
#32521=CARTESIAN_POINT('Ctrl Pts',(-0.00230795192820077,-0.0341000732985576,
-0.0140925375217369));
#32522=CARTESIAN_POINT('Ctrl Pts',(-0.00226395465425984,-0.034103824766328,
-0.0141448775882746));
#32523=CARTESIAN_POINT('Ctrl Pts',(-0.00223050998484804,-0.034106653025306,
-0.0141826846258763));
#32524=CARTESIAN_POINT('Ctrl Pts',(-0.00206084248745236,-0.034120812824986,
-0.0143650001362215));
#32525=CARTESIAN_POINT('Ctrl Pts',(-0.00191145882869984,-0.034132667946825,
-0.0144965773114821));
#32526=CARTESIAN_POINT('Ctrl Pts',(-0.00166645299184769,-0.0341502440525831,
-0.0146725630220531));
#32527=CARTESIAN_POINT('Ctrl Pts',(-0.00157968542853716,-0.0341561695176447,
-0.0147283465301897));
#32528=CARTESIAN_POINT('Ctrl Pts',(-0.00143100652823459,-0.0341657827333614,
-0.0148134419433172));
#32529=CARTESIAN_POINT('Ctrl Pts',(-0.0013706592051858,-0.03416954746851,
-0.0148453004125789));
#32530=CARTESIAN_POINT('Ctrl Pts',(-0.00128423907191374,-0.0341747492485911,
-0.0148872190408566));
#32531=CARTESIAN_POINT('Ctrl Pts',(-0.00125903523533144,-0.0341762443998648,
-0.0148990140592912));
#32532=CARTESIAN_POINT('Ctrl Pts',(-0.001215174019169,-0.0341788094166759,
-0.0149188013074119));
#32533=CARTESIAN_POINT('Ctrl Pts',(-0.00119659320688423,-0.034179884747394,
-0.0149269578767765));
#32534=CARTESIAN_POINT('Ctrl Pts',(-0.00116063602620518,-0.0341819445240121,
-0.0149423090770054));
#32535=CARTESIAN_POINT('Ctrl Pts',(-0.00114327200410095,-0.0341829298087768,
-0.0149495300470402));
#32536=CARTESIAN_POINT('Ctrl Pts',(-0.00109707117346208,-0.0341855271998249,
-0.014968235462984));
#32537=CARTESIAN_POINT('Ctrl Pts',(-0.00106812170071878,-0.0341871299544445,
-0.014979436619136));
#32538=CARTESIAN_POINT('Ctrl Pts',(-0.000958664249872616,-0.0341931025270523,
-0.0150198464034051));
#32539=CARTESIAN_POINT('Ctrl Pts',(-0.000877088902219408,-0.0341973762735131,
-0.0150460537379515));
#32540=CARTESIAN_POINT('Ctrl Pts',(-0.000565047458946579,-0.0342132244841497,
-0.0151317525531442));
#32541=CARTESIAN_POINT('Ctrl Pts',(-0.000328931019634678,-0.0342241407562824,
-0.0151672433965715));
#32542=CARTESIAN_POINT('Ctrl Pts',(-3.42820793670757E-5,-0.0342384788764484,
-0.0151761961482578));
#32543=CARTESIAN_POINT('Ctrl Pts',(2.25823401362681E-5,-0.0342412828056937,
-0.0151763069201371));
#32544=CARTESIAN_POINT('Ctrl Pts',(0.000117226831195046,-0.034246058458155,
-0.0151738007129355));
#32545=CARTESIAN_POINT('Ctrl Pts',(0.000155016910013541,-0.0342479942884883,
-0.0151720843213275));
#32546=CARTESIAN_POINT('Ctrl Pts',(0.000208318725397031,-0.0342507779373783,
-0.0151686523609703));
#32547=CARTESIAN_POINT('Ctrl Pts',(0.000223866317502566,-0.0342515963089763,
-0.0151675295462171));
#32548=CARTESIAN_POINT('Ctrl Pts',(0.000250680309804121,-0.0342530198289133,
-0.015165382906679));
#32549=CARTESIAN_POINT('Ctrl Pts',(0.000261951093202847,-0.03425362190514,
-0.0151644164178833));
#32550=CARTESIAN_POINT('Ctrl Pts',(0.000286014821568249,-0.0342549156690621,
-0.0151622157386412));
#32551=CARTESIAN_POINT('Ctrl Pts',(0.000298805506103946,-0.0342556082872627,
-0.0151609630719462));
#32552=CARTESIAN_POINT('Ctrl Pts',(0.000333962716912195,-0.0342575249093787,
-0.015157291700008));
#32553=CARTESIAN_POINT('Ctrl Pts',(0.000356310289424819,-0.0342587575299941,
-0.0151547035728422));
#32554=CARTESIAN_POINT('Ctrl Pts',(0.000513576010346341,-0.0342675228920418,
-0.0151346952853522));
#32555=CARTESIAN_POINT('Ctrl Pts',(0.00064719097540904,-0.0342754367332917,
-0.0151083682128113));
#32556=CARTESIAN_POINT('Ctrl Pts',(0.000946840011479498,-0.0342936420926783,
-0.0150278459720689));
#32557=CARTESIAN_POINT('Ctrl Pts',(0.00111088790677592,-0.0343039287943268,
-0.014968039696976));
#32558=CARTESIAN_POINT('Ctrl Pts',(0.00132555183636874,-0.0343174151433276,
-0.0148678472916823));
#32559=CARTESIAN_POINT('Ctrl Pts',(0.00138144153916055,-0.0343209321186503,
-0.0148395986568057));
#32560=CARTESIAN_POINT('Ctrl Pts',(0.00147833552793655,-0.0343270335771446,
-0.0147867544238806));
#32561=CARTESIAN_POINT('Ctrl Pts',(0.00151971153156067,-0.0343296405749895,
-0.0147628897950129));
#32562=CARTESIAN_POINT('Ctrl Pts',(0.00158127995482397,-0.0343335234940839,
-0.014725391594343));
#32563=CARTESIAN_POINT('Ctrl Pts',(0.00160190379290108,-0.0343348248410766,
-0.0147124841552056));
#32564=CARTESIAN_POINT('Ctrl Pts',(0.00163908390228504,-0.0343371726784623,
-0.0146885806576091));
#32565=CARTESIAN_POINT('Ctrl Pts',(0.00165569211696096,-0.03433822211851,
-0.0146776683315079));
#32566=CARTESIAN_POINT('Ctrl Pts',(0.00169145340477964,-0.0343404837883751,
-0.014653659505954));
#32567=CARTESIAN_POINT('Ctrl Pts',(0.00171056552600858,-0.0343416937605292,
-0.0146405041547294));
#32568=CARTESIAN_POINT('Ctrl Pts',(0.00176297504096698,-0.0343450166098808,
-0.0146035260553021));
#32569=CARTESIAN_POINT('Ctrl Pts',(0.00179594090345443,-0.0343471121430334,
-0.0145792410083115));
#32570=CARTESIAN_POINT('Ctrl Pts',(0.002015006397015,-0.0343610985681317,
-0.0144108363731809));
#32571=CARTESIAN_POINT('Ctrl Pts',(0.00218407892212733,-0.0343721134321571,
-0.014245927362271));
#32572=CARTESIAN_POINT('Ctrl Pts',(0.00239609404274169,-0.0343881404002779,
-0.0139839099219335));
#32573=CARTESIAN_POINT('Ctrl Pts',(0.00245598149570972,-0.0343930104480621,
-0.0139016829958145));
#32574=CARTESIAN_POINT('Ctrl Pts',(0.00254205699614042,-0.0344008165638233,
-0.0137699211504468));
#32575=CARTESIAN_POINT('Ctrl Pts',(0.00257122983607939,-0.0344036313082395,
-0.0137224245093847));
#32576=CARTESIAN_POINT('Ctrl Pts',(0.00260804371731996,-0.0344074533653778,
-0.0136585641292623));
#32577=CARTESIAN_POINT('Ctrl Pts',(0.00261688566483034,-0.0344083936449175,
-0.0136429023181759));
#32578=CARTESIAN_POINT('Ctrl Pts',(0.00263126831706156,-0.0344099621380394,
-0.0136168824354636));
#32579=CARTESIAN_POINT('Ctrl Pts',(0.00263689009826553,-0.0344105854458042,
-0.0136065693895787));
#32580=CARTESIAN_POINT('Ctrl Pts',(0.00264743917073649,-0.0344117751624809,
-0.0135869439400167));
#32581=CARTESIAN_POINT('Ctrl Pts',(0.00265237824260972,-0.0344123407924217,
-0.0135776380940047));
#32582=CARTESIAN_POINT('Ctrl Pts',(0.00266550002957876,-0.0344138664384547,
-0.0135525973212715));
#32583=CARTESIAN_POINT('Ctrl Pts',(0.00267359227826778,-0.0344148317573992,
-0.0135368157563903));
#32584=CARTESIAN_POINT('Ctrl Pts',(0.00270360905272258,-0.0344185036667659,
-0.0134769758389944));
#32585=CARTESIAN_POINT('Ctrl Pts',(0.00272458732103992,-0.0344212592091826,
-0.0134324539443992));
#32586=CARTESIAN_POINT('Ctrl Pts',(0.00284647516087281,-0.0344384026480205,
-0.0131563559827071));
#32587=CARTESIAN_POINT('Ctrl Pts',(0.00291889953234112,-0.034453623836841,
-0.0129133122837938));
#32588=CARTESIAN_POINT('Ctrl Pts',(0.00297765692132849,-0.0344743274315713,
-0.0125570596108822));
#32589=CARTESIAN_POINT('Ctrl Pts',(0.00298949077105853,-0.0344804115792897,
-0.0124491805486363));
#32590=CARTESIAN_POINT('Ctrl Pts',(0.00299724546138588,-0.0344880908989193,
-0.0123084293409625));
#32591=CARTESIAN_POINT('Ctrl Pts',(0.00299850611955335,-0.0344898458974053,
-0.0122759428935426));
#32592=CARTESIAN_POINT('Ctrl Pts',(0.00299971598216001,-0.0344927183440224,
-0.0122222550161421));
#32593=CARTESIAN_POINT('Ctrl Pts',(0.00299996892616627,-0.0344938449683844,
-0.0122010637404368));
#32594=CARTESIAN_POINT('Ctrl Pts',(0.00300002461319226,-0.0344960419371712,
-0.0121594846018045));
#32595=CARTESIAN_POINT('Ctrl Pts',(0.00299984411022637,-0.0344971127343431,
-0.0121390979436702));
#32596=CARTESIAN_POINT('Ctrl Pts',(0.00299891529576274,-0.0344996590735799,
-0.0120903406682142));
#32597=CARTESIAN_POINT('Ctrl Pts',(0.00299797219369084,-0.0345011285952758,
-0.0120619754773406));
#32598=CARTESIAN_POINT('Ctrl Pts',(0.00299321271817669,-0.0345062854345003,
-0.0119616958334017));
#32599=CARTESIAN_POINT('Ctrl Pts',(0.00298720971645073,-0.0345099065214422,
-0.0118899076669784));
#32600=CARTESIAN_POINT('Ctrl Pts',(0.00296529790018503,-0.0345189959594432,
-0.0117073176237771));
#32601=CARTESIAN_POINT('Ctrl Pts',(0.00294576314498241,-0.0345243675747273,
-0.0115970624596732));
#32602=CARTESIAN_POINT('Ctrl Pts',(0.00288173866082887,-0.0345376533955076,
-0.0113252019220437));
#32603=CARTESIAN_POINT('Ctrl Pts',(0.00282979326742278,-0.0345454756227368,
-0.0111657595648701));
#32604=CARTESIAN_POINT('Ctrl Pts',(0.00273982593493822,-0.0345568871223864,
-0.0109521282819776));
#32605=CARTESIAN_POINT('Ctrl Pts',(0.00271292201820517,-0.0345601190442526,
-0.0108935888341284));
#32606=CARTESIAN_POINT('Ctrl Pts',(0.00267545318480082,-0.0345644567784832,
-0.0108185287065842));
#32607=CARTESIAN_POINT('Ctrl Pts',(0.00266658006343966,-0.0345654732865576,
-0.0108011786027092));
#32608=CARTESIAN_POINT('Ctrl Pts',(0.00265193889398139,-0.0345671354871448,
-0.0107732251215521));
#32609=CARTESIAN_POINT('Ctrl Pts',(0.00264627464727293,-0.0345677750349074,
-0.0107625677004703));
#32610=CARTESIAN_POINT('Ctrl Pts',(0.0026350039720529,-0.0345690413360245,
-0.0107416669590874));
#32611=CARTESIAN_POINT('Ctrl Pts',(0.00262940177935275,-0.0345696678410616,
-0.0107314216945453));
#32612=CARTESIAN_POINT('Ctrl Pts',(0.00261518123589728,-0.0345712504016995,
-0.0107057721071383));
#32613=CARTESIAN_POINT('Ctrl Pts',(0.00260648654243604,-0.0345722110228962,
-0.0106904107783884));
#32614=CARTESIAN_POINT('Ctrl Pts',(0.00257122949402419,-0.0345760761453026,
-0.0106293831634086));
#32615=CARTESIAN_POINT('Ctrl Pts',(0.00254359972078884,-0.0345790382761807,
-0.0105843474669341));
#32616=CARTESIAN_POINT('Ctrl Pts',(0.0024639394286114,-0.0345873529935348,
-0.0104618806600705));
#32617=CARTESIAN_POINT('Ctrl Pts',(0.00240946536699408,-0.0345927937015789,
-0.0103861117755327));
#32618=CARTESIAN_POINT('Ctrl Pts',(0.00220654767787301,-0.0346119681278612,
-0.0101299597176363));
#32619=CARTESIAN_POINT('Ctrl Pts',(0.00204064041593849,-0.0346257273955933,
-0.009964439755018));
#32620=CARTESIAN_POINT('Ctrl Pts',(0.00181808388552439,-0.0346414203239254,
-0.00978900365582104));
#32621=CARTESIAN_POINT('Ctrl Pts',(0.00177820983410336,-0.0346441422964082,
-0.00975915091342264));
#32622=CARTESIAN_POINT('Ctrl Pts',(0.00171745851345907,-0.0346481591624086,
-0.00971598595232774));
#32623=CARTESIAN_POINT('Ctrl Pts',(0.00169713111366653,-0.0346494821804487,
-0.00970191774174177));
#32624=CARTESIAN_POINT('Ctrl Pts',(0.00166013453096633,-0.0346518530905548,
-0.00967698371915239));
#32625=CARTESIAN_POINT('Ctrl Pts',(0.00164352688581077,-0.0346529042105308,
-0.00966602955233309));
#32626=CARTESIAN_POINT('Ctrl Pts',(0.00160757221629099,-0.0346551521949152,
-0.00964282429162535));
#32627=CARTESIAN_POINT('Ctrl Pts',(0.00158819133633765,-0.0346563470292288,
-0.00963062782762439));
#32628=CARTESIAN_POINT('Ctrl Pts',(0.00153403817337389,-0.0346596402926559,
-0.00959740844662663));
#32629=CARTESIAN_POINT('Ctrl Pts',(0.00149897498055441,-0.0346617215321998,
-0.00957686788523866));
#32630=CARTESIAN_POINT('Ctrl Pts',(0.00134975892204702,-0.0346703805985349,
-0.00949347943719754));
#32631=CARTESIAN_POINT('Ctrl Pts',(0.00123198693284768,-0.0346767289236711,
-0.00943738819676805));
#32632=CARTESIAN_POINT('Ctrl Pts',(0.00102720088399999,-0.0346872818427046,
-0.00935574979752547));
#32633=CARTESIAN_POINT('Ctrl Pts',(0.000942005841697467,-0.0346915407991256,
-0.00932616021978938));
#32634=CARTESIAN_POINT('Ctrl Pts',(0.000708750964245328,-0.0347030886555901,
-0.0092567526449807));
#32635=CARTESIAN_POINT('Ctrl Pts',(0.000558775451297078,-0.0347103902258542,
-0.00922437269920118));
#32636=CARTESIAN_POINT('Ctrl Pts',(0.000377694610717754,-0.0347196991481665,
-0.00919957680386364));
#32637=CARTESIAN_POINT('Ctrl Pts',(0.000348332311057776,-0.0347212240978858,
-0.00919599768639593));
#32638=CARTESIAN_POINT('Ctrl Pts',(0.000304848400077032,-0.0347235115019578,
-0.00919134866932447));
#32639=CARTESIAN_POINT('Ctrl Pts',(0.000290763648035617,-0.0347242569003196,
-0.0091899435687827));
#32640=CARTESIAN_POINT('Ctrl Pts',(0.000265531238535391,-0.0347256011157826,
-0.00918760659456845));
#32641=CARTESIAN_POINT('Ctrl Pts',(0.000254387584534166,-0.0347261979114213,
-0.00918663732241465));
#32642=CARTESIAN_POINT('Ctrl Pts',(0.000229431710881271,-0.0347275415210618,
-0.00918460722840893));
#32643=CARTESIAN_POINT('Ctrl Pts',(0.000215617521548614,-0.0347282900522575,
-0.00918357974293981));
#32644=CARTESIAN_POINT('Ctrl Pts',(0.000173855539317694,-0.0347305663830886,
-0.00918076421870998));
#32645=CARTESIAN_POINT('Ctrl Pts',(0.000145890049198672,-0.0347321088562114,
-0.00917927185825855));
#32646=CARTESIAN_POINT('Ctrl Pts',(6.24895452250378E-6,-0.0347398879023014,
-0.00917377931081361));
#32647=CARTESIAN_POINT('Ctrl Pts',(-0.000105561046078815,-0.0347463590294455,
-0.00917562991509687));
#32648=CARTESIAN_POINT('Ctrl Pts',(-0.000475559634842973,-0.0347680737263861,
-0.00920246313494406));
#32649=CARTESIAN_POINT('Ctrl Pts',(-0.000730653026213323,-0.0347834157303929,
-0.00925465585206034));
#32650=CARTESIAN_POINT('Ctrl Pts',(-0.00101312983671242,-0.0347998730326235,
-0.00935182773343107));
#32651=CARTESIAN_POINT('Ctrl Pts',(-0.00105013240568794,-0.0348020209309889,
-0.00936537743360993));
#32652=CARTESIAN_POINT('Ctrl Pts',(-0.00111006271315644,-0.0348054876307774,
-0.00938867181549161));
#32653=CARTESIAN_POINT('Ctrl Pts',(-0.00113315415373076,-0.0348068204060212,
-0.00939797973037137));
#32654=CARTESIAN_POINT('Ctrl Pts',(-0.00117449703184685,-0.034809201847736,
-0.0094152459229905));
#32655=CARTESIAN_POINT('Ctrl Pts',(-0.00119278999264321,-0.034810253867157,
-0.00942310041850815));
#32656=CARTESIAN_POINT('Ctrl Pts',(-0.00123183874922494,-0.0348124964043728,
-0.00944032922346036));
#32657=CARTESIAN_POINT('Ctrl Pts',(-0.00125256879173167,-0.0348136849875685,
-0.00944975899928105));
#32658=CARTESIAN_POINT('Ctrl Pts',(-0.00130943538444792,-0.0348169414264154,
-0.00947641236007226));
#32659=CARTESIAN_POINT('Ctrl Pts',(-0.00134533828458003,-0.0348189927399427,
-0.00949412484542092));
#32660=CARTESIAN_POINT('Ctrl Pts',(-0.00153121340017156,-0.0348296051922691,
-0.00959049794414904));
#32661=CARTESIAN_POINT('Ctrl Pts',(-0.00167468894013557,-0.0348377480243278,
-0.00968103847350597));
#32662=CARTESIAN_POINT('Ctrl Pts',(-0.00195526993133758,-0.0348544604459651,
-0.00989326612709907));
#32663=CARTESIAN_POINT('Ctrl Pts',(-0.00209042051034744,-0.0348629835393922,
-0.0100163588671412));
#32664=CARTESIAN_POINT('Ctrl Pts',(-0.00224403055794431,-0.0348743685349453,
-0.010184279248007));
#32665=CARTESIAN_POINT('Ctrl Pts',(-0.00227376053086639,-0.03487666475848,
-0.0102182902741463));
#32666=CARTESIAN_POINT('Ctrl Pts',(-0.00231370946432668,-0.0348799018090744,
-0.0102661300046118));
#32667=CARTESIAN_POINT('Ctrl Pts',(-0.00232459557282121,-0.0348808001937584,
-0.0102793960908996));
#32668=CARTESIAN_POINT('Ctrl Pts',(-0.00234256336751784,-0.0348823118105403,
-0.010301679253244));
#32669=CARTESIAN_POINT('Ctrl Pts',(-0.0023497084346415,-0.0348829207146633,
-0.0103106450658337));
#32670=CARTESIAN_POINT('Ctrl Pts',(-0.00236433667522902,-0.0348841840047522,
-0.010329218405693));
#32671=CARTESIAN_POINT('Ctrl Pts',(-0.00237181299642614,-0.0348848388036065,
-0.0103388308597318));
#32672=CARTESIAN_POINT('Ctrl Pts',(-0.00239140383310954,-0.0348865783659193,
-0.0103643381437399));
#32673=CARTESIAN_POINT('Ctrl Pts',(-0.00240341820997934,-0.0348876695771154,
-0.0103803087253376));
#32674=CARTESIAN_POINT('Ctrl Pts',(-0.00246119335319745,-0.034893032644773,
-0.0104587274714324));
#32675=CARTESIAN_POINT('Ctrl Pts',(-0.00250468172916291,-0.034897429775811,
-0.0105228071672573));
#32676=CARTESIAN_POINT('Ctrl Pts',(-0.00264612979829027,-0.0349128589598591,
-0.0107496463854092));
#32677=CARTESIAN_POINT('Ctrl Pts',(-0.0027310901716194,-0.0349241816136645,
-0.0109199794702632));
#32678=CARTESIAN_POINT('Ctrl Pts',(-0.00284710874499847,-0.034942869468628,
-0.0112210787534907));
#32679=CARTESIAN_POINT('Ctrl Pts',(-0.00288656839361039,-0.0349503877135219,
-0.0113479931833876));
#32680=CARTESIAN_POINT('Ctrl Pts',(-0.00292569159968663,-0.0349595656926304,
-0.0115113477665344));
#32681=CARTESIAN_POINT('Ctrl Pts',(-0.00293328687454053,-0.0349614703302367,
-0.0115457206204964));
#32682=CARTESIAN_POINT('Ctrl Pts',(-0.00294459517957993,-0.0349645216583975,
-0.0116015427964108));
#32683=CARTESIAN_POINT('Ctrl Pts',(-0.00294868265409088,-0.0349656799091502,
-0.0116229121054753));
#32684=CARTESIAN_POINT('Ctrl Pts',(-0.00295610318756234,-0.034967895696436,
-0.0116641316930658));
#32685=CARTESIAN_POINT('Ctrl Pts',(-0.00295946963592129,-0.0349689542178807,
-0.0116839746989232));
#32686=CARTESIAN_POINT('Ctrl Pts',(-0.00296684851618281,-0.0349714065677787,
-0.0117302899625403));
#32687=CARTESIAN_POINT('Ctrl Pts',(-0.00297070678939083,-0.0349727955649953,
-0.0117567852434946));
#32688=CARTESIAN_POINT('Ctrl Pts',(-0.00298225423626283,-0.0349773394749354,
-0.011844281862726));
#32689=CARTESIAN_POINT('Ctrl Pts',(-0.00298842321182215,-0.0349804480173611,
-0.0119054696907493));
#32690=CARTESIAN_POINT('Ctrl Pts',(-0.00299888051881708,-0.0349879193123658,
-0.012055176314337));
#32691=CARTESIAN_POINT('Ctrl Pts',(-0.00300113642909699,-0.0349922263284735,
-0.0121437792915847));
#32692=CARTESIAN_POINT('Ctrl Pts',(-0.0029972755540795,-0.0350020639478382,
-0.0123487355071376));
#32693=CARTESIAN_POINT('Ctrl Pts',(-0.00298831174534155,-0.0350075441243131,
-0.0124648899098138));
#32694=CARTESIAN_POINT('Ctrl Pts',(-0.00295282137540481,-0.0350200664070991,
-0.0127257845928377));
#32695=CARTESIAN_POINT('Ctrl Pts',(-0.00292235874664381,-0.035027124061726,
-0.012869675384374));
#32696=CARTESIAN_POINT('Ctrl Pts',(-0.00287518126323332,-0.0350358393843081,
-0.0130325014184055));
#32697=CARTESIAN_POINT('Ctrl Pts',(-0.00286862991324815,-0.0350370157495548,
-0.0130541901699344));
#32698=CARTESIAN_POINT('Ctrl Pts',(-0.00285796762736313,-0.035038882049868,
-0.0130880962008863));
#32699=CARTESIAN_POINT('Ctrl Pts',(-0.00285402241401679,-0.0350395630211296,
-0.0131003651264354));
#32700=CARTESIAN_POINT('Ctrl Pts',(-0.0028464688720019,-0.0350408498287807,
-0.0131233461494037));
#32701=CARTESIAN_POINT('Ctrl Pts',(-0.00284287889529581,-0.0350414546464236,
-0.0131340637730616));
#32702=CARTESIAN_POINT('Ctrl Pts',(-0.00283421583975468,-0.0350428981197999,
-0.0131594494742046));
#32703=CARTESIAN_POINT('Ctrl Pts',(-0.00282908938235331,-0.0350437397429562,
-0.0131740988138366));
#32704=CARTESIAN_POINT('Ctrl Pts',(-0.00281122113107034,-0.0350466297114517,
-0.0132239157160189));
#32705=CARTESIAN_POINT('Ctrl Pts',(-0.00279793583624809,-0.0350487059158552,
-0.0132588832549685));
#32706=CARTESIAN_POINT('Ctrl Pts',(-0.00276314855281294,-0.0350539544321809,
-0.0133455294954337));
#32707=CARTESIAN_POINT('Ctrl Pts',(-0.00274084780511743,-0.0350571581687624,
-0.0133968713414091));
#32708=CARTESIAN_POINT('Ctrl Pts',(-0.00262084172779812,-0.0350735378706403,
-0.0136532766472321));
#32709=CARTESIAN_POINT('Ctrl Pts',(-0.00250149268052828,-0.0350871224767957,
-0.0138474215552333));
#32710=CARTESIAN_POINT('Ctrl Pts',(-0.00230244058815474,-0.035105529532247,
-0.0141014434232573));
#32711=CARTESIAN_POINT('Ctrl Pts',(-0.00223994197591191,-0.0351108694527583,
-0.0141738003970405));
#32712=CARTESIAN_POINT('Ctrl Pts',(-0.00215196430840077,-0.035117821671529,
-0.0142663270946311));
#32713=CARTESIAN_POINT('Ctrl Pts',(-0.00212946479547153,-0.0351195546247943,
-0.0142892417790271));
#32714=CARTESIAN_POINT('Ctrl Pts',(-0.00209157116994248,-0.0351224007560056,
-0.0143266149368271));
#32715=CARTESIAN_POINT('Ctrl Pts',(-0.00207638494079759,-0.0351235227751405,
-0.0143412796287501));
#32716=CARTESIAN_POINT('Ctrl Pts',(-0.00204619363440947,-0.0351257176947062,
-0.0143698244192038));
#32717=CARTESIAN_POINT('Ctrl Pts',(-0.00203119901204034,-0.0351267909625586,
-0.014383713862132));
#32718=CARTESIAN_POINT('Ctrl Pts',(-0.00199483328704307,-0.0351293545215655,
-0.0144167151856495));
#32719=CARTESIAN_POINT('Ctrl Pts',(-0.00197332768640488,-0.0351308385725719,
-0.0144356762461259));
#32720=CARTESIAN_POINT('Ctrl Pts',(-0.00189529263666527,-0.0351361142235893,
-0.0145025146618048));
#32721=CARTESIAN_POINT('Ctrl Pts',(-0.00183726433942285,-0.0351398352890842,
-0.0145486044655414));
#32722=CARTESIAN_POINT('Ctrl Pts',(-0.00168342624038712,-0.0351492617776901,
-0.0146617614015495));
#32723=CARTESIAN_POINT('Ctrl Pts',(-0.00158529546913449,-0.0351548601216049,
-0.0147254617843674));
#32724=CARTESIAN_POINT('Ctrl Pts',(-0.00132710590219501,-0.0351689745289846,
-0.0148723786877163));
#32725=CARTESIAN_POINT('Ctrl Pts',(-0.00116282155333357,-0.0351773911406822,
-0.0149471878973429));
#32726=CARTESIAN_POINT('Ctrl Pts',(-0.000947635353302538,-0.0351887696077677,
-0.0150226552664496));
#32727=CARTESIAN_POINT('Ctrl Pts',(-0.000902064935518247,-0.0351911996397882,
-0.0150374215037975));
#32728=CARTESIAN_POINT('Ctrl Pts',(-0.000839339166156025,-0.0351945960922051,
-0.0150560994395986));
#32729=CARTESIAN_POINT('Ctrl Pts',(-0.000822472077934371,-0.0351955144467649,
-0.0150609612204881));
#32730=CARTESIAN_POINT('Ctrl Pts',(-0.000795447385743178,-0.0351969952819539,
-0.0150684945966033));
#32731=CARTESIAN_POINT('Ctrl Pts',(-0.000785316496457693,-0.0351975525183222,
-0.0150712614245921));
#32732=CARTESIAN_POINT('Ctrl Pts',(-0.000763784453527056,-0.0351987417253721,
-0.0150770206806381));
#32733=CARTESIAN_POINT('Ctrl Pts',(-0.000752379845245758,-0.0351993744924799,
-0.0150799992018155));
#32734=CARTESIAN_POINT('Ctrl Pts',(-0.000723339335479696,-0.0352009925808031,
-0.0150874011218788));
#32735=CARTESIAN_POINT('Ctrl Pts',(-0.000705680422636967,-0.0352019828778839,
-0.0150917314905322));
#32736=CARTESIAN_POINT('Ctrl Pts',(-0.000631995950186454,-0.0352061383741216,
-0.0151090920681379));
#32737=CARTESIAN_POINT('Ctrl Pts',(-0.000575643687420339,-0.0352093722179058,
-0.015120669439084));
#32738=CARTESIAN_POINT('Ctrl Pts',(-0.000413507845707785,-0.0352187704930593,
-0.0151491481895211));
#32739=CARTESIAN_POINT('Ctrl Pts',(-0.00030710634564027,-0.0352250488796188,
-0.0151620138722155));
#32740=CARTESIAN_POINT('Ctrl Pts',(2.49417841265192E-5,-0.0352446067499424,
-0.0151842276432674));
#32741=CARTESIAN_POINT('Ctrl Pts',(0.000251149750532565,-0.0352578146674948,
-0.0151738344723821));
#32742=CARTESIAN_POINT('Ctrl Pts',(0.000511947896089953,-0.0352723503420026,
-0.0151320976305147));
#32743=CARTESIAN_POINT('Ctrl Pts',(0.000549704449373298,-0.0352744396976675,
-0.015125310265623));
#32744=CARTESIAN_POINT('Ctrl Pts',(0.000611436566119944,-0.0352778319502788,
-0.0151129862474772));
#32745=CARTESIAN_POINT('Ctrl Pts',(0.000635491811659911,-0.0352791478363707,
-0.0151078756109039));
#32746=CARTESIAN_POINT('Ctrl Pts',(0.00067888125731334,-0.0352815111025249,
-0.0150980982590127));
#32747=CARTESIAN_POINT('Ctrl Pts',(0.000698236873399678,-0.0352825616190308,
-0.0150935339981171));
#32748=CARTESIAN_POINT('Ctrl Pts',(0.000739872340052679,-0.035284813854923,
-0.015083277856986));
#32749=CARTESIAN_POINT('Ctrl Pts',(0.000762135105975031,-0.0352860134717941,
-0.0150775215706431));
#32750=CARTESIAN_POINT('Ctrl Pts',(0.000823994324082737,-0.0352893349892275,
-0.015060766118253));
#32751=CARTESIAN_POINT('Ctrl Pts',(0.000863434917108734,-0.0352914391958564,
-0.015049208301472));
#32752=CARTESIAN_POINT('Ctrl Pts',(0.00102997600453913,-0.0353002815883928,
-0.0149966654928808));
#32753=CARTESIAN_POINT('Ctrl Pts',(0.00115450741646375,-0.0353067779285413,
-0.0149480273707974));
#32754=CARTESIAN_POINT('Ctrl Pts',(0.00135818382546414,-0.0353175380028714,
-0.0148523628690619));
#32755=CARTESIAN_POINT('Ctrl Pts',(0.00143915547467117,-0.0353218570361767,
-0.0148097094986222));
#32756=CARTESIAN_POINT('Ctrl Pts',(0.00164533814460637,-0.0353332064572015,
-0.0146887481524998));
#32757=CARTESIAN_POINT('Ctrl Pts',(0.00176692979934277,-0.035340255689866,
-0.0146047891214333));
#32758=CARTESIAN_POINT('Ctrl Pts',(0.00190500854207849,-0.0353492839001866,
-0.0144935736248103));
#32759=CARTESIAN_POINT('Ctrl Pts',(0.00192789860726415,-0.0353508174483709,
-0.0144745685682159));
#32760=CARTESIAN_POINT('Ctrl Pts',(0.00196128070921921,-0.0353531153268114,
-0.0144460028973862));
#32761=CARTESIAN_POINT('Ctrl Pts',(0.00197199422219986,-0.0353538623749409,
-0.0144367026950361));
#32762=CARTESIAN_POINT('Ctrl Pts',(0.00199103683897563,-0.0353552082656566,
-0.0144199338227507));
#32763=CARTESIAN_POINT('Ctrl Pts',(0.00199939069241221,-0.0353558050623468,
-0.0144124940710782));
#32764=CARTESIAN_POINT('Ctrl Pts',(0.00201797375330345,-0.035357147025304,
-0.014395757111758));
#32765=CARTESIAN_POINT('Ctrl Pts',(0.0020281803463914,-0.0353578938856961,
-0.0143864359088202));
#32766=CARTESIAN_POINT('Ctrl Pts',(0.00205875760081152,-0.0353601600735434,
-0.0143581211111652));
#32767=CARTESIAN_POINT('Ctrl Pts',(0.00207892802349295,-0.035361693891269,
-0.014338914515934));
#32768=CARTESIAN_POINT('Ctrl Pts',(0.00217771454033156,-0.0353693883602091,
-0.0142421902929268));
#32769=CARTESIAN_POINT('Ctrl Pts',(0.00225227201902579,-0.0353757783059338,
-0.0141606596484366));
#32770=CARTESIAN_POINT('Ctrl Pts',(0.00248789499352634,-0.0353975562332824,
-0.0138725865777045));
#32771=CARTESIAN_POINT('Ctrl Pts',(0.0026264282681735,-0.0354130553448458,
-0.0136490958475107));
#32772=CARTESIAN_POINT('Ctrl Pts',(0.00275019798843151,-0.0354296164117932,
-0.0133749880325005));
#32773=CARTESIAN_POINT('Ctrl Pts',(0.00276551539659859,-0.0354317361552911,
-0.0133392267850519));
#32774=CARTESIAN_POINT('Ctrl Pts',(0.00278943361497699,-0.0354351670758613,
-0.0132802411859556));
#32775=CARTESIAN_POINT('Ctrl Pts',(0.00279844975250142,-0.0354364917494667,
-0.0132571911417256));
#32776=CARTESIAN_POINT('Ctrl Pts',(0.00281419771968432,-0.0354388644406584,
-0.0132154142773067));
#32777=CARTESIAN_POINT('Ctrl Pts',(0.00282103035834589,-0.035439915707377,
-0.0131967272267249));
#32778=CARTESIAN_POINT('Ctrl Pts',(0.00283531831039913,-0.0354421627381174,
-0.0131564109877264));
#32779=CARTESIAN_POINT('Ctrl Pts',(0.00284271316972503,-0.035443356488532,
-0.0131347616236971));
#32780=CARTESIAN_POINT('Ctrl Pts',(0.00286252006682121,-0.0354466433586039,
-0.0130745308093722));
#32781=CARTESIAN_POINT('Ctrl Pts',(0.00287439926247934,-0.0354487194019013,
-0.0130357785740234));
#32782=CARTESIAN_POINT('Ctrl Pts',(0.00292094883453316,-0.0354573373929622,
-0.0128721639036939));
#32783=CARTESIAN_POINT('Ctrl Pts',(0.00294829760271707,-0.0354636525531688,
-0.0127453583361953));
#32784=CARTESIAN_POINT('Ctrl Pts',(0.00297920596294723,-0.035473712465473,
-0.0125375358704473));
#32785=CARTESIAN_POINT('Ctrl Pts',(0.00298783942475793,-0.0354775228170552,
-0.0124574527700879));
#32786=CARTESIAN_POINT('Ctrl Pts',(0.003004254943023,-0.0354891250148958,
-0.0122133197283107));
#32787=CARTESIAN_POINT('Ctrl Pts',(0.00300180377856027,-0.0354969119081081,
-0.0120489082021016));
#32788=CARTESIAN_POINT('Ctrl Pts',(0.00298308284062134,-0.0355067683900154,
-0.0118563592865642));
#32789=CARTESIAN_POINT('Ctrl Pts',(0.00297981799026124,-0.0355082803582784,
-0.0118272212824298));
#32790=CARTESIAN_POINT('Ctrl Pts',(0.00297435075122108,-0.0355105519412426,
-0.0117841434736861));
#32791=CARTESIAN_POINT('Ctrl Pts',(0.00297247613896369,-0.0355112948386907,
-0.0117701630640507));
#32792=CARTESIAN_POINT('Ctrl Pts',(0.00296893837442253,-0.0355126365285948,
-0.0117451213040687));
#32793=CARTESIAN_POINT('Ctrl Pts',(0.00296731185787311,-0.035513233336693,
-0.0117340553210341));
#32794=CARTESIAN_POINT('Ctrl Pts',(0.00296352543645847,-0.0355145795042095,
-0.0117092590723368));
#32795=CARTESIAN_POINT('Ctrl Pts',(0.00296133199462682,-0.0355153306163834,
-0.0116955346674882));
#32796=CARTESIAN_POINT('Ctrl Pts',(0.00295439247135007,-0.0355176226675588,
-0.0116539694306518));
#32797=CARTESIAN_POINT('Ctrl Pts',(0.00294934865376934,-0.035519178566197,
-0.011626180620626));
#32798=CARTESIAN_POINT('Ctrl Pts',(0.00292200145941928,-0.0355270902140677,
-0.0114867454820147));
#32799=CARTESIAN_POINT('Ctrl Pts',(0.00289374888780714,-0.0355336888710772,
-0.0113763687435723));
#32800=CARTESIAN_POINT('Ctrl Pts',(0.00279882897120363,-0.0355520547175795,
-0.011077458764045));
#32801=CARTESIAN_POINT('Ctrl Pts',(0.00271948512217469,-0.0355638836750979,
-0.010893539523627));
#32802=CARTESIAN_POINT('Ctrl Pts',(0.00258269460608775,-0.0355798341890619,
-0.0106473291393328));
#32803=CARTESIAN_POINT('Ctrl Pts',(0.00254003605500516,-0.0355843828625148,
-0.0105774428116812));
#32804=CARTESIAN_POINT('Ctrl Pts',(0.0024775887225792,-0.0355904929685943,
-0.0104839642136478));
#32805=CARTESIAN_POINT('Ctrl Pts',(0.00246021955942856,-0.035592140334989,
-0.0104588051433091));
#32806=CARTESIAN_POINT('Ctrl Pts',(0.00243159822569542,-0.0355947735420527,
-0.0104186735745273));
#32807=CARTESIAN_POINT('Ctrl Pts',(0.00242058542714945,-0.0355957682274401,
-0.0104035337096179));
#32808=CARTESIAN_POINT('Ctrl Pts',(0.00239730437013557,-0.0355978332217003,
-0.0103721498533602));
#32809=CARTESIAN_POINT('Ctrl Pts',(0.00238501102549321,-0.0355989025012567,
-0.0103559256085253));
#32810=CARTESIAN_POINT('Ctrl Pts',(0.00235529657326915,-0.0356014380629962,
-0.0103175279340267));
#32811=CARTESIAN_POINT('Ctrl Pts',(0.00233772595529563,-0.0356028984619101,
-0.0102954723434859));
#32812=CARTESIAN_POINT('Ctrl Pts',(0.00227499037939574,-0.0356079820961516,
-0.0102189619968596));
#32813=CARTESIAN_POINT('Ctrl Pts',(0.00222821134265425,-0.0356115416780241,
-0.0101658582847115));
#32814=CARTESIAN_POINT('Ctrl Pts',(0.00210477889758045,-0.0356204276361308,
-0.010035348361344));
#32815=CARTESIAN_POINT('Ctrl Pts',(0.00202570772893042,-0.0356256632065451,
-0.0099603701160623));
#32816=CARTESIAN_POINT('Ctrl Pts',(0.00182080313311095,-0.0356384650704474,
-0.00978623413408031));
#32817=CARTESIAN_POINT('Ctrl Pts',(0.00169078563158549,-0.0356459445899314,
-0.00969254034883679));
#32818=CARTESIAN_POINT('Ctrl Pts',(0.00149007106669639,-0.0356574155936249,
-0.00957100002751177));
#32819=CARTESIAN_POINT('Ctrl Pts',(0.00142480103958752,-0.0356611377085898,
-0.0095347336854759));
#32820=CARTESIAN_POINT('Ctrl Pts',(0.00134002046946372,-0.0356660458469634,
-0.00949168428875245));
#32821=CARTESIAN_POINT('Ctrl Pts',(0.00132169574677134,-0.0356671109668186,
-0.00948261390312541));
#32822=CARTESIAN_POINT('Ctrl Pts',(0.00129222102104624,-0.0356688331712479,
-0.00946839772997434));
#32823=CARTESIAN_POINT('Ctrl Pts',(0.00128112936501425,-0.0356694832719174,
-0.00946313171999589));
#32824=CARTESIAN_POINT('Ctrl Pts',(0.00125955000247898,-0.0356707525567307,
-0.00945304830138889));
#32825=CARTESIAN_POINT('Ctrl Pts',(0.00124906634270593,-0.0356713712775203,
-0.00944822309673462));
#32826=CARTESIAN_POINT('Ctrl Pts',(0.00122310909517892,-0.0356729078963964,
-0.00943645704824017));
#32827=CARTESIAN_POINT('Ctrl Pts',(0.0012076040867256,-0.0356738298338929,
-0.00942958673859811));
#32828=CARTESIAN_POINT('Ctrl Pts',(0.00114865157128265,-0.0356773482285946,
-0.00940406049390908));
#32829=CARTESIAN_POINT('Ctrl Pts',(0.00110482522134812,-0.0356799904646111,
-0.00938630198301244));
#32830=CARTESIAN_POINT('Ctrl Pts',(0.000987090500063967,-0.0356871247529926,
-0.00934180532661316));
#32831=CARTESIAN_POINT('Ctrl Pts',(0.000912521190919585,-0.0356916800276548,
-0.00931692352892374));
#32832=CARTESIAN_POINT('Ctrl Pts',(0.000578718474900576,-0.0357120031188721,
-0.00921993332101712));
#32833=CARTESIAN_POINT('Ctrl Pts',(0.000311390463711398,-0.0357279528770105,
-0.00917994576843555));
#32834=CARTESIAN_POINT('Ctrl Pts',(1.2640490683327E-6,-0.0357450060604786,
-0.00917557289780277));
#32835=CARTESIAN_POINT('Ctrl Pts',(-3.97773751530382E-5,-0.0357472374922339,
-0.00917583628752131));
#32836=CARTESIAN_POINT('Ctrl Pts',(-0.00010401540030905,-0.0357506915968563,
-0.00917756710042888));
#32837=CARTESIAN_POINT('Ctrl Pts',(-0.000127221269946943,-0.0357519315240605,
-0.00917846207972079));
#32838=CARTESIAN_POINT('Ctrl Pts',(-0.000170260321233034,-0.0357542171177686,
-0.0091806227014639));
#32839=CARTESIAN_POINT('Ctrl Pts',(-0.000190095700126816,-0.035755264932482,
-0.00918181613165416));
#32840=CARTESIAN_POINT('Ctrl Pts',(-0.000234161614358208,-0.0357575809579381,
-0.00918490711869147));
#32841=CARTESIAN_POINT('Ctrl Pts',(-0.000258384027387859,-0.0357588461088733,
-0.00918690223642446));
#32842=CARTESIAN_POINT('Ctrl Pts',(-0.000329993331741674,-0.0357625645113579,
-0.00919367747865179));
#32843=CARTESIAN_POINT('Ctrl Pts',(-0.000377294606204041,-0.0357649922616427,
-0.00919929197504775));
#32844=CARTESIAN_POINT('Ctrl Pts',(-0.000486192326624026,-0.0357705291573544,
-0.00921485551991437));
#32845=CARTESIAN_POINT('Ctrl Pts',(-0.000547652502143375,-0.0357736149414238,
-0.00922560447311942));
#32846=CARTESIAN_POINT('Ctrl Pts',(-0.00077809403146185,-0.0357851048795045,
-0.00927335716765128));
#32847=CARTESIAN_POINT('Ctrl Pts',(-0.000944098692126996,-0.0357931978196018,
-0.00932303136735014));
#32848=CARTESIAN_POINT('Ctrl Pts',(-0.00123300152870086,-0.0358080037030274,
-0.00943747928173621));
#32849=CARTESIAN_POINT('Ctrl Pts',(-0.0013574418274879,-0.0358146531628978,
-0.00949698614339815));
#32850=CARTESIAN_POINT('Ctrl Pts',(-0.00149692664947124,-0.0358228944549558,
-0.00957590769076583));
#32851=CARTESIAN_POINT('Ctrl Pts',(-0.00151638821710602,-0.03582406319409,
-0.00958721016462689));
#32852=CARTESIAN_POINT('Ctrl Pts',(-0.00154676225157033,-0.0358259200028109,
-0.0096053101999919));
#32853=CARTESIAN_POINT('Ctrl Pts',(-0.00155776167756375,-0.0358265992567676,
-0.00961196097860854));
#32854=CARTESIAN_POINT('Ctrl Pts',(-0.00157836009166009,-0.0358278848432368,
-0.00962459724626502));
#32855=CARTESIAN_POINT('Ctrl Pts',(-0.00158796841316746,-0.0358284901859162,
-0.00963056660996079));
#32856=CARTESIAN_POINT('Ctrl Pts',(-0.00161073364819649,-0.0358299377072133,
-0.00964488904518821));
#32857=CARTESIAN_POINT('Ctrl Pts',(-0.0016238595459862,-0.0358307829006293,
-0.00965329049633871));
#32858=CARTESIAN_POINT('Ctrl Pts',(-0.00166859978259292,-0.0358336985936239,
-0.00968242112911092));
#32859=CARTESIAN_POINT('Ctrl Pts',(-0.00169988635108253,-0.0358357975969619,
-0.00970364469975761));
#32860=CARTESIAN_POINT('Ctrl Pts',(-0.00177716194304706,-0.0358411177276784,
-0.00975822584444497));
#32861=CARTESIAN_POINT('Ctrl Pts',(-0.00182261951791848,-0.0358443712949381,
-0.00979230875885999));
#32862=CARTESIAN_POINT('Ctrl Pts',(-0.00205281636964779,-0.035861395976342,
-0.00997534134104765));
#32863=CARTESIAN_POINT('Ctrl Pts',(-0.00222040102343298,-0.0358755951013135,
-0.0101445613961145));
#32864=CARTESIAN_POINT('Ctrl Pts',(-0.00241927372754666,-0.035893960534741,
-0.0103997496023323));
#32865=CARTESIAN_POINT('Ctrl Pts',(-0.00246930624738904,-0.0358987599965681,
-0.0104699932953441));
#32866=CARTESIAN_POINT('Ctrl Pts',(-0.00253318293974001,-0.0359051400291047,
-0.0105683858663624));
#32867=CARTESIAN_POINT('Ctrl Pts',(-0.0025497120692482,-0.0359068169183037,
-0.0105947347661383));
#32868=CARTESIAN_POINT('Ctrl Pts',(-0.0025755790368098,-0.0359094846237416,
-0.0106374298462313));
#32869=CARTESIAN_POINT('Ctrl Pts',(-0.00258517768870117,-0.0359104847268032,
-0.0106536146731552));
#32870=CARTESIAN_POINT('Ctrl Pts',(-0.00260480559629456,-0.0359125516483981,
-0.0106874315651146));
#32871=CARTESIAN_POINT('Ctrl Pts',(-0.00261480959590133,-0.0359136175368941,
-0.0107050772263566));
#32872=CARTESIAN_POINT('Ctrl Pts',(-0.00263808771232186,-0.035916128349276,
-0.0107471249035681));
#32873=CARTESIAN_POINT('Ctrl Pts',(-0.00265120350205029,-0.0359175677036972,
-0.0107716126991749));
#32874=CARTESIAN_POINT('Ctrl Pts',(-0.00269520022554495,-0.0359224863568711,
-0.0108565710396449));
#32875=CARTESIAN_POINT('Ctrl Pts',(-0.00272436833485895,-0.0359259076037169,
-0.0109179073711483));
#32876=CARTESIAN_POINT('Ctrl Pts',(-0.00279222630517896,-0.035934345868882,
-0.0110740596658006));
#32877=CARTESIAN_POINT('Ctrl Pts',(-0.00282819169515727,-0.0359392843203902,
-0.0111699654192824));
#32878=CARTESIAN_POINT('Ctrl Pts',(-0.0029189285374855,-0.0359535815104554,
-0.0114555821162686));
#32879=CARTESIAN_POINT('Ctrl Pts',(-0.0029599679246924,-0.0359627342564858,
-0.0116490583439944));
#32880=CARTESIAN_POINT('Ctrl Pts',(-0.00298749116615407,-0.0359751427634141,
-0.0118972121940021));
#32881=CARTESIAN_POINT('Ctrl Pts',(-0.00299190092736898,-0.0359777920004475,
-0.0119494188085586));
#32882=CARTESIAN_POINT('Ctrl Pts',(-0.00299599531540426,-0.0359814481546266,
-0.0120198351449709));
#32883=CARTESIAN_POINT('Ctrl Pts',(-0.00299688457985966,-0.0359823970292153,
-0.0120379679209503));
#32884=CARTESIAN_POINT('Ctrl Pts',(-0.0029980328675489,-0.0359839144702652,
-0.0120667130621144));
#32885=CARTESIAN_POINT('Ctrl Pts',(-0.0029984002450903,-0.0359844773066483,
-0.0120773209219052));
#32886=CARTESIAN_POINT('Ctrl Pts',(-0.00299905304236399,-0.0359856650120847,
-0.012099585311108));
#32887=CARTESIAN_POINT('Ctrl Pts',(-0.002999326808685,-0.0359862905408736,
-0.0121112418630132));
#32888=CARTESIAN_POINT('Ctrl Pts',(-0.00299984268902756,-0.035987867465534,
-0.0121404635320267));
#32889=CARTESIAN_POINT('Ctrl Pts',(-0.00299999848009557,-0.0359888233622487,
-0.0121580296009286));
#32890=CARTESIAN_POINT('Ctrl Pts',(-0.00300000446576103,-0.0359926443202545,
-0.0122277151720247));
#32891=CARTESIAN_POINT('Ctrl Pts',(-0.00299865071308026,-0.0359955654232249,
-0.0122798231593143));
#32892=CARTESIAN_POINT('Ctrl Pts',(-0.00299119267042623,-0.0360037233650442,
-0.0124230410351089));
#32893=CARTESIAN_POINT('Ctrl Pts',(-0.00298228539517348,-0.0360090448149082,
-0.0125139473711002));
#32894=CARTESIAN_POINT('Ctrl Pts',(-0.0029369956463546,-0.0360276453175141,
-0.0128278163188737));
#32895=CARTESIAN_POINT('Ctrl Pts',(-0.00287960294277976,-0.036040969330536,
-0.0130470086908784));
#32896=CARTESIAN_POINT('Ctrl Pts',(-0.00277769058637646,-0.036056702744964,
-0.0133106009435901));
#32897=CARTESIAN_POINT('Ctrl Pts',(-0.0027557391732687,-0.0360598149919933,
-0.0133629166525026));
#32898=CARTESIAN_POINT('Ctrl Pts',(-0.00272170725122933,-0.036064266480404,
-0.0134379823683335));
#32899=CARTESIAN_POINT('Ctrl Pts',(-0.00271079755916636,-0.0360656441297542,
-0.0134612469341236));
#32900=CARTESIAN_POINT('Ctrl Pts',(-0.00269085028842581,-0.0360680781725724,
-0.0135024000169851));
#32901=CARTESIAN_POINT('Ctrl Pts',(-0.00268192991378836,-0.0360691384536184,
-0.0135203433260573));
#32902=CARTESIAN_POINT('Ctrl Pts',(-0.00266281773391231,-0.0360713525648563,
-0.013557840208983));
#32903=CARTESIAN_POINT('Ctrl Pts',(-0.00265258875598696,-0.0360725050377761,
-0.0135773735551754));
#32904=CARTESIAN_POINT('Ctrl Pts',(-0.00262481767440084,-0.0360755503132234,
-0.0136290120897287));
#32905=CARTESIAN_POINT('Ctrl Pts',(-0.0026069018317157,-0.0360774300754184,
-0.0136609126516327));
#32906=CARTESIAN_POINT('Ctrl Pts',(-0.00249102456812778,-0.0360890890793787,
-0.0138586790253759));
#32907=CARTESIAN_POINT('Ctrl Pts',(-0.00237786047785913,-0.0360982973943212,
-0.0140151180067865));
#32908=CARTESIAN_POINT('Ctrl Pts',(-0.00212381856825827,-0.0361165180276222,
-0.014303311021787));
#32909=CARTESIAN_POINT('Ctrl Pts',(-0.00198371673595574,-0.0361255015589338,
-0.01443451081625));
#32910=CARTESIAN_POINT('Ctrl Pts',(-0.00181014934738116,-0.0361366927959653,
-0.0145683680477551));
#32911=CARTESIAN_POINT('Ctrl Pts',(-0.00178797848923303,-0.0361381237947136,
-0.0145849818346945));
#32912=CARTESIAN_POINT('Ctrl Pts',(-0.00175442959424053,-0.0361402964925662,
-0.0146094035870066));
#32913=CARTESIAN_POINT('Ctrl Pts',(-0.0017432220614141,-0.0361410235150193,
-0.0146174443858314));
#32914=CARTESIAN_POINT('Ctrl Pts',(-0.00172282466151885,-0.0361423496054179,
-0.0146318663875494));
#32915=CARTESIAN_POINT('Ctrl Pts',(-0.00171365402088759,-0.0361429469267552,
-0.0146382738545781));
#32916=CARTESIAN_POINT('Ctrl Pts',(-0.00169274658924429,-0.0361443112357483,
-0.0146527083813521));
#32917=CARTESIAN_POINT('Ctrl Pts',(-0.00168098847057417,-0.0361450802202468,
-0.0146607033668935));
#32918=CARTESIAN_POINT('Ctrl Pts',(-0.00164431359148961,-0.0361474829283557,
-0.014685261181092));
#32919=CARTESIAN_POINT('Ctrl Pts',(-0.00161920624480304,-0.0361491337014477,
-0.0147015346149449));
#32920=CARTESIAN_POINT('Ctrl Pts',(-0.00148403081831568,-0.036158034850397,
-0.0147863051682421));
#32921=CARTESIAN_POINT('Ctrl Pts',(-0.00136985965557709,-0.0361655945145673,
-0.0148479846532686));
#32922=CARTESIAN_POINT('Ctrl Pts',(-0.0010299371033938,-0.0361875549046775,
-0.0150040999399211));
#32923=CARTESIAN_POINT('Ctrl Pts',(-0.000796130037670471,-0.0362019196288875,
-0.0150786043184217));
#32924=CARTESIAN_POINT('Ctrl Pts',(-0.000516810069068373,-0.0362175284952902,
-0.0151312696220082));
#32925=CARTESIAN_POINT('Ctrl Pts',(-0.000477625799261746,-0.0362196867764967,
-0.0151378546646231));
#32926=CARTESIAN_POINT('Ctrl Pts',(-0.000415630167953753,-0.0362230532810829,
-0.0151470109173127));
#32927=CARTESIAN_POINT('Ctrl Pts',(-0.000392901272377092,-0.0362242773700545,
-0.0151501018862697));
#32928=CARTESIAN_POINT('Ctrl Pts',(-0.000350400163917462,-0.036226547939529,
-0.0151553860281987));
#32929=CARTESIAN_POINT('Ctrl Pts',(-0.000330637378707389,-0.0362275963553301,
-0.0151576437859936));
#32930=CARTESIAN_POINT('Ctrl Pts',(-0.000286319573974246,-0.0362299314524598,
-0.0151622607498318));
#32931=CARTESIAN_POINT('Ctrl Pts',(-0.000261754830036736,-0.0362312148140198,
-0.0151645140051839));
#32932=CARTESIAN_POINT('Ctrl Pts',(-0.000187797776576142,-0.0362350475724103,
-0.0151703790261994));
#32933=CARTESIAN_POINT('Ctrl Pts',(-0.000138339992681926,-0.0362375689594494,
-0.0151730711308622));
#32934=CARTESIAN_POINT('Ctrl Pts',(0.000116250536762689,-0.0362503682636465,
-0.0151806134042614));
#32935=CARTESIAN_POINT('Ctrl Pts',(0.000321419199358098,-0.0362600363131822,
-0.0151656348821813));
#32936=CARTESIAN_POINT('Ctrl Pts',(0.000674690224411421,-0.0362770596895092,
-0.0151030328860211));
#32937=CARTESIAN_POINT('Ctrl Pts',(0.000823621058036811,-0.0362843764791667,
-0.015064663907936));
#32938=CARTESIAN_POINT('Ctrl Pts',(0.000997093887906155,-0.0362937102196635,
-0.0150054625301104));
#32939=CARTESIAN_POINT('Ctrl Pts',(0.00102509814223837,-0.0362952434151831,
-0.0149954380726004));
#32940=CARTESIAN_POINT('Ctrl Pts',(0.00106623107715375,-0.036297540864094,
-0.0149800202802216));
#32941=CARTESIAN_POINT('Ctrl Pts',(0.00107947870708767,-0.036298287844663,
-0.0149749472370169));
#32942=CARTESIAN_POINT('Ctrl Pts',(0.00110310804554624,-0.0362996336666335,
-0.0149657059325244));
#32943=CARTESIAN_POINT('Ctrl Pts',(0.00111350310949635,-0.0363002304631388,
-0.0149615732947957));
#32944=CARTESIAN_POINT('Ctrl Pts',(0.00113669207131603,-0.036301572492908,
-0.0149522038103222));
#32945=CARTESIAN_POINT('Ctrl Pts',(0.0011494729228974,-0.0363023194212357,
-0.0149469366632353));
#32946=CARTESIAN_POINT('Ctrl Pts',(0.00118789914223002,-0.0363045860209889,
-0.0149307891644975));
#32947=CARTESIAN_POINT('Ctrl Pts',(0.00121342916770938,-0.0363061201901037,
-0.0149196400148282));
#32948=CARTESIAN_POINT('Ctrl Pts',(0.00133940120861653,-0.0363138180789388,
-0.0148625251346083));
#32949=CARTESIAN_POINT('Ctrl Pts',(0.00143739996686642,-0.0363202113048059,
-0.0148113947578893));
#32950=CARTESIAN_POINT('Ctrl Pts',(0.00175730887216658,-0.0363419866340859,
-0.0146213260183779));
#32951=CARTESIAN_POINT('Ctrl Pts',(0.00196386152873907,-0.0363574793432828,
-0.014458781871455));
#32952=CARTESIAN_POINT('Ctrl Pts',(0.00217389430384587,-0.0363740361980171,
-0.0142436294527254));
#32953=CARTESIAN_POINT('Ctrl Pts',(0.00220053740300941,-0.0363761570975972,
-0.0142152527195389));
#32954=CARTESIAN_POINT('Ctrl Pts',(0.00224321190486484,-0.0363795894882185,
-0.0141679911262435));
#32955=CARTESIAN_POINT('Ctrl Pts',(0.00225957440740101,-0.0363809144952551,
-0.0141494126014718));
#32956=CARTESIAN_POINT('Ctrl Pts',(0.00228866992933204,-0.0363832875454547,
-0.0141155403310367));
#32957=CARTESIAN_POINT('Ctrl Pts',(0.00230148417241686,-0.036384338842024,
-0.0141003185383934));
#32958=CARTESIAN_POINT('Ctrl Pts',(0.00232870134266448,-0.0363865856821838,
-0.0140673270993386));
#32959=CARTESIAN_POINT('Ctrl Pts',(0.0023430544507531,-0.0363877792154732,
-0.0140495178793561));
#32960=CARTESIAN_POINT('Ctrl Pts',(0.00238225824026796,-0.0363910648052641,
-0.0139997190718823));
#32961=CARTESIAN_POINT('Ctrl Pts',(0.00240666726536358,-0.0363931398080355,
-0.0139673871536493));
#32962=CARTESIAN_POINT('Ctrl Pts',(0.00255034639338418,-0.0364055566190344,
-0.0137688333369805));
#32963=CARTESIAN_POINT('Ctrl Pts',(0.00265301248107068,-0.0364152588639168,
-0.0135912633896652));
#32964=CARTESIAN_POINT('Ctrl Pts',(0.00280657010375567,-0.0364330326520467,
-0.0132492448683431));
#32965=CARTESIAN_POINT('Ctrl Pts',(0.00286296272161191,-0.0364410903712434,
-0.0130882337540886));
#32966=CARTESIAN_POINT('Ctrl Pts',(0.00291262039576375,-0.0364512484975482,
-0.012895217561391));
#32967=CARTESIAN_POINT('Ctrl Pts',(0.00291944394782601,-0.0364527457688092,
-0.0128670041007212));
#32968=CARTESIAN_POINT('Ctrl Pts',(0.00292896107046031,-0.0364549994289248,
-0.0128249945978945));
#32969=CARTESIAN_POINT('Ctrl Pts',(0.00293196896862156,-0.036455739480162,
-0.0128112707447091));
#32970=CARTESIAN_POINT('Ctrl Pts',(0.0029371980543264,-0.0364570783169823,
-0.0127865845601266));
#32971=CARTESIAN_POINT('Ctrl Pts',(0.00293945448876798,-0.0364576751605383,
-0.0127756302445659));
#32972=CARTESIAN_POINT('Ctrl Pts',(0.0029443881296107,-0.0364590243324186,
-0.0127509821567199));
#32973=CARTESIAN_POINT('Ctrl Pts',(0.00294703107634154,-0.0364597784548663,
-0.0127372822624239));
#32974=CARTESIAN_POINT('Ctrl Pts',(0.00295478538395082,-0.0364620889218922,
-0.0126955231591981));
#32975=CARTESIAN_POINT('Ctrl Pts',(0.00295959212610445,-0.0364636605647079,
-0.0126674097665459));
#32976=CARTESIAN_POINT('Ctrl Pts',(0.00298196990773466,-0.0364717299512634,
-0.0125242708731424));
#32977=CARTESIAN_POINT('Ctrl Pts',(0.00299323769398351,-0.0364784807095211,
-0.0124083685500126));
#32978=CARTESIAN_POINT('Ctrl Pts',(0.0030057654876214,-0.0364974208622691,
-0.012085345771044));
#32979=CARTESIAN_POINT('Ctrl Pts',(0.00299237074063453,-0.0365096628881006,
-0.0118782768645188));
#32980=CARTESIAN_POINT('Ctrl Pts',(0.00294535016614654,-0.0365255166214546,
-0.0116010276599633));
#32981=CARTESIAN_POINT('Ctrl Pts',(0.00293022238353103,-0.0365296293113734,
-0.0115283116476631));
#32982=CARTESIAN_POINT('Ctrl Pts',(0.00290533963104305,-0.0365352595648814,
-0.0114276082146904));
#32983=CARTESIAN_POINT('Ctrl Pts',(0.00289784653207465,-0.0365368464537141,
-0.0113990942378676));
#32984=CARTESIAN_POINT('Ctrl Pts',(0.00288446375329487,-0.0365395080808752,
-0.0113510597922487));
#32985=CARTESIAN_POINT('Ctrl Pts',(0.00287879328157979,-0.0365405896676996,
-0.0113314809031983));
#32986=CARTESIAN_POINT('Ctrl Pts',(0.00286691521852962,-0.036542765596481,
-0.0112919797198651));
#32987=CARTESIAN_POINT('Ctrl Pts',(0.00286069843270487,-0.0365438595744673,
-0.011272061353524));
#32988=CARTESIAN_POINT('Ctrl Pts',(0.00284475981024879,-0.0365465575247099,
-0.011222807320906));
#32989=CARTESIAN_POINT('Ctrl Pts',(0.0028347914317321,-0.0365481535001276,
-0.0111935536278561));
#32990=CARTESIAN_POINT('Ctrl Pts',(0.00279329964189367,-0.0365544544545892,
-0.0110776856491529));
#32991=CARTESIAN_POINT('Ctrl Pts',(0.00275824297825931,-0.0365590452878288,
-0.0109923869126421));
#32992=CARTESIAN_POINT('Ctrl Pts',(0.00264740074443722,-0.0365718638606297,
-0.0107544945394076));
#32993=CARTESIAN_POINT('Ctrl Pts',(0.00256248164488157,-0.0365798388836663,
-0.0106065602530943));
#32994=CARTESIAN_POINT('Ctrl Pts',(0.00238494659545061,-0.0365946746051794,
-0.0103504753036083));
#32995=CARTESIAN_POINT('Ctrl Pts',(0.00229632337619972,-0.0366014836238115,
-0.010240170970903));
#32996=CARTESIAN_POINT('Ctrl Pts',(0.00218494895902605,-0.0366099084212479,
-0.0101200065252737));
#32997=CARTESIAN_POINT('Ctrl Pts',(0.00216944445717086,-0.0366110786895943,
-0.0101036519089914));
#32998=CARTESIAN_POINT('Ctrl Pts',(0.00214480495625915,-0.0366129374017226,
-0.0100782410495192));
#32999=CARTESIAN_POINT('Ctrl Pts',(0.00213579317251943,-0.0366136170002465,
-0.0100690659433162));
#33000=CARTESIAN_POINT('Ctrl Pts',(0.00211874570625072,-0.0366149028298883,
-0.0100519313120288));
#33001=CARTESIAN_POINT('Ctrl Pts',(0.00211072364031695,-0.0366155080653574,
-0.010043958912748));
#33002=CARTESIAN_POINT('Ctrl Pts',(0.0020915500342721,-0.0366169547660525,
-0.0100251183128678));
#33003=CARTESIAN_POINT('Ctrl Pts',(0.00208035869424938,-0.0366177992364829,
-0.0100142913153454));
#33004=CARTESIAN_POINT('Ctrl Pts',(0.00204176856454916,-0.0366207097053319,
-0.00997753480300241));
#33005=CARTESIAN_POINT('Ctrl Pts',(0.00201396619849019,-0.0366228040759775,
-0.00995203608989637));
#33006=CARTESIAN_POINT('Ctrl Pts',(0.00194323780956477,-0.0366281096275946,
-0.00988958242850173));
#33007=CARTESIAN_POINT('Ctrl Pts',(0.0018997327068062,-0.0366313530404973,
-0.00985330669503815));
#33008=CARTESIAN_POINT('Ctrl Pts',(0.00167043419294685,-0.0366482420893763,
-0.00967286592462395));
#33009=CARTESIAN_POINT('Ctrl Pts',(0.00146915479416005,-0.0366623117469007,
-0.00954965853702657));
#33010=CARTESIAN_POINT('Ctrl Pts',(0.00117549151968438,-0.0366806854025545,
-0.00941433367250835));
#33011=CARTESIAN_POINT('Ctrl Pts',(0.00109383854871171,-0.0366855976305841,
-0.00938098473124982));
#33012=CARTESIAN_POINT('Ctrl Pts',(0.00098134625636968,-0.0366920973499346,
-0.00934072716949374));
#33013=CARTESIAN_POINT('Ctrl Pts',(0.000951699117684725,-0.0366937860358502,
-0.0093306380988298));
#33014=CARTESIAN_POINT('Ctrl Pts',(0.000901964581640302,-0.0366965793944118,
-0.00931457757477032));
#33015=CARTESIAN_POINT('Ctrl Pts',(0.000881963296006947,-0.0366976922472465,
-0.00930834921859086));
#33016=CARTESIAN_POINT('Ctrl Pts',(0.000842209702367135,-0.036699883800035,
-0.00929642533591894));
#33017=CARTESIAN_POINT('Ctrl Pts',(0.000822460854643503,-0.0367009626895432,
-0.00929072232315037));
#33018=CARTESIAN_POINT('Ctrl Pts',(0.00077441871185937,-0.0367035642101964,
-0.00927738224183657));
#33019=CARTESIAN_POINT('Ctrl Pts',(0.000746068838789926,-0.0367050801130852,
-0.00926995581700696));
#33020=CARTESIAN_POINT('Ctrl Pts',(0.000641096027188231,-0.0367106264794309,
-0.00924409506994982));
#33021=CARTESIAN_POINT('Ctrl Pts',(0.000563861671009458,-0.0367145760332935,
-0.00922826585836568));
#33022=CARTESIAN_POINT('Ctrl Pts',(0.000358759315627147,-0.03672480538856,
-0.00919458815514616));
#33023=CARTESIAN_POINT('Ctrl Pts',(0.000230208683209771,-0.0367309507413409,
-0.00918191668380646));
#33024=CARTESIAN_POINT('Ctrl Pts',(-9.00185525693171E-5,-0.0367461468814493,
-0.00917110414474542));
#33025=CARTESIAN_POINT('Ctrl Pts',(-0.000281433776674939,-0.0367551235167671,
-0.00918296170668082));
#33026=CARTESIAN_POINT('Ctrl Pts',(-0.000497765622491052,-0.0367663070708568,
-0.00921730674930765));
#33027=CARTESIAN_POINT('Ctrl Pts',(-0.000525077258624144,-0.0367677386903863,
-0.00922203169455336));
#33028=CARTESIAN_POINT('Ctrl Pts',(-0.00056587886809098,-0.0367699121477052,
-0.00922967416104993));
#33029=CARTESIAN_POINT('Ctrl Pts',(-0.000579421221987906,-0.0367706392936709,
-0.00923230757331932));
#33030=CARTESIAN_POINT('Ctrl Pts',(-0.000603911681821247,-0.0367719655023004,
-0.00923724547920457));
#33031=CARTESIAN_POINT('Ctrl Pts',(-0.0006148657016026,-0.0367725628164889,
-0.00923951793029843));
#33032=CARTESIAN_POINT('Ctrl Pts',(-0.000639710303475704,-0.0367739269704792,
-0.00924481715111586));
#33033=CARTESIAN_POINT('Ctrl Pts',(-0.00065359220211092,-0.0367746958050904,
-0.00924788140880198));
#33034=CARTESIAN_POINT('Ctrl Pts',(-0.000696607047403286,-0.0367770975716373,
-0.00925769754465249));
#33035=CARTESIAN_POINT('Ctrl Pts',(-0.000725660404111588,-0.0367787475347113,
-0.00926478627289187));
#33036=CARTESIAN_POINT('Ctrl Pts',(-0.000879936119126035,-0.0367876398206301,
-0.00930488095683669));
#33037=CARTESIAN_POINT('Ctrl Pts',(-0.00100302097123913,-0.0367951908062692,
-0.00934553287137309));
#33038=CARTESIAN_POINT('Ctrl Pts',(-0.00134999711134431,-0.0368171583481161,
-0.00948561362835855));
#33039=CARTESIAN_POINT('Ctrl Pts',(-0.0015648898522476,-0.0368315395698085,
-0.00960465929852245));
#33040=CARTESIAN_POINT('Ctrl Pts',(-0.00179504554140822,-0.0368471591859041,
-0.00977181808903299));
#33041=CARTESIAN_POINT('Ctrl Pts',(-0.00182667875586705,-0.0368493142030486,
-0.00979576533585459));
#33042=CARTESIAN_POINT('Ctrl Pts',(-0.00187582820077025,-0.0368526767936784,
-0.00983453013964745));
#33043=CARTESIAN_POINT('Ctrl Pts',(-0.00189366464718435,-0.0368539001719131,
-0.00984893262602421));
#33044=CARTESIAN_POINT('Ctrl Pts',(-0.00192666654807844,-0.0368561700798597,
-0.0098762116423573));
#33045=CARTESIAN_POINT('Ctrl Pts',(-0.00194187230772095,-0.0368572185352222,
-0.00988903723687733));
#33046=CARTESIAN_POINT('Ctrl Pts',(-0.00197565860381956,-0.0368595545506384,
-0.0099181149559936));
#33047=CARTESIAN_POINT('Ctrl Pts',(-0.00199416848711677,-0.0368608387785798,
-0.00993444716980923));
#33048=CARTESIAN_POINT('Ctrl Pts',(-0.00204926890635601,-0.0368646770293317,
-0.00998428799926465));
#33049=CARTESIAN_POINT('Ctrl Pts',(-0.00208523267764469,-0.0368672029188704,
-0.0100184783792989));
#33050=CARTESIAN_POINT('Ctrl Pts',(-0.00226552429857299,-0.0368800087819219,
-0.0101986023311671));
#33051=CARTESIAN_POINT('Ctrl Pts',(-0.00239544736210209,-0.0368896788398055,
-0.0103581733530736));
#33052=CARTESIAN_POINT('Ctrl Pts',(-0.00259220574585257,-0.0369066939174307,
-0.0106579656236349));
#33053=CARTESIAN_POINT('Ctrl Pts',(-0.00266638302995268,-0.0369139999167096,
-0.010792413259548));
#33054=CARTESIAN_POINT('Ctrl Pts',(-0.00274229612521887,-0.0369233223798479,
-0.0109590138959835));
#33055=CARTESIAN_POINT('Ctrl Pts',(-0.00275423495015243,-0.036924856793475,
-0.010986283677699));
#33056=CARTESIAN_POINT('Ctrl Pts',(-0.00277126261280445,-0.0369271557259446,
-0.0110268080745781));
#33057=CARTESIAN_POINT('Ctrl Pts',(-0.00277666664411211,-0.0369279029398237,
-0.0110399291253249));
#33058=CARTESIAN_POINT('Ctrl Pts',(-0.0027861640698091,-0.0369292489992423,
-0.0110634617525319));
#33059=CARTESIAN_POINT('Ctrl Pts',(-0.00279029259871304,-0.0369298457964329,
-0.011073858570028));
#33060=CARTESIAN_POINT('Ctrl Pts',(-0.00279939131751406,-0.0369311875956844,
-0.0110971507181222));
#33061=CARTESIAN_POINT('Ctrl Pts',(-0.00280433057080931,-0.0369319342895694,
-0.0111100573330409));
#33062=CARTESIAN_POINT('Ctrl Pts',(-0.00281894963931801,-0.0369341994680632,
-0.0111490632400563));
#33063=CARTESIAN_POINT('Ctrl Pts',(-0.00282835530145968,-0.0369357324247709,
-0.0111752629362362));
#33064=CARTESIAN_POINT('Ctrl Pts',(-0.00287320611079789,-0.0369434185187938,
-0.0113058839811864));
#33065=CARTESIAN_POINT('Ctrl Pts',(-0.00290323726482158,-0.0369498004327213,
-0.0114120669032405));
#33066=CARTESIAN_POINT('Ctrl Pts',(-0.00297553762605092,-0.03696914222798,
-0.0117346034232676));
#33067=CARTESIAN_POINT('Ctrl Pts',(-0.00299990468521026,-0.0369821981326441,
-0.0119542272990632));
#33068=CARTESIAN_POINT('Ctrl Pts',(-0.00299999972093215,-0.0369945846061161,
-0.0121745592977555));
#33069=CARTESIAN_POINT('',(-0.0029999998192441,-0.0399949849792216,-0.0121748118762893));
#33070=CARTESIAN_POINT('Ctrl Pts',(-0.00299999972093215,-0.0369945846061161,
-0.0121745592977554));
#33071=CARTESIAN_POINT('Ctrl Pts',(-0.00300002044309324,-0.0369972854273804,
-0.0122226018135391));
#33072=CARTESIAN_POINT('Ctrl Pts',(-0.00299888744122127,-0.036999954978733,
-0.0122706295676167));
#33073=CARTESIAN_POINT('Ctrl Pts',(-0.00299499082230191,-0.0370044480830774,
-0.012352416913827));
#33074=CARTESIAN_POINT('Ctrl Pts',(-0.00299280903808429,-0.0370062877432467,
-0.0123861838072021));
#33075=CARTESIAN_POINT('Ctrl Pts',(-0.00298845331848487,-0.0370091714159223,
-0.0124395483674484));
#33076=CARTESIAN_POINT('Ctrl Pts',(-0.00298665668657259,-0.0370102268141541,
-0.0124591732365225));
#33077=CARTESIAN_POINT('Ctrl Pts',(-0.00298274368844551,-0.0370122905234387,
-0.0124977271901588));
#33078=CARTESIAN_POINT('Ctrl Pts',(-0.0029806401715497,-0.0370132991780978,
-0.0125166566183005));
#33079=CARTESIAN_POINT('Ctrl Pts',(-0.00297578076485031,-0.0370154337400218,
-0.0125568917393376));
#33080=CARTESIAN_POINT('Ctrl Pts',(-0.00297297599174496,-0.0370165580796817,
-0.012578190516932));
#33081=CARTESIAN_POINT('Ctrl Pts',(-0.0029651561954335,-0.0370194387258182,
-0.012633016070175));
#33082=CARTESIAN_POINT('Ctrl Pts',(-0.00295980119818566,-0.0370211844854742,
-0.0126664917065591));
#33083=CARTESIAN_POINT('Ctrl Pts',(-0.00293371205169528,-0.0370288041114952,
-0.0128135560272379));
#33084=CARTESIAN_POINT('Ctrl Pts',(-0.00290699715426476,-0.0370344929313124,
-0.0129259880337695));
#33085=CARTESIAN_POINT('Ctrl Pts',(-0.00282859361209651,-0.0370476857028708,
-0.0131877595939289));
#33086=CARTESIAN_POINT('Ctrl Pts',(-0.00277146896525616,-0.0370550638819975,
-0.013335101189664));
#33087=CARTESIAN_POINT('Ctrl Pts',(-0.00265315300429085,-0.037068102831315,
-0.0135808422605973));
#33088=CARTESIAN_POINT('Ctrl Pts',(-0.00259737631624408,-0.0370736802610889,
-0.0136814584216503));
#33089=CARTESIAN_POINT('Ctrl Pts',(-0.00252081613852199,-0.0370809905291002,
-0.013802595614908));
#33090=CARTESIAN_POINT('Ctrl Pts',(-0.00250532288371242,-0.0370824546846683,
-0.0138263567689643));
#33091=CARTESIAN_POINT('Ctrl Pts',(-0.00248172659690742,-0.0370846679180651,
-0.0138614472282185));
#33092=CARTESIAN_POINT('Ctrl Pts',(-0.00247387743128668,-0.0370854014986492,
-0.0138729461767796));
#33093=CARTESIAN_POINT('Ctrl Pts',(-0.00245957864348211,-0.0370867339378084,
-0.013893583766505));
#33094=CARTESIAN_POINT('Ctrl Pts',(-0.00245315757200238,-0.0370873309510449,
-0.0139027415352423));
#33095=CARTESIAN_POINT('Ctrl Pts',(-0.00243853728434795,-0.0370886873438808,
-0.0139233469712934));
#33096=CARTESIAN_POINT('Ctrl Pts',(-0.00243030863270394,-0.0370894486154127,
-0.013934772898004));
#33097=CARTESIAN_POINT('Ctrl Pts',(-0.00240477593244303,-0.0370918031743114,
-0.0139697052009798));
#33098=CARTESIAN_POINT('Ctrl Pts',(-0.00238720946407241,-0.0370934125854988,
-0.0139930166878927));
#33099=CARTESIAN_POINT('Ctrl Pts',(-0.00223219197604203,-0.0371074991872236,
-0.0141926042982427));
#33100=CARTESIAN_POINT('Ctrl Pts',(-0.00207578302806841,-0.0371208839489748,
-0.0143532566941638));
#33101=CARTESIAN_POINT('Ctrl Pts',(-0.0018205562500794,-0.0371401449311814,
-0.0145626807052035));
#33102=CARTESIAN_POINT('Ctrl Pts',(-0.00173457132032445,-0.0371462847788871,
-0.0146258809382894));
#33103=CARTESIAN_POINT('Ctrl Pts',(-0.00160560038026694,-0.0371549488219101,
-0.0147104760708857));
#33104=CARTESIAN_POINT('Ctrl Pts',(-0.00156518619011357,-0.0371575920287867,
-0.014735630184333));
#33105=CARTESIAN_POINT('Ctrl Pts',(-0.00149081407952689,-0.0371623270430561,
-0.0147794997362258));
#33106=CARTESIAN_POINT('Ctrl Pts',(-0.00145705986625813,-0.0371644295871248,
-0.014798538588036));
#33107=CARTESIAN_POINT('Ctrl Pts',(-0.00140313272875679,-0.0371677171758412,
-0.0148275932857108));
#33108=CARTESIAN_POINT('Ctrl Pts',(-0.00138320044839812,-0.0371689172351352,
-0.0148380446835801));
#33109=CARTESIAN_POINT('Ctrl Pts',(-0.00134538638621148,-0.0371711661406242,
-0.0148573329546732));
#33110=CARTESIAN_POINT('Ctrl Pts',(-0.00132753050291453,-0.0371722165903185,
-0.0148662176722987));
#33111=CARTESIAN_POINT('Ctrl Pts',(-0.00128682026186918,-0.0371745861967653,
-0.0148859702516155));
#33112=CARTESIAN_POINT('Ctrl Pts',(-0.00126391418380141,-0.0371759015780273,
-0.0148967283915958));
#33113=CARTESIAN_POINT('Ctrl Pts',(-0.00119265434133246,-0.0371799406994135,
-0.0149291024015441));
#33114=CARTESIAN_POINT('Ctrl Pts',(-0.00114386112634324,-0.037182631598501,
-0.0149497291333713));
#33115=CARTESIAN_POINT('Ctrl Pts',(-0.000880427758573214,-0.0371968095614718,
-0.0150529583010294));
#33116=CARTESIAN_POINT('Ctrl Pts',(-0.000657379722192128,-0.0372075190551629,
-0.0151119633160031));
#33117=CARTESIAN_POINT('Ctrl Pts',(-0.000338363856336814,-0.0372228871702796,
-0.0151581411054175));
#33118=CARTESIAN_POINT('Ctrl Pts',(-0.000246396792648505,-0.0372273338265884,
-0.0151671435738797));
#33119=CARTESIAN_POINT('Ctrl Pts',(-0.000101732598820027,-0.0372345380187635,
-0.0151745875303708));
#33120=CARTESIAN_POINT('Ctrl Pts',(-4.9239780400128E-5,-0.0372371954855935,
-0.0151759085239918));
#33121=CARTESIAN_POINT('Ctrl Pts',(2.08703028142546E-5,-0.0372408334751768,
-0.0151758323925362));
#33122=CARTESIAN_POINT('Ctrl Pts',(3.84820360315202E-5,-0.0372417548179085,
-0.0151756581652024));
#33123=CARTESIAN_POINT('Ctrl Pts',(6.77578217498163E-5,-0.0372433002521556,
-0.0151751107020802));
#33124=CARTESIAN_POINT('Ctrl Pts',(7.94233512608195E-5,-0.037243919733841,
-0.0151748244590345));
#33125=CARTESIAN_POINT('Ctrl Pts',(0.000103161117889949,-0.0372451882798842,
-0.0151741033940211));
#33126=CARTESIAN_POINT('Ctrl Pts',(0.000115232879814928,-0.0372458375703076,
-0.0151736637035798));
#33127=CARTESIAN_POINT('Ctrl Pts',(0.000146820030051706,-0.0372475468571941,
-0.0151723221319126));
#33128=CARTESIAN_POINT('Ctrl Pts',(0.000166329551303206,-0.0372486129221587,
-0.0151713025188336));
#33129=CARTESIAN_POINT('Ctrl Pts',(0.000250631803590922,-0.0372532601648237,
-0.0151660705880903));
#33130=CARTESIAN_POINT('Ctrl Pts',(0.000315284714862968,-0.0372569279704126,
-0.0151599461572649));
#33131=CARTESIAN_POINT('Ctrl Pts',(0.000545366834080181,-0.0372702371484968,
-0.0151305906431541));
#33132=CARTESIAN_POINT('Ctrl Pts',(0.000708992075988477,-0.0372801612482176,
-0.0150956524265341));
#33133=CARTESIAN_POINT('Ctrl Pts',(0.00102219420103656,-0.0372992835294335,
-0.0150008814363621));
#33134=CARTESIAN_POINT('Ctrl Pts',(0.00117158357947138,-0.0373084634288394,
-0.0149422712382416));
#33135=CARTESIAN_POINT('Ctrl Pts',(0.00135146440412296,-0.0373194516452926,
-0.014854497933067));
#33136=CARTESIAN_POINT('Ctrl Pts',(0.00138698451412708,-0.0373216193006787,
-0.0148362794446832));
#33137=CARTESIAN_POINT('Ctrl Pts',(0.0014421622064965,-0.0373249843645516,
-0.0148065729005021));
#33138=CARTESIAN_POINT('Ctrl Pts',(0.00146206977513875,-0.0373261980010782,
-0.0147955611954879));
#33139=CARTESIAN_POINT('Ctrl Pts',(0.00149916198486166,-0.0373284589626624,
-0.0147744894185091));
#33140=CARTESIAN_POINT('Ctrl Pts',(0.00151637536302494,-0.0373295080801955,
-0.0147644826897266));
#33141=CARTESIAN_POINT('Ctrl Pts',(0.00155491507616576,-0.037331857277806,
-0.0147415618848708));
#33142=CARTESIAN_POINT('Ctrl Pts',(0.00157618274298463,-0.0373331538500317,
-0.0147285517636009));
#33143=CARTESIAN_POINT('Ctrl Pts',(0.00163073857920877,-0.03733648197205,
-0.0146942363965434));
#33144=CARTESIAN_POINT('Ctrl Pts',(0.00166377281675525,-0.0373384992548174,
-0.0146725354843417));
#33145=CARTESIAN_POINT('Ctrl Pts',(0.00190972404152861,-0.0373535592438023,
-0.014503914698254));
#33146=CARTESIAN_POINT('Ctrl Pts',(0.00210325364473563,-0.0373655228288524,
-0.0143306715972191));
#33147=CARTESIAN_POINT('Ctrl Pts',(0.0023453447593637,-0.0373832651392373,
-0.0140498645242398));
#33148=CARTESIAN_POINT('Ctrl Pts',(0.00241370426447676,-0.037388711233053,
-0.0139609549110292));
#33149=CARTESIAN_POINT('Ctrl Pts',(0.0024927455841174,-0.0373958609720388,
-0.0138452860628398));
#33150=CARTESIAN_POINT('Ctrl Pts',(0.00250824069277282,-0.037397308889097,
-0.0138219136931857));
#33151=CARTESIAN_POINT('Ctrl Pts',(0.00253090100950291,-0.0373995022775469,
-0.0137866705232363));
#33152=CARTESIAN_POINT('Ctrl Pts',(0.00253831563468918,-0.037400232656178,
-0.0137749611046467));
#33153=CARTESIAN_POINT('Ctrl Pts',(0.00255156743641552,-0.0374015619777372,
-0.0137537090294394));
#33154=CARTESIAN_POINT('Ctrl Pts',(0.00255743273512644,-0.0374021591234302,
-0.0137441845411578));
#33155=CARTESIAN_POINT('Ctrl Pts',(0.00257059538114897,-0.0374035193023665,
-0.013722539914486));
#33156=CARTESIAN_POINT('Ctrl Pts',(0.00257786032128642,-0.0374042842779993,
-0.0137104008702787));
#33157=CARTESIAN_POINT('Ctrl Pts',(0.00260002822468843,-0.0374066618840454,
-0.0136727586730617));
#33158=CARTESIAN_POINT('Ctrl Pts',(0.00261464019585624,-0.0374082910782125,
-0.0136470871305454));
#33159=CARTESIAN_POINT('Ctrl Pts',(0.00270220658746547,-0.0374184262177816,
-0.0134878174700126));
#33160=CARTESIAN_POINT('Ctrl Pts',(0.00276527951816509,-0.0374273627007037,
-0.0133490510875615));
#33161=CARTESIAN_POINT('Ctrl Pts',(0.00288458392718222,-0.0374477836794666,
-0.0130227774474267));
#33162=CARTESIAN_POINT('Ctrl Pts',(0.002933575167356,-0.0374592043657586,
-0.0128333172933975));
#33163=CARTESIAN_POINT('Ctrl Pts',(0.00297266017997057,-0.037473260151968,
-0.0125839673303088));
#33164=CARTESIAN_POINT('Ctrl Pts',(0.00297989501878687,-0.037476396424312,
-0.0125272674231773));
#33165=CARTESIAN_POINT('Ctrl Pts',(0.00298806324686612,-0.0374808903773776,
-0.0124444727489461));
#33166=CARTESIAN_POINT('Ctrl Pts',(0.00299028280805924,-0.0374822869104341,
-0.0124185200714889));
#33167=CARTESIAN_POINT('Ctrl Pts',(0.00299361066697225,-0.0374847388873987,
-0.0123725668869731));
#33168=CARTESIAN_POINT('Ctrl Pts',(0.00299485715402919,-0.0374857985029798,
-0.0123525782677314));
#33169=CARTESIAN_POINT('Ctrl Pts',(0.00299705750808612,-0.0374880141205574,
-0.0123105170379525));
#33170=CARTESIAN_POINT('Ctrl Pts',(0.00299796790448567,-0.0374891687295452,
-0.0122884432973145));
#33171=CARTESIAN_POINT('Ctrl Pts',(0.00299974422656263,-0.0374922264601912,
-0.0122295915892838));
#33172=CARTESIAN_POINT('Ctrl Pts',(0.00300017767121487,-0.0374941163446732,
-0.0121928038145459));
#33173=CARTESIAN_POINT('Ctrl Pts',(0.00299880250555736,-0.037504692502762,
-0.0119848382545637));
#33174=CARTESIAN_POINT('Ctrl Pts',(0.00298302146881439,-0.0375129412064582,
-0.0118140605827843));
#33175=CARTESIAN_POINT('Ctrl Pts',(0.00292980333788672,-0.0375272513084608,
-0.0115177380114177));
#33176=CARTESIAN_POINT('Ctrl Pts',(0.00289857466076249,-0.0375333522074619,
-0.011391553369944));
#33177=CARTESIAN_POINT('Ctrl Pts',(0.00283083713085173,-0.037544181788,
-0.0111782636316869));
#33178=CARTESIAN_POINT('Ctrl Pts',(0.00279821676528967,-0.0375488192113112,
-0.0110901258412438));
#33179=CARTESIAN_POINT('Ctrl Pts',(0.00275329122241311,-0.0375547481661455,
-0.0109842867149117));
#33180=CARTESIAN_POINT('Ctrl Pts',(0.00274485953352157,-0.0375558442465599,
-0.0109649901466173));
#33181=CARTESIAN_POINT('Ctrl Pts',(0.00273113664496737,-0.0375576046980961,
-0.0109344642778422));
#33182=CARTESIAN_POINT('Ctrl Pts',(0.00272597754827251,-0.0375582615292014,
-0.0109231759777802));
#33183=CARTESIAN_POINT('Ctrl Pts',(0.002715970479512,-0.0375595267206954,
-0.0109016347115573));
#33184=CARTESIAN_POINT('Ctrl Pts',(0.00271113419474063,-0.0375601344054861,
-0.0108913767451032));
#33185=CARTESIAN_POINT('Ctrl Pts',(0.00269912675937915,-0.0375616336472831,
-0.0108662783933782));
#33186=CARTESIAN_POINT('Ctrl Pts',(0.00269189128805988,-0.0375625289554351,
-0.0108514693041431));
#33187=CARTESIAN_POINT('Ctrl Pts',(0.00266630623366604,-0.0375656651415887,
-0.0108001794102768));
#33188=CARTESIAN_POINT('Ctrl Pts',(0.00264733478122021,-0.0375679390852926,
-0.0107640155522906));
#33189=CARTESIAN_POINT('Ctrl Pts',(0.00250100657200337,-0.0375850491183667,
-0.0104984060320765));
#33190=CARTESIAN_POINT('Ctrl Pts',(0.00234477208838719,-0.0376008994558459,
-0.0102861651716031));
#33191=CARTESIAN_POINT('Ctrl Pts',(0.00208695424460772,-0.037622243702121,
-0.0100179295092302));
#33192=CARTESIAN_POINT('Ctrl Pts',(0.00200672343028683,-0.0376283958452394,
-0.00994312444017302));
#33193=CARTESIAN_POINT('Ctrl Pts',(0.00189753733051129,-0.037636145131618,
-0.00985197387956283));
#33194=CARTESIAN_POINT('Ctrl Pts',(0.00187216413263985,-0.0376379058075873,
-0.0098314845030936));
#33195=CARTESIAN_POINT('Ctrl Pts',(0.00182974225931127,-0.0376407850343264,
-0.00979835601947079));
#33196=CARTESIAN_POINT('Ctrl Pts',(0.00181288502435536,-0.0376419128484175,
-0.00978547718433662));
#33197=CARTESIAN_POINT('Ctrl Pts',(0.00177975583463052,-0.0376440982712655,
-0.00976071871862555));
#33198=CARTESIAN_POINT('Ctrl Pts',(0.00176349805428186,-0.0376451564975836,
-0.00974882208551559));
#33199=CARTESIAN_POINT('Ctrl Pts',(0.00172423940507011,-0.0376476786356387,
-0.00972069732877153));
#33200=CARTESIAN_POINT('Ctrl Pts',(0.00170112735470768,-0.0376491365779514,
-0.0097046272558229));
#33201=CARTESIAN_POINT('Ctrl Pts',(0.00162377641072108,-0.0376539310241366,
-0.00965244373114894));
#33202=CARTESIAN_POINT('Ctrl Pts',(0.00156858583977075,-0.0376572154170436,
-0.00961777103012518));
#33203=CARTESIAN_POINT('Ctrl Pts',(0.00132601850555366,-0.0376711479922775,
-0.00947618631205751));
#33204=CARTESIAN_POINT('Ctrl Pts',(0.00112855205184552,-0.0376811848038427,
-0.00938786133563327));
#33205=CARTESIAN_POINT('Ctrl Pts',(0.000839021764853071,-0.0376957123064264,
-0.00929420590120984));
#33206=CARTESIAN_POINT('Ctrl Pts',(0.000753564249706857,-0.0376999868228641,
-0.00927068746040749));
#33207=CARTESIAN_POINT('Ctrl Pts',(0.00061734691175093,-0.0377069437191662,
-0.00923961469493174));
#33208=CARTESIAN_POINT('Ctrl Pts',(0.000567217490811083,-0.0377095341475461,
-0.00922952030581138));
#33209=CARTESIAN_POINT('Ctrl Pts',(0.000499671268170587,-0.0377130934865716,
-0.00921770639638369));
#33210=CARTESIAN_POINT('Ctrl Pts',(0.000482459589042077,-0.0377140064137885,
-0.00921485056501733));
#33211=CARTESIAN_POINT('Ctrl Pts',(0.000453729411853558,-0.0377155416462878,
-0.00921034068145948));
#33212=CARTESIAN_POINT('Ctrl Pts',(0.000442224153176486,-0.0377161594717798,
-0.00920860318178661));
#33213=CARTESIAN_POINT('Ctrl Pts',(0.000418708128923782,-0.0377174289485115,
-0.00920519165008405));
#33214=CARTESIAN_POINT('Ctrl Pts',(0.000406696870285474,-0.0377180808731861,
-0.00920352344263359));
#33215=CARTESIAN_POINT('Ctrl Pts',(0.000375096833428594,-0.037719804637521,
-0.00919932973339328));
#33216=CARTESIAN_POINT('Ctrl Pts',(0.00035549295112039,-0.0377208827259958,
-0.0091969248184984));
#33217=CARTESIAN_POINT('Ctrl Pts',(0.000269027170829223,-0.0377256718604464,
-0.00918718323297989));
#33218=CARTESIAN_POINT('Ctrl Pts',(0.000201956959841878,-0.0377294759985951,
-0.00918190330559078));
#33219=CARTESIAN_POINT('Ctrl Pts',(-3.0407849027876E-5,-0.0377428396741294,
-0.00917145408906216));
#33220=CARTESIAN_POINT('Ctrl Pts',(-0.000195914849611807,-0.0377526626329514,
-0.00917769456514838));
#33221=CARTESIAN_POINT('Ctrl Pts',(-0.000470297970778056,-0.0377688102072291,
-0.00921086606483261));
#33222=CARTESIAN_POINT('Ctrl Pts',(-0.000579714920712568,-0.0377752165082834,
-0.00923030354177732));
#33223=CARTESIAN_POINT('Ctrl Pts',(-0.00075755950619684,-0.0377854921212332,
-0.00927219377045805));
#33224=CARTESIAN_POINT('Ctrl Pts',(-0.000826702041539106,-0.0377894531243794,
-0.00929111761568895));
#33225=CARTESIAN_POINT('Ctrl Pts',(-0.000922142781441596,-0.0377948723204791,
-0.00932095307942868));
#33226=CARTESIAN_POINT('Ctrl Pts',(-0.000949060428788879,-0.0377963953640786,
-0.00932978812936573));
#33227=CARTESIAN_POINT('Ctrl Pts',(-0.000995119084197374,-0.0377989929058438,
-0.00934563187099686));
#33228=CARTESIAN_POINT('Ctrl Pts',(-0.00101432089647831,-0.0378000732444643,
-0.00935245667976048));
#33229=CARTESIAN_POINT('Ctrl Pts',(-0.0010510007034363,-0.0378021324395794,
-0.00936591610863203));
#33230=CARTESIAN_POINT('Ctrl Pts',(-0.00106848908562557,-0.0378031122532645,
-0.0093725194646185));
#33231=CARTESIAN_POINT('Ctrl Pts',(-0.00111426458223233,-0.0378056722919803,
-0.00939029421720802));
#33232=CARTESIAN_POINT('Ctrl Pts',(-0.00114244588364151,-0.0378072436855356,
-0.00940173317791727));
#33233=CARTESIAN_POINT('Ctrl Pts',(-0.00124471550365131,-0.0378129337398839,
-0.00944506784794806));
#33234=CARTESIAN_POINT('Ctrl Pts',(-0.00131768583698017,-0.0378169682643452,
-0.00947952037346398));
#33235=CARTESIAN_POINT('Ctrl Pts',(-0.00156723723700532,-0.0378307971921275,
-0.00960989843765308));
#33236=CARTESIAN_POINT('Ctrl Pts',(-0.00173549288162418,-0.0378401429586102,
-0.00972056882622447));
#33237=CARTESIAN_POINT('Ctrl Pts',(-0.00198009706791911,-0.0378552118975698,
-0.00991924846681959));
#33238=CARTESIAN_POINT('Ctrl Pts',(-0.00206457454301919,-0.0378607565391,
-0.00999627135374706));
#33239=CARTESIAN_POINT('Ctrl Pts',(-0.00216422795614718,-0.0378680267272226,
-0.0100981340055179));
#33240=CARTESIAN_POINT('Ctrl Pts',(-0.00218372060427283,-0.0378694868556049,
-0.0101186308215999));
#33241=CARTESIAN_POINT('Ctrl Pts',(-0.00221236016960907,-0.0378716951686239,
-0.0101496114736076));
#33242=CARTESIAN_POINT('Ctrl Pts',(-0.00222172918579084,-0.0378724279567887,
-0.0101598887990773));
#33243=CARTESIAN_POINT('Ctrl Pts',(-0.00223850401260117,-0.037873759621071,
-0.0101785488793524));
#33244=CARTESIAN_POINT('Ctrl Pts',(-0.0022459348551604,-0.0378743566637337,
-0.0101869084087238));
#33245=CARTESIAN_POINT('Ctrl Pts',(-0.00226262538298555,-0.0378757139789977,
-0.0102058976782667));
#33246=CARTESIAN_POINT('Ctrl Pts',(-0.00227185695899828,-0.0378764761558808,
-0.01021655120047));
#33247=CARTESIAN_POINT('Ctrl Pts',(-0.00230002711983631,-0.0378788363362719,
-0.0102495271960145));
#33248=CARTESIAN_POINT('Ctrl Pts',(-0.00231871382895359,-0.0378804505703915,
-0.0102720615401041));
#33249=CARTESIAN_POINT('Ctrl Pts',(-0.00243922423081966,-0.037891165131394,
-0.0104217918058745));
#33250=CARTESIAN_POINT('Ctrl Pts',(-0.00253086451726537,-0.0379007601187622,
-0.0105568214346169));
#33251=CARTESIAN_POINT('Ctrl Pts',(-0.0026513271363398,-0.0379151398042545,
-0.0107697438117327));
#33252=CARTESIAN_POINT('Ctrl Pts',(-0.00268864846269303,-0.0379199360982675,
-0.0108424930478021));
#33253=CARTESIAN_POINT('Ctrl Pts',(-0.00277736852592235,-0.0379322019982186,
-0.0110343490997371));
#33254=CARTESIAN_POINT('Ctrl Pts',(-0.00282410316489579,-0.037939572177499,
-0.0111554341335098));
#33255=CARTESIAN_POINT('Ctrl Pts',(-0.00287497631173254,-0.0379489218076826,
-0.0113178588574153));
#33256=CARTESIAN_POINT('Ctrl Pts',(-0.00288630754296669,-0.0379511242289986,
-0.0113567853906999));
#33257=CARTESIAN_POINT('Ctrl Pts',(-0.00290279455745963,-0.0379545305932805,
-0.0114180227124528));
#33258=CARTESIAN_POINT('Ctrl Pts',(-0.0029084895529716,-0.0379557514279185,
-0.0114401821771386));
#33259=CARTESIAN_POINT('Ctrl Pts',(-0.00291866219870402,-0.0379580189776256,
-0.0114817302279686));
#33260=CARTESIAN_POINT('Ctrl Pts',(-0.00292320149540094,-0.0379590675837491,
-0.011501102300451));
#33261=CARTESIAN_POINT('Ctrl Pts',(-0.00293295352853091,-0.0379614069315476,
-0.0115446671166774));
#33262=CARTESIAN_POINT('Ctrl Pts',(-0.00293806033987555,-0.0379626942964263,
-0.0115688822261031));
#33263=CARTESIAN_POINT('Ctrl Pts',(-0.00295042051231099,-0.0379659814071533,
-0.0116313065490464));
#33264=CARTESIAN_POINT('Ctrl Pts',(-0.00295723168769888,-0.0379679674894826,
-0.0116695991348617));
#33265=CARTESIAN_POINT('Ctrl Pts',(-0.00300413471564091,-0.0379831666217663,
-0.0119666834664119));
#33266=CARTESIAN_POINT('Ctrl Pts',(-0.00301092898457304,-0.0379952659165436,
-0.0122295706366045));
#33267=CARTESIAN_POINT('Ctrl Pts',(-0.00297194724054524,-0.0380130907312578,
-0.0125997792812104));
#33268=CARTESIAN_POINT('Ctrl Pts',(-0.0029543398689143,-0.0380184595843295,
-0.0127088220121337));
#33269=CARTESIAN_POINT('Ctrl Pts',(-0.00292481886294813,-0.0380255149297125,
-0.0128438429341274));
#33270=CARTESIAN_POINT('Ctrl Pts',(-0.00291849219275542,-0.0380269531610892,
-0.0128709639012601));
#33271=CARTESIAN_POINT('Ctrl Pts',(-0.00290846198336515,-0.0380291347061286,
-0.0129114074567973));
#33272=CARTESIAN_POINT('Ctrl Pts',(-0.00290504225315914,-0.0380298631659172,
-0.012924799572219));
#33273=CARTESIAN_POINT('Ctrl Pts',(-0.00289868750565138,-0.0380311906359535,
-0.0129489870996352));
#33274=CARTESIAN_POINT('Ctrl Pts',(-0.00289578448739946,-0.0380317878778922,
-0.0129597903641244));
#33275=CARTESIAN_POINT('Ctrl Pts',(-0.00288906260805417,-0.0380331503993545,
-0.0129842582231015));
#33276=CARTESIAN_POINT('Ctrl Pts',(-0.0028852072065392,-0.0380339176522124,
-0.0129979120764626));
#33277=CARTESIAN_POINT('Ctrl Pts',(-0.00287296677832843,-0.0380363094934002,
-0.0130401143631185));
#33278=CARTESIAN_POINT('Ctrl Pts',(-0.00286425399823239,-0.0380379509200457,
-0.013068565009904));
#33279=CARTESIAN_POINT('Ctrl Pts',(-0.00280996833975091,-0.0380478133513822,
-0.0132368467884605));
#33280=CARTESIAN_POINT('Ctrl Pts',(-0.00275458874533698,-0.038056434931989,
-0.01337329385379));
#33281=CARTESIAN_POINT('Ctrl Pts',(-0.00264728509805603,-0.0380706686341365,
-0.0135903956917944));
#33282=CARTESIAN_POINT('Ctrl Pts',(-0.00260110350078717,-0.0380762629662318,
-0.0136736216504018));
#33283=CARTESIAN_POINT('Ctrl Pts',(-0.00248210666811348,-0.0380893915027212,
-0.0138659151507224));
#33284=CARTESIAN_POINT('Ctrl Pts',(-0.00240594005634628,-0.0380968430181555,
-0.0139726897951731));
#33285=CARTESIAN_POINT('Ctrl Pts',(-0.00229725377369942,-0.0381062799918662,
-0.0141056937700087));
#33286=CARTESIAN_POINT('Ctrl Pts',(-0.00227083867429439,-0.038108493388957,
-0.014136707979788));
#33287=CARTESIAN_POINT('Ctrl Pts',(-0.00222858609876653,-0.0381119127829061,
-0.0141843176970745));
#33288=CARTESIAN_POINT('Ctrl Pts',(-0.00221317673944085,-0.0381131358831869,
-0.0142012851040353));
#33289=CARTESIAN_POINT('Ctrl Pts',(-0.00218403275149779,-0.0381154055340991,
-0.0142326460906157));
#33290=CARTESIAN_POINT('Ctrl Pts',(-0.00217034654364241,-0.0381164540065879,
-0.0142470827775327));
#33291=CARTESIAN_POINT('Ctrl Pts',(-0.00213935320174369,-0.0381187903874408,
-0.0142791310866967));
#33292=CARTESIAN_POINT('Ctrl Pts',(-0.00212197009664199,-0.0381200749588172,
-0.0142966674185424));
#33293=CARTESIAN_POINT('Ctrl Pts',(-0.00207679152586123,-0.0381233496544202,
-0.0143411325998502));
#33294=CARTESIAN_POINT('Ctrl Pts',(-0.00204868754421004,-0.0381253262954874,
-0.014367742212188));
#33295=CARTESIAN_POINT('Ctrl Pts',(-0.00185590655526666,-0.0381385062048197,
-0.0145433244082964));
#33296=CARTESIAN_POINT('Ctrl Pts',(-0.00167564669943691,-0.0381489445459278,
-0.0146741576283947));
#33297=CARTESIAN_POINT('Ctrl Pts',(-0.00138759235799904,-0.0381646762826408,
-0.0148379065620802));
#33298=CARTESIAN_POINT('Ctrl Pts',(-0.00128972269425873,-0.038169890963357,
-0.0148866747598141));
#33299=CARTESIAN_POINT('Ctrl Pts',(-0.00113597550791388,-0.0381781807261722,
-0.014953072817688));
#33300=CARTESIAN_POINT('Ctrl Pts',(-0.00108187647986248,-0.0381811158805767,
-0.0149745907096343));
#33301=CARTESIAN_POINT('Ctrl Pts',(-0.00101003612252503,-0.0381850784681157,
-0.0150007710434108));
#33302=CARTESIAN_POINT('Ctrl Pts',(-0.000992826780230872,-0.038186032518885,
-0.0150068651647332));
#33303=CARTESIAN_POINT('Ctrl Pts',(-0.000964401817901725,-0.0381876178596878,
-0.015016639875531));
#33304=CARTESIAN_POINT('Ctrl Pts',(-0.00095321793925728,-0.0381882440256238,
-0.0150204121034411));
#33305=CARTESIAN_POINT('Ctrl Pts',(-0.000930697826041185,-0.0381895102537011,
-0.0150278602247926));
#33306=CARTESIAN_POINT('Ctrl Pts',(-0.00091936139598845,-0.0381901503697621,
-0.0150315347521498));
#33307=CARTESIAN_POINT('Ctrl Pts',(-0.000890097351650106,-0.0381918091841625,
-0.0150408279237655));
#33308=CARTESIAN_POINT('Ctrl Pts',(-0.000872138556095567,-0.0381928333369005,
-0.0150463458001818));
#33309=CARTESIAN_POINT('Ctrl Pts',(-0.000798881986234456,-0.0381970326494137,
-0.0150681031221734));
#33310=CARTESIAN_POINT('Ctrl Pts',(-0.000743176224571877,-0.0382002756647244,
-0.015082915349514));
#33311=CARTESIAN_POINT('Ctrl Pts',(-0.000519219071816896,-0.0382134201201707,
-0.0151356082420127));
#33312=CARTESIAN_POINT('Ctrl Pts',(-0.000348267692692032,-0.0382236699510084,
-0.0151605552173447));
#33313=CARTESIAN_POINT('Ctrl Pts',(-1.28885291828755E-5,-0.0382433151825151,
-0.0151802786561979));
#33314=CARTESIAN_POINT('Ctrl Pts',(0.000150874798862594,-0.0382526940326813,
-0.0151765176658144));
#33315=CARTESIAN_POINT('Ctrl Pts',(0.000353269772085546,-0.0382638669440909,
-0.0151552486787805));
#33316=CARTESIAN_POINT('Ctrl Pts',(0.000392920194550312,-0.0382660368777107,
-0.0151502793427568));
#33317=CARTESIAN_POINT('Ctrl Pts',(0.000454980648122617,-0.0382694046483831,
-0.0151412386768143));
#33318=CARTESIAN_POINT('Ctrl Pts',(0.000477462777156135,-0.0382706187566624,
-0.0151377019048761));
#33319=CARTESIAN_POINT('Ctrl Pts',(0.000519533418745883,-0.03827288014437,
-0.0151305920887756));
#33320=CARTESIAN_POINT('Ctrl Pts',(0.00053913071657834,-0.0382739292227878,
-0.0151270792112145));
#33321=CARTESIAN_POINT('Ctrl Pts',(0.000583173594536535,-0.0382762777493693,
-0.0151187310354264));
#33322=CARTESIAN_POINT('Ctrl Pts',(0.000607596965225421,-0.0382775736985255,
-0.0151137856993893));
#33323=CARTESIAN_POINT('Ctrl Pts',(0.000670547487576641,-0.0382808990435796,
-0.0151002206531614));
#33324=CARTESIAN_POINT('Ctrl Pts',(0.000708971722641221,-0.0382829142136489,
-0.0150911436158416));
#33325=CARTESIAN_POINT('Ctrl Pts',(0.000997947248644278,-0.0382979837337265,
-0.0150168267535087));
#33326=CARTESIAN_POINT('Ctrl Pts',(0.00123927253768217,-0.0383099566142507,
-0.0149201627607569));
#33327=CARTESIAN_POINT('Ctrl Pts',(0.00156289130452094,-0.0383277045138112,
-0.0147390358303782));
#33328=CARTESIAN_POINT('Ctrl Pts',(0.00165744085573282,-0.0383331452782901,
-0.0146789353326539));
#33329=CARTESIAN_POINT('Ctrl Pts',(0.00177117902580598,-0.038340288503813,
-0.0145973632402221));
#33330=CARTESIAN_POINT('Ctrl Pts',(0.00179372460252557,-0.0383417357548207,
-0.0145807103594571));
#33331=CARTESIAN_POINT('Ctrl Pts',(0.00182706247315057,-0.0383439283282149,
-0.0145553563306604));
#33332=CARTESIAN_POINT('Ctrl Pts',(0.00183803371714259,-0.0383446585742784,
-0.0145468918897105));
#33333=CARTESIAN_POINT('Ctrl Pts',(0.00185775475092044,-0.0383459877658143,
-0.0145314577554535));
#33334=CARTESIAN_POINT('Ctrl Pts',(0.00186652472745447,-0.0383465849160221,
-0.0145245147268607));
#33335=CARTESIAN_POINT('Ctrl Pts',(0.00188630045166375,-0.0383479452485527,
-0.0145086779308926));
#33336=CARTESIAN_POINT('Ctrl Pts',(0.00189728219272437,-0.0383487103753437,
-0.0144997552811555));
#33337=CARTESIAN_POINT('Ctrl Pts',(0.00193100401168371,-0.0383510889321497,
-0.0144719580023355));
#33338=CARTESIAN_POINT('Ctrl Pts',(0.00195352801886612,-0.0383527189442987,
-0.0144528252913142));
#33339=CARTESIAN_POINT('Ctrl Pts',(0.00208997361415517,-0.0383628301454171,
-0.014333408604781));
#33340=CARTESIAN_POINT('Ctrl Pts',(0.00219642458859821,-0.038371739263382,
-0.0142249377524926));
#33341=CARTESIAN_POINT('Ctrl Pts',(0.00235312967283044,-0.0383860349905313,
-0.0140389539007192));
#33342=CARTESIAN_POINT('Ctrl Pts',(0.00240882810348608,-0.0383914099590158,
-0.0139663591219473));
#33343=CARTESIAN_POINT('Ctrl Pts',(0.00253571217344898,-0.0384042896785454,
-0.013784323934531));
#33344=CARTESIAN_POINT('Ctrl Pts',(0.00260324776088318,-0.038411707240564,
-0.0136725568138752));
#33345=CARTESIAN_POINT('Ctrl Pts',(0.00268201036428155,-0.0384211077693719,
-0.0135206480449679));
#33346=CARTESIAN_POINT('Ctrl Pts',(0.00269998709514019,-0.0384233165952397,
-0.0134841813957939));
#33347=CARTESIAN_POINT('Ctrl Pts',(0.00272692448824798,-0.0384267305617329,
-0.0134266159918156));
#33348=CARTESIAN_POINT('Ctrl Pts',(0.00273639356015427,-0.0384279527175141,
-0.01340576175171));
#33349=CARTESIAN_POINT('Ctrl Pts',(0.00275363988920776,-0.0384302214888551,
-0.0133665938626722));
#33350=CARTESIAN_POINT('Ctrl Pts',(0.00276147552375389,-0.0384312700134707,
-0.0133483074289872));
#33351=CARTESIAN_POINT('Ctrl Pts',(0.00277863606857027,-0.0384336076164033,
-0.0133071323687479));
#33352=CARTESIAN_POINT('Ctrl Pts',(0.00278786125751644,-0.0384348933412666,
-0.0132842036009561));
#33353=CARTESIAN_POINT('Ctrl Pts',(0.00281083059315546,-0.0384381731661011,
-0.0132250124882865));
#33354=CARTESIAN_POINT('Ctrl Pts',(0.00282415708452435,-0.0384401537084813,
-0.0131885924368582));
#33355=CARTESIAN_POINT('Ctrl Pts',(0.0029087266652231,-0.0384532907482815,
-0.0129428059397929));
#33356=CARTESIAN_POINT('Ctrl Pts',(0.00295733651518357,-0.0384636897262207,
-0.01272637643387));
#33357=CARTESIAN_POINT('Ctrl Pts',(0.00299382221118458,-0.0384794029121674,
-0.0123974111947451));
#33358=CARTESIAN_POINT('Ctrl Pts',(0.00299992494541448,-0.0384846421759763,
-0.0122876885680689));
#33359=CARTESIAN_POINT('Ctrl Pts',(0.00300003817796209,-0.0384929168377875,
-0.0121204987763927));
#33360=CARTESIAN_POINT('Ctrl Pts',(0.00299843043573469,-0.038495809124339,
-0.012063126393098));
#33361=CARTESIAN_POINT('Ctrl Pts',(0.00299411551288363,-0.0384997512260852,
-0.0119871095017452));
#33362=CARTESIAN_POINT('Ctrl Pts',(0.00299287675335369,-0.0385007308112597,
-0.0119683909390974));
#33363=CARTESIAN_POINT('Ctrl Pts',(0.00299056458162604,-0.0385023475237244,
-0.0119378084189421));
#33364=CARTESIAN_POINT('Ctrl Pts',(0.00298959589558238,-0.0385029791164709,
-0.0119259368058963));
#33365=CARTESIAN_POINT('Ctrl Pts',(0.00298752611668686,-0.0385042447654798,
-0.0119023077716062));
#33366=CARTESIAN_POINT('Ctrl Pts',(0.00298642624939588,-0.0385048787493831,
-0.0118905504776998));
#33367=CARTESIAN_POINT('Ctrl Pts',(0.00298344667560644,-0.038506503615628,
-0.0118606070286782));
#33368=CARTESIAN_POINT('Ctrl Pts',(0.00298147010031703,-0.0385074995524286,
-0.0118424312156196));
#33369=CARTESIAN_POINT('Ctrl Pts',(0.00297247650210088,-0.038511712887228,
-0.0117662180915147));
#33370=CARTESIAN_POINT('Ctrl Pts',(0.00296393030013996,-0.0385150012420553,
-0.0117083772068289));
#33371=CARTESIAN_POINT('Ctrl Pts',(0.0029344403410876,-0.0385246272079108,
-0.0115424722609411));
#33372=CARTESIAN_POINT('Ctrl Pts',(0.00290923312333203,-0.0385310845282925,
-0.0114352641599816));
#33373=CARTESIAN_POINT('Ctrl Pts',(0.00281593822788839,-0.0385505263554746,
-0.0111179254418827));
#33374=CARTESIAN_POINT('Ctrl Pts',(0.00273049172443464,-0.0385634283098509,
-0.0109136482570906));
#33375=CARTESIAN_POINT('Ctrl Pts',(0.00260456342050484,-0.0385777217191394,
-0.0106866401861755));
#33376=CARTESIAN_POINT('Ctrl Pts',(0.0025850793150576,-0.0385798365196836,
-0.010653069193299));
#33377=CARTESIAN_POINT('Ctrl Pts',(0.0025521255816362,-0.0385832611598833,
-0.0105987463552682));
#33378=CARTESIAN_POINT('Ctrl Pts',(0.00253904146004677,-0.0385845844127943,
-0.0105777670026649));
#33379=CARTESIAN_POINT('Ctrl Pts',(0.00251496343622294,-0.0385869555834838,
-0.010540202129362));
#33380=CARTESIAN_POINT('Ctrl Pts',(0.00250406114513512,-0.0385880067320656,
-0.0105235598500129));
#33381=CARTESIAN_POINT('Ctrl Pts',(0.00248025784800593,-0.0385902546063497,
-0.0104880010413813));
#33382=CARTESIAN_POINT('Ctrl Pts',(0.00246730415786335,-0.0385914493041666,
-0.010469121197277));
#33383=CARTESIAN_POINT('Ctrl Pts',(0.00243077399012196,-0.0385947417312756,
-0.0104171641161299));
#33384=CARTESIAN_POINT('Ctrl Pts',(0.00240673957702643,-0.0385968222861442,
-0.0103844140338685));
#33385=CARTESIAN_POINT('Ctrl Pts',(0.00230289525315512,-0.0386054758775297,
-0.0102487759939204));
#33386=CARTESIAN_POINT('Ctrl Pts',(0.00221709284449092,-0.0386118197773989,
-0.0101506478682194));
#33387=CARTESIAN_POINT('Ctrl Pts',(0.00206224495969223,-0.0386223217727025,
-0.00999523494514102));
#33388=CARTESIAN_POINT('Ctrl Pts',(0.00199652444888733,-0.0386265354076054,
-0.00993490683747034));
#33389=CARTESIAN_POINT('Ctrl Pts',(0.00181013109120773,-0.0386380794596843,
-0.00977852475355941));
#33390=CARTESIAN_POINT('Ctrl Pts',(0.00168459870079932,-0.0386454212204768,
-0.00968871096250319));
#33391=CARTESIAN_POINT('Ctrl Pts',(0.00152732877733873,-0.0386547814237194,
-0.00959357742562413));
#33392=CARTESIAN_POINT('Ctrl Pts',(0.00150169444234515,-0.0386563121970781,
-0.00957858635902542));
#33393=CARTESIAN_POINT('Ctrl Pts',(0.00146350008988871,-0.0386586066976584,
-0.0095570045953262));
#33394=CARTESIAN_POINT('Ctrl Pts',(0.00145110840548118,-0.0386593532160095,
-0.00955011808274345));
#33395=CARTESIAN_POINT('Ctrl Pts',(0.00142885222449578,-0.0386606985661463,
-0.00953795517227716));
#33396=CARTESIAN_POINT('Ctrl Pts',(0.00141900638169355,-0.038661295359854,
-0.0095326457611751));
#33397=CARTESIAN_POINT('Ctrl Pts',(0.00139691971816581,-0.0386626378407869,
-0.0095208944121656));
#33398=CARTESIAN_POINT('Ctrl Pts',(0.00138466400744241,-0.0386633852294527,
-0.00951448204312785));
#33399=CARTESIAN_POINT('Ctrl Pts',(0.00134755456317872,-0.0386656546466079,
-0.0094953915466785));
#33400=CARTESIAN_POINT('Ctrl Pts',(0.0013225685018813,-0.038667191223888,
-0.00948297547858484));
#33401=CARTESIAN_POINT('Ctrl Pts',(0.00119748217814813,-0.0386749126413374,
-0.00942297838613298));
#33402=CARTESIAN_POINT('Ctrl Pts',(0.00109497828094512,-0.0386813284494651,
-0.00938062474162731));
#33403=CARTESIAN_POINT('Ctrl Pts',(0.000744042790804974,-0.0387030860675511,
-0.00925789132101391));
#33404=CARTESIAN_POINT('Ctrl Pts',(0.000487470579661229,-0.0387185349053377,
-0.00920423463305956));
#33405=CARTESIAN_POINT('Ctrl Pts',(0.00018822610378376,-0.0387350628504217,
-0.00918150917919925));
#33406=CARTESIAN_POINT('Ctrl Pts',(0.000149222848675907,-0.0387371916534693,
-0.0091793122081576));
#33407=CARTESIAN_POINT('Ctrl Pts',(8.54070832880134E-5,-0.0387406340826542,
-0.00917696674648536));
#33408=CARTESIAN_POINT('Ctrl Pts',(6.06168239286941E-5,-0.0387419613584356,
-0.00917636324646113));
#33409=CARTESIAN_POINT('Ctrl Pts',(1.59234775696302E-5,-0.0387443368416078,
-0.00917582954878122));
#33410=CARTESIAN_POINT('Ctrl Pts',(-3.97663950225589E-6,-0.0387453883316623,
-0.00917578992119837));
#33411=CARTESIAN_POINT('Ctrl Pts',(-4.67173719602617E-5,-0.0387476338483137,
-0.00917613009128741));
#33412=CARTESIAN_POINT('Ctrl Pts',(-6.95563115034423E-5,-0.038748825887186,
-0.00917657275312798));
#33413=CARTESIAN_POINT('Ctrl Pts',(-0.000132732048396999,-0.0387521027168052,
-0.00917851924458077));
#33414=CARTESIAN_POINT('Ctrl Pts',(-0.000173047625683019,-0.0387541706077786,
-0.00918057635945556));
#33415=CARTESIAN_POINT('Ctrl Pts',(-0.000406993128765488,-0.0387660547152393,
-0.00919725292670068));
#33416=CARTESIAN_POINT('Ctrl Pts',(-0.000598880785348187,-0.0387753021225477,
-0.00922982987934081));
#33417=CARTESIAN_POINT('Ctrl Pts',(-0.000962051909960035,-0.0387931437202054,
-0.00932846365032878));
#33418=CARTESIAN_POINT('Ctrl Pts',(-0.00113308553822213,-0.0388017195433591,
-0.00939210132974085));
#33419=CARTESIAN_POINT('Ctrl Pts',(-0.00132277308792866,-0.0388124524766794,
-0.00948307198145786));
#33420=CARTESIAN_POINT('Ctrl Pts',(-0.00134809790753585,-0.0388139123763085,
-0.00949566080804657));
#33421=CARTESIAN_POINT('Ctrl Pts',(-0.00138560366985646,-0.038816120403891,
-0.0095149707550036));
#33422=CARTESIAN_POINT('Ctrl Pts',(-0.00139792260213483,-0.0388168531407309,
-0.00952142194251254));
#33423=CARTESIAN_POINT('Ctrl Pts',(-0.00142006828334926,-0.0388181847446295,
-0.00953321612340705));
#33424=CARTESIAN_POINT('Ctrl Pts',(-0.00142991060176433,-0.0388187817788467,
-0.0095385287392919));
#33425=CARTESIAN_POINT('Ctrl Pts',(-0.00145209104366136,-0.038820139114881,
-0.00955066180060661));
#33426=CARTESIAN_POINT('Ctrl Pts',(-0.00146441088651729,-0.038820901321531,
-0.00955751421822301));
#33427=CARTESIAN_POINT('Ctrl Pts',(-0.00150216668415699,-0.0388232617255935,
-0.00957886418071039));
#33428=CARTESIAN_POINT('Ctrl Pts',(-0.00152743840433289,-0.0388248761584615,
-0.00959364706722501));
#33429=CARTESIAN_POINT('Ctrl Pts',(-0.00165807674838472,-0.0388333870204492,
-0.00967265373142536));
#33430=CARTESIAN_POINT('Ctrl Pts',(-0.00175961675864719,-0.0388405657251032,
-0.00974295978235645));
#33431=CARTESIAN_POINT('Ctrl Pts',(-0.00203544054951817,-0.0388611635934932,
-0.0099602593015319));
#33432=CARTESIAN_POINT('Ctrl Pts',(-0.00219774383051521,-0.0388745971795189,
-0.0101211456020383));
#33433=CARTESIAN_POINT('Ctrl Pts',(-0.00237422535755924,-0.0388902799717701,
-0.0103411878523124));
#33434=CARTESIAN_POINT('Ctrl Pts',(-0.00240701601816053,-0.0388932544580106,
-0.0103844243298767));
#33435=CARTESIAN_POINT('Ctrl Pts',(-0.00245354594362036,-0.0388975687565241,
-0.0104493628472223));
#33436=CARTESIAN_POINT('Ctrl Pts',(-0.00246820703516177,-0.0388989429010993,
-0.0104703882411029));
#33437=CARTESIAN_POINT('Ctrl Pts',(-0.00249384189615975,-0.0389013729704397,
-0.0105081741320989));
#33438=CARTESIAN_POINT('Ctrl Pts',(-0.00250492050365629,-0.0389024327386065,
-0.0105248613236326));
#33439=CARTESIAN_POINT('Ctrl Pts',(-0.00252785961587549,-0.0389046479843788,
-0.0105601759248636));
#33440=CARTESIAN_POINT('Ctrl Pts',(-0.0025396832775329,-0.0389058020775142,
-0.0105788259046472));
#33441=CARTESIAN_POINT('Ctrl Pts',(-0.00257062713357922,-0.0389088568147299,
-0.0106288478617212));
#33442=CARTESIAN_POINT('Ctrl Pts',(-0.00258937907631898,-0.0389107442689742,
-0.0106604438395106));
#33443=CARTESIAN_POINT('Ctrl Pts',(-0.00271078419993422,-0.0389232303810811,
-0.0108738409426379));
#33444=CARTESIAN_POINT('Ctrl Pts',(-0.00279479958166486,-0.0389331454946652,
-0.011065586539442));
#33445=CARTESIAN_POINT('Ctrl Pts',(-0.00291087670828539,-0.0389512600979821,
-0.0114296402026054));
#33446=CARTESIAN_POINT('Ctrl Pts',(-0.00294911221939567,-0.0389594500161003,
-0.0115989978677757));
#33447=CARTESIAN_POINT('Ctrl Pts',(-0.00297640784128063,-0.0389697537799309,
-0.0117992533425694));
#33448=CARTESIAN_POINT('Ctrl Pts',(-0.00297988934446562,-0.0389712412015348,
-0.011827872633229));
#33449=CARTESIAN_POINT('Ctrl Pts',(-0.00298444918056285,-0.0389734828493506,
-0.0118704692173335));
#33450=CARTESIAN_POINT('Ctrl Pts',(-0.00298584296106661,-0.0389742209904355,
-0.0118844118039434));
#33451=CARTESIAN_POINT('Ctrl Pts',(-0.00298817358054488,-0.0389755579552331,
-0.0119095005871635));
#33452=CARTESIAN_POINT('Ctrl Pts',(-0.00298914582883364,-0.0389761548658353,
-0.0119206429542594));
#33453=CARTESIAN_POINT('Ctrl Pts',(-0.00299119399647987,-0.0389775062239053,
-0.0119457354316928));
#33454=CARTESIAN_POINT('Ctrl Pts',(-0.00299223464617144,-0.0389782624945639,
-0.0119596877050776));
#33455=CARTESIAN_POINT('Ctrl Pts',(-0.00299511325906131,-0.0389805859756623,
-0.0120022985324384));
#33456=CARTESIAN_POINT('Ctrl Pts',(-0.00299663730093455,-0.038982168723352,
-0.0120309759044117));
#33457=CARTESIAN_POINT('Ctrl Pts',(-0.00300232497431783,-0.038990350493258,
-0.0121777282662941));
#33458=CARTESIAN_POINT('Ctrl Pts',(-0.00299992206141389,-0.0389972098103454,
-0.0122959456158238));
#33459=CARTESIAN_POINT('Ctrl Pts',(-0.00297374028262983,-0.0390165642481569,
-0.0126251368941267));
#33460=CARTESIAN_POINT('Ctrl Pts',(-0.00293454618453088,-0.0390291041056367,
-0.0128342183540017));
#33461=CARTESIAN_POINT('Ctrl Pts',(-0.00285381195661623,-0.039044899389337,
-0.0131034923703898));
#33462=CARTESIAN_POINT('Ctrl Pts',(-0.00283173084692017,-0.0390487104256614,
-0.0131688580216957));
#33463=CARTESIAN_POINT('Ctrl Pts',(-0.00279732358097167,-0.0390540021401096,
-0.0132601965120349));
#33464=CARTESIAN_POINT('Ctrl Pts',(-0.0027868492676536,-0.0390555416770672,
-0.0132868396426793));
#33465=CARTESIAN_POINT('Ctrl Pts',(-0.00276832514389438,-0.0390581477582604,
-0.0133320475137219));
#33466=CARTESIAN_POINT('Ctrl Pts',(-0.00276046607754844,-0.0390592204936834,
-0.0133506878514358));
#33467=CARTESIAN_POINT('Ctrl Pts',(-0.00274403413157239,-0.0390613982542113,
-0.0133885861381884));
#33468=CARTESIAN_POINT('Ctrl Pts',(-0.0027354456072213,-0.0390625026825667,
-0.0134078360966683));
#33469=CARTESIAN_POINT('Ctrl Pts',(-0.00271332968509638,-0.0390652644042006,
-0.0134560340897733));
#33470=CARTESIAN_POINT('Ctrl Pts',(-0.00269954122029,-0.0390669128358835,
-0.0134848598443316));
#33471=CARTESIAN_POINT('Ctrl Pts',(-0.0026396470821944,-0.0390737813662494,
-0.0136050994738884));
#33472=CARTESIAN_POINT('Ctrl Pts',(-0.00258933654992385,-0.039078857944528,
-0.0136943460116615));
#33473=CARTESIAN_POINT('Ctrl Pts',(-0.00241999263689838,-0.0390942384668816,
-0.0139617680625989));
#33474=CARTESIAN_POINT('Ctrl Pts',(-0.00228639399007479,-0.0391041170316073,
-0.0141298882182757));
#33475=CARTESIAN_POINT('Ctrl Pts',(-0.00207441824598657,-0.0391187646997157,
-0.014344837198527));
#33476=CARTESIAN_POINT('Ctrl Pts',(-0.00201008653344285,-0.0391231087231494,
-0.0144045865696192));
#33477=CARTESIAN_POINT('Ctrl Pts',(-0.0019270058287337,-0.0391287296770877,
-0.0144752232587987));
#33478=CARTESIAN_POINT('Ctrl Pts',(-0.00191063143912187,-0.0391298380409864,
-0.0144888472744108));
#33479=CARTESIAN_POINT('Ctrl Pts',(-0.00188444792794975,-0.0391316136790795,
-0.0145101650411146));
#33480=CARTESIAN_POINT('Ctrl Pts',(-0.00187473326568934,-0.0391322731882558,
-0.0145179742339421));
#33481=CARTESIAN_POINT('Ctrl Pts',(-0.00185600428031605,-0.0391335466151013,
-0.0145328384666745));
#33482=CARTESIAN_POINT('Ctrl Pts',(-0.0018469978403904,-0.039134159890283,
-0.0145399027762784));
#33483=CARTESIAN_POINT('Ctrl Pts',(-0.00182495514277333,-0.0391356626648682,
-0.0145569893848625));
#33484=CARTESIAN_POINT('Ctrl Pts',(-0.00181187656359613,-0.0391365558177641,
-0.0145669563135732));
#33485=CARTESIAN_POINT('Ctrl Pts',(-0.00176388642718363,-0.0391398365684443,
-0.0146029088547011));
#33486=CARTESIAN_POINT('Ctrl Pts',(-0.00172849383643636,-0.0391422626399744,
-0.0146282404378204));
#33487=CARTESIAN_POINT('Ctrl Pts',(-0.00163519224018046,-0.0391486490110194,
-0.0146919961484998));
#33488=CARTESIAN_POINT('Ctrl Pts',(-0.00157647771028428,-0.0391526586969372,
-0.0147291933836279));
#33489=CARTESIAN_POINT('Ctrl Pts',(-0.00140528564537905,-0.0391642196998403,
-0.0148294913241597));
#33490=CARTESIAN_POINT('Ctrl Pts',(-0.0012899578316361,-0.0391718488368925,
-0.0148874269556516));
#33491=CARTESIAN_POINT('Ctrl Pts',(-0.00102070520665153,-0.0391889279319041,
-0.0150016105366168));
#33492=CARTESIAN_POINT('Ctrl Pts',(-0.000865166701356852,-0.0391982789183774,
-0.0150530467161435));
#33493=CARTESIAN_POINT('Ctrl Pts',(-0.00067097495634809,-0.0392092081008345,
-0.0151000806411456));
#33494=CARTESIAN_POINT('Ctrl Pts',(-0.000635605052469569,-0.0392111705041494,
-0.0151079718697894));
#33495=CARTESIAN_POINT('Ctrl Pts',(-0.000578570366755936,-0.0392142907984768,
-0.0151196160429682));
#33496=CARTESIAN_POINT('Ctrl Pts',(-0.000556992945057825,-0.0392154612242389,
-0.0151237748813571));
#33497=CARTESIAN_POINT('Ctrl Pts',(-0.000515638383835819,-0.0392176857541131,
-0.0151312752965544));
#33498=CARTESIAN_POINT('Ctrl Pts',(-0.000495869688292898,-0.0392187410324173,
-0.0151346563347835));
#33499=CARTESIAN_POINT('Ctrl Pts',(-0.000450122735577565,-0.039221164972726,
-0.0151420090617193));
#33500=CARTESIAN_POINT('Ctrl Pts',(-0.000424123045263789,-0.0392225291600631,
-0.0151458381785259));
#33501=CARTESIAN_POINT('Ctrl Pts',(-0.000340076528525251,-0.0392268982572724,
-0.0151570899707118));
#33502=CARTESIAN_POINT('Ctrl Pts',(-0.00028186034272584,-0.0392298617549315,
-0.0151631563377064));
#33503=CARTESIAN_POINT('Ctrl Pts',(-0.000141124136975081,-0.0392369031773296,
-0.0151736704707532));
#33504=CARTESIAN_POINT('Ctrl Pts',(-5.85247863529789E-5,-0.0392409340142681,
-0.0151764198772384));
#33505=CARTESIAN_POINT('Ctrl Pts',(0.000145908966180293,-0.0392507765552011,
-0.015174778479957));
#33506=CARTESIAN_POINT('Ctrl Pts',(0.000267560614603388,-0.0392565132968298,
-0.0151663805902251));
#33507=CARTESIAN_POINT('Ctrl Pts',(0.000527771718355039,-0.0392689839189267,
-0.0151324091744021));
#33508=CARTESIAN_POINT('Ctrl Pts',(0.000665715536189162,-0.0392757203222382,
-0.0151044333918121));
#33509=CARTESIAN_POINT('Ctrl Pts',(0.000829825185483897,-0.0392843921204166,
-0.0150589547412073));
#33510=CARTESIAN_POINT('Ctrl Pts',(0.000858354197409255,-0.0392859245929285,
-0.0150505901062668));
#33511=CARTESIAN_POINT('Ctrl Pts',(0.000900301656824832,-0.0392882211165156,
-0.0150376111487432));
#33512=CARTESIAN_POINT('Ctrl Pts',(0.000913819996949949,-0.039288967910889,
-0.0150333231696109));
#33513=CARTESIAN_POINT('Ctrl Pts',(0.0009379450740193,-0.0392903134851821,
-0.0150254820619961));
#33514=CARTESIAN_POINT('Ctrl Pts',(0.000948563046926292,-0.0392909102220226,
-0.0150219652412202));
#33515=CARTESIAN_POINT('Ctrl Pts',(0.000972259805630739,-0.039292252215025,
-0.0150139692066333));
#33516=CARTESIAN_POINT('Ctrl Pts',(0.000985327335711489,-0.0392929991675005,
-0.0150094589634474));
#33517=CARTESIAN_POINT('Ctrl Pts',(0.00102463790398862,-0.0392952660846629,
-0.014995586166974));
#33518=CARTESIAN_POINT('Ctrl Pts',(0.00105078148140545,-0.0392968005553837,
-0.0149859483954579));
#33519=CARTESIAN_POINT('Ctrl Pts',(0.0011799303674384,-0.0393045015598309,
-0.0149362837497199));
#33520=CARTESIAN_POINT('Ctrl Pts',(0.00128079683873615,-0.0393108978285933,
-0.0148909532409753));
#33521=CARTESIAN_POINT('Ctrl Pts',(0.001611300749046,-0.0393326757371569,
-0.0147198998180659));
#33522=CARTESIAN_POINT('Ctrl Pts',(0.00182699172161334,-0.0393481677114533,
-0.0145697220746977));
#33523=CARTESIAN_POINT('Ctrl Pts',(0.00204924915412847,-0.0393647249737159,
-0.0143672213436977));
#33524=CARTESIAN_POINT('Ctrl Pts',(0.00207751856400366,-0.0393668468467883,
-0.0143404393591483));
#33525=CARTESIAN_POINT('Ctrl Pts',(0.00212289938237204,-0.0393702804875151,
-0.0142957380223536));
#33526=CARTESIAN_POINT('Ctrl Pts',(0.00214032378805177,-0.0393716057876214,
-0.0142781442304326));
#33527=CARTESIAN_POINT('Ctrl Pts',(0.00217135386096708,-0.0393739791661016,
-0.0142460267837763));
#33528=CARTESIAN_POINT('Ctrl Pts',(0.00218503649062956,-0.0393750305014769,
-0.0142315797903034));
#33529=CARTESIAN_POINT('Ctrl Pts',(0.00221413398877599,-0.0393772772141166,
-0.0142002380458476));
#33530=CARTESIAN_POINT('Ctrl Pts',(0.00222950150161526,-0.0393784705838083,
-0.014183300936165));
#33531=CARTESIAN_POINT('Ctrl Pts',(0.00227153637598166,-0.0393817551613423,
-0.0141358945749736));
#33532=CARTESIAN_POINT('Ctrl Pts',(0.00229778330847261,-0.0393838293344136,
-0.0141050581548049));
#33533=CARTESIAN_POINT('Ctrl Pts',(0.00245209062998006,-0.0393961873073987,
-0.0139161505622354));
#33534=CARTESIAN_POINT('Ctrl Pts',(0.00256442601590134,-0.0394058396432739,
-0.01374592050761));
#33535=CARTESIAN_POINT('Ctrl Pts',(0.00273815972245396,-0.0394236191171213,
-0.0134135610356391));
#33536=CARTESIAN_POINT('Ctrl Pts',(0.00280444514595227,-0.0394317328632308,
-0.0132549801383261));
#33537=CARTESIAN_POINT('Ctrl Pts',(0.00286564618576958,-0.0394419526798934,
-0.0130640592459295));
#33538=CARTESIAN_POINT('Ctrl Pts',(0.00287408252761063,-0.0394434459431049,
-0.0130363690600189));
#33539=CARTESIAN_POINT('Ctrl Pts',(0.00288601241832093,-0.0394456947683726,
-0.0129950781136299));
#33540=CARTESIAN_POINT('Ctrl Pts',(0.00288981350310425,-0.0394464340991057,
-0.0129815671923847));
#33541=CARTESIAN_POINT('Ctrl Pts',(0.00289647407954364,-0.0394477724375182,
-0.0129572386566017));
#33542=CARTESIAN_POINT('Ctrl Pts',(0.00289936805307299,-0.0394483695172106,
-0.0129464310403337));
#33543=CARTESIAN_POINT('Ctrl Pts',(0.00290574146158099,-0.0394497203007062,
-0.01292208511333));
#33544=CARTESIAN_POINT('Ctrl Pts',(0.00290918675807305,-0.039450475814798,
-0.012908538602502));
#33545=CARTESIAN_POINT('Ctrl Pts',(0.00291939934681311,-0.0394527935443473,
-0.0128671759216941));
#33546=CARTESIAN_POINT('Ctrl Pts',(0.00292586308743801,-0.0394543711750504,
-0.0128392872385315));
#33547=CARTESIAN_POINT('Ctrl Pts',(0.00295676936123018,-0.0394624987347242,
-0.0126966894374659));
#33548=CARTESIAN_POINT('Ctrl Pts',(0.00297486741668729,-0.0394693052259971,
-0.0125807175142311));
#33549=CARTESIAN_POINT('Ctrl Pts',(0.00300626841307121,-0.0394884620701573,
-0.0122552952313297));
#33550=CARTESIAN_POINT('Ctrl Pts',(0.00300447414339993,-0.0395008608299876,
-0.0120450340041819));
#33551=CARTESIAN_POINT('Ctrl Pts',(0.00297270405076887,-0.0395166729678301,
-0.0117658380842074));
#33552=CARTESIAN_POINT('Ctrl Pts',(0.00296212176763812,-0.0395206163921595,
-0.0116953144040078));
#33553=CARTESIAN_POINT('Ctrl Pts',(0.00294370913985941,-0.0395260580939518,
-0.0115966996928226));
#33554=CARTESIAN_POINT('Ctrl Pts',(0.00293796819512319,-0.0395276196805869,
-0.0115682470409497));
#33555=CARTESIAN_POINT('Ctrl Pts',(0.00292751073052948,-0.0395302518617929,
-0.0115200383741477));
#33556=CARTESIAN_POINT('Ctrl Pts',(0.00292300493616394,-0.0395313289461742,
-0.0115002391607041));
#33557=CARTESIAN_POINT('Ctrl Pts',(0.00291343451724971,-0.0395335063590285,
-0.0114600742373949));
#33558=CARTESIAN_POINT('Ctrl Pts',(0.00290835651715466,-0.0395346061986208,
-0.0114397128569683));
#33559=CARTESIAN_POINT('Ctrl Pts',(0.0028951308664012,-0.0395373387166609,
-0.0113889559416659));
#33560=CARTESIAN_POINT('Ctrl Pts',(0.00288671774743782,-0.0395389629419467,
-0.011358631831447));
#33561=CARTESIAN_POINT('Ctrl Pts',(0.00285030885504014,-0.0395455574706666,
-0.0112349859373537));
#33562=CARTESIAN_POINT('Ctrl Pts',(0.00281825126161172,-0.0395503989741523,
-0.011142918631392));
#33563=CARTESIAN_POINT('Ctrl Pts',(0.00271851747211837,-0.0395633735513514,
-0.0108959320556279));
#33564=CARTESIAN_POINT('Ctrl Pts',(0.00264215149722873,-0.0395712782327611,
-0.0107449193280151));
#33565=CARTESIAN_POINT('Ctrl Pts',(0.00248193095408904,-0.0395858265197355,
-0.0104851141351942));
#33566=CARTESIAN_POINT('Ctrl Pts',(0.00240256396271854,-0.0395924094033827,
-0.010374115438874));
#33567=CARTESIAN_POINT('Ctrl Pts',(0.00230163406931255,-0.0396005745914476,
-0.0102515386359574));
#33568=CARTESIAN_POINT('Ctrl Pts',(0.00228713723402088,-0.039601743072216,
-0.010234330822341));
#33569=CARTESIAN_POINT('Ctrl Pts',(0.00226405701431732,-0.039603599607838,
-0.0102075517207339));
#33570=CARTESIAN_POINT('Ctrl Pts',(0.00225560306191441,-0.0396042788539704,
-0.0101978694561736));
#33571=CARTESIAN_POINT('Ctrl Pts',(0.00223959729801393,-0.0396055640606734,
-0.010179774193298));
#33572=CARTESIAN_POINT('Ctrl Pts',(0.00223205981432771,-0.0396061690273814,
-0.0101713491647288));
#33573=CARTESIAN_POINT('Ctrl Pts',(0.00221402705030322,-0.0396076154805386,
-0.0101514208487962));
#33574=CARTESIAN_POINT('Ctrl Pts',(0.00220348958532341,-0.0396084599764574,
-0.0101399564077591));
#33575=CARTESIAN_POINT('Ctrl Pts',(0.00216708456251237,-0.0396113734112116,
-0.0101009625689168));
#33576=CARTESIAN_POINT('Ctrl Pts',(0.0021407874339902,-0.0396134708419514,
-0.0100738409414576));
#33577=CARTESIAN_POINT('Ctrl Pts',(0.00207371457127198,-0.0396187866753922,
-0.010007229462345));
#33578=CARTESIAN_POINT('Ctrl Pts',(0.00203231757378688,-0.0396220375036569,
-0.00996838729685674));
#33579=CARTESIAN_POINT('Ctrl Pts',(0.00181272409183881,-0.0396390244275337,
-0.00977376100081102));
#33580=CARTESIAN_POINT('Ctrl Pts',(0.00161762034693136,-0.0396531882096877,
-0.009638267884226));
#33581=CARTESIAN_POINT('Ctrl Pts',(0.00133189107574234,-0.0396715664798037,
-0.00948631457592746));
#33582=CARTESIAN_POINT('Ctrl Pts',(0.00125342120706623,-0.0396764068472325,
-0.00944886050546996));
#33583=CARTESIAN_POINT('Ctrl Pts',(0.00114474767397187,-0.0396828294802495,
-0.00940267387661836));
#33584=CARTESIAN_POINT('Ctrl Pts',(0.00111587640407197,-0.0396845099174429,
-0.00939093116434264));
#33585=CARTESIAN_POINT('Ctrl Pts',(0.00106928810481684,-0.0396871811612268,
-0.0093728233155729));
#33586=CARTESIAN_POINT('Ctrl Pts',(0.00105168556853572,-0.039688181322305,
-0.0093661715330512));
#33587=CARTESIAN_POINT('Ctrl Pts',(0.0010150080638223,-0.0396902468043696,
-0.00935270453531472));
#33588=CARTESIAN_POINT('Ctrl Pts',(0.000995924280322381,-0.0396913112129239,
-0.00934591599117993));
#33589=CARTESIAN_POINT('Ctrl Pts',(0.000950597863230456,-0.0396938157262249,
-0.00933030763103566));
#33590=CARTESIAN_POINT('Ctrl Pts',(0.000924298793233889,-0.0396952503187625,
-0.00932165669526648));
#33591=CARTESIAN_POINT('Ctrl Pts',(0.000833605375945967,-0.0397001372874357,
-0.00929320862828096));
#33592=CARTESIAN_POINT('Ctrl Pts',(0.000768664168127061,-0.0397035325723301,
-0.00927521639528295));
#33593=CARTESIAN_POINT('Ctrl Pts',(0.000604795754938369,-0.0397118893254924,
-0.00923570669867853));
#33594=CARTESIAN_POINT('Ctrl Pts',(0.000505281739059318,-0.0397167742408331,
-0.00921697986296786));
#33595=CARTESIAN_POINT('Ctrl Pts',(0.000211278876579293,-0.0397309347067533,
-0.00917692201730842));
#33596=CARTESIAN_POINT('Ctrl Pts',(1.54489283979635E-5,-0.0397400035473488,
-0.00916953023161437));
#33597=CARTESIAN_POINT('Ctrl Pts',(-0.000234939306648998,-0.0397524382447527,
-0.00918455477104413));
#33598=CARTESIAN_POINT('Ctrl Pts',(-0.000290081535653657,-0.0397552314741943,
-0.00918939797984695));
#33599=CARTESIAN_POINT('Ctrl Pts',(-0.000363445185181044,-0.0397590569618281,
-0.00919789251939113));
#33600=CARTESIAN_POINT('Ctrl Pts',(-0.000381814833243012,-0.0397600240287658,
-0.00920019199310643));
#33601=CARTESIAN_POINT('Ctrl Pts',(-0.00041074397304167,-0.039761563132472,
-0.00920408556273013));
#33602=CARTESIAN_POINT('Ctrl Pts',(-0.000421318531893806,-0.0397621291344292,
-0.0092055663133028));
#33603=CARTESIAN_POINT('Ctrl Pts',(-0.000443353371492702,-0.0397633160708654,
-0.0092087718755136));
#33604=CARTESIAN_POINT('Ctrl Pts',(-0.000454811848787681,-0.0397639375868941,
-0.00921050668293932));
#33605=CARTESIAN_POINT('Ctrl Pts',(-0.00048327371581384,-0.0397654915894961,
-0.00921498463737923));
#33606=CARTESIAN_POINT('Ctrl Pts',(-0.000500263966787123,-0.0397664283187391,
-0.00921780788834041));
#33607=CARTESIAN_POINT('Ctrl Pts',(-0.000565834052410495,-0.039770076043224,
-0.00922928465586122));
#33608=CARTESIAN_POINT('Ctrl Pts',(-0.000614219683179988,-0.0397728370995543,
-0.00923898956491019));
#33609=CARTESIAN_POINT('Ctrl Pts',(-0.000744113699894974,-0.0397803982986722,
-0.00926839319478653));
#33610=CARTESIAN_POINT('Ctrl Pts',(-0.000825070500280015,-0.0397852702984067,
-0.00929032271465621));
#33611=CARTESIAN_POINT('Ctrl Pts',(-0.00109410228534698,-0.0398017949266034,
-0.00937544606675465));
#33612=CARTESIAN_POINT('Ctrl Pts',(-0.00127682639303939,-0.0398135420009456,
-0.00945389296504211));
#33613=CARTESIAN_POINT('Ctrl Pts',(-0.00152376337572712,-0.0398295349814844,
-0.00959028664832621));
#33614=CARTESIAN_POINT('Ctrl Pts',(-0.00159532836875495,-0.0398341922533159,
-0.00963381888695232));
#33615=CARTESIAN_POINT('Ctrl Pts',(-0.00169062013624761,-0.0398404204088989,
-0.00969739542851158));
#33616=CARTESIAN_POINT('Ctrl Pts',(-0.00171599241279145,-0.0398420816261606,
-0.00971489413730863));
#33617=CARTESIAN_POINT('Ctrl Pts',(-0.00175637707271845,-0.0398447312993771,
-0.00974367485790911));
#33618=CARTESIAN_POINT('Ctrl Pts',(-0.00177156058830689,-0.0398457288010343,
-0.00975471193714494));
#33619=CARTESIAN_POINT('Ctrl Pts',(-0.00180297103271198,-0.0398477954422173,
-0.00977799825500174));
#33620=CARTESIAN_POINT('Ctrl Pts',(-0.00181917907705367,-0.0398488635967568,
-0.00979027142678888));
#33621=CARTESIAN_POINT('Ctrl Pts',(-0.00185742377422857,-0.0398513889086865,
-0.00981984780132442));
#33622=CARTESIAN_POINT('Ctrl Pts',(-0.00187934544332701,-0.0398528403243052,
-0.00983729695923238));
#33623=CARTESIAN_POINT('Ctrl Pts',(-0.00195475984832837,-0.0398578505814981,
-0.00989907054993767));
#33624=CARTESIAN_POINT('Ctrl Pts',(-0.00200695674159328,-0.0398613483559867,
-0.00994494512315154));
#33625=CARTESIAN_POINT('Ctrl Pts',(-0.00213461105148626,-0.0398700332804864,
-0.0100652472391694));
#33626=CARTESIAN_POINT('Ctrl Pts',(-0.00220780609729937,-0.0398751353458972,
-0.0101419367900389));
#33627=CARTESIAN_POINT('Ctrl Pts',(-0.00242320606735126,-0.039890899785197,
-0.010392982674363));
#33628=CARTESIAN_POINT('Ctrl Pts',(-0.00254995311452363,-0.0399012893600811,
-0.0105795227271284));
#33629=CARTESIAN_POINT('Ctrl Pts',(-0.00266813542260465,-0.0399142231334858,
-0.0108040333618264));
#33630=CARTESIAN_POINT('Ctrl Pts',(-0.00268123659104808,-0.0399157152516365,
-0.0108298195700061));
#33631=CARTESIAN_POINT('Ctrl Pts',(-0.00270014029017881,-0.0399179631098428,
-0.0108683979211079));
#33632=CARTESIAN_POINT('Ctrl Pts',(-0.00270622944840316,-0.0399187026749469,
-0.0108810485612566));
#33633=CARTESIAN_POINT('Ctrl Pts',(-0.00271702252410573,-0.0399200426439551,
-0.0109038806513336));
#33634=CARTESIAN_POINT('Ctrl Pts',(-0.00272175845410706,-0.0399206411373407,
-0.0109140463719535));
#33635=CARTESIAN_POINT('Ctrl Pts',(-0.00273229686775892,-0.0399219969193233,
-0.0109370025767652));
#33636=CARTESIAN_POINT('Ctrl Pts',(-0.00273806658244795,-0.0399227560490853,
-0.0109498073537495));
#33637=CARTESIAN_POINT('Ctrl Pts',(-0.00275540544741321,-0.0399250885108314,
-0.0109890204997561));
#33638=CARTESIAN_POINT('Ctrl Pts',(-0.00276668370052161,-0.0399266774278223,
-0.0110155548654924));
#33639=CARTESIAN_POINT('Ctrl Pts',(-0.00282250314421805,-0.0399349062873632,
-0.0111523243778234));
#33640=CARTESIAN_POINT('Ctrl Pts',(-0.0028608422701259,-0.0399418080382577,
-0.0112649676206232));
#33641=CARTESIAN_POINT('Ctrl Pts',(-0.00294966047371335,-0.0399614114238219,
-0.0115875915182237));
#33642=CARTESIAN_POINT('Ctrl Pts',(-0.00298432685081978,-0.0399741518488867,
-0.0118012033774357));
#33643=CARTESIAN_POINT('Ctrl Pts',(-0.00299857292497328,-0.0399891941625337,
-0.0120693580166509));
#33644=CARTESIAN_POINT('Ctrl Pts',(-0.00299998151196683,-0.0399921098222384,
-0.0121220739398953));
#33645=CARTESIAN_POINT('Ctrl Pts',(-0.0029999998192441,-0.0399949849792216,
-0.0121748118762894));
#33646=CARTESIAN_POINT('Ctrl Pts',(0.00256965295416722,-0.0405776976452009,
-0.0106276660578484));
#33647=CARTESIAN_POINT('Ctrl Pts',(0.00261879861117561,-0.0405720710453063,
-0.0107092371239148));
#33648=CARTESIAN_POINT('Ctrl Pts',(0.00266403531987886,-0.0405664894762788,
-0.0107931070827784));
#33649=CARTESIAN_POINT('Ctrl Pts',(0.00272274854087895,-0.0405587562280604,
-0.0109155807532141));
#33650=CARTESIAN_POINT('Ctrl Pts',(0.00273954608364068,-0.0405564757033417,
-0.0109525242035279));
#33651=CARTESIAN_POINT('Ctrl Pts',(0.00276145282245608,-0.0405534158610409,
-0.0110034206692555));
#33652=CARTESIAN_POINT('Ctrl Pts',(0.00276721497095573,-0.0405526022603544,
-0.011017086159205));
#33653=CARTESIAN_POINT('Ctrl Pts',(0.00277696563795014,-0.0405512108519496,
-0.0110406983771469));
#33654=CARTESIAN_POINT('Ctrl Pts',(0.00278100258354374,-0.0405506302687271,
-0.011050624660749));
#33655=CARTESIAN_POINT('Ctrl Pts',(0.00278905317772386,-0.0405494635330612,
-0.0110707279345512));
#33656=CARTESIAN_POINT('Ctrl Pts',(0.00279306442155231,-0.040548877595032,
-0.0110809054290569));
#33657=CARTESIAN_POINT('Ctrl Pts',(0.00280147737259189,-0.0405476384279538,
-0.0111025981923252));
#33658=CARTESIAN_POINT('Ctrl Pts',(0.00280586396624662,-0.0405469860823097,
-0.0111141191484769));
#33659=CARTESIAN_POINT('Ctrl Pts',(0.00281753865299263,-0.0405452319461826,
-0.0111453592877216));
#33660=CARTESIAN_POINT('Ctrl Pts',(0.00282469081541642,-0.0405441377088638,
-0.0111651288990728));
#33661=CARTESIAN_POINT('Ctrl Pts',(0.00285966167485715,-0.0405386781683054,
-0.0112650649466885));
#33662=CARTESIAN_POINT('Ctrl Pts',(0.00288428004607311,-0.0405344704922299,
-0.0113463166276499));
#33663=CARTESIAN_POINT('Ctrl Pts',(0.0029409825100946,-0.0405234096535795,
-0.0115667564360639));
#33664=CARTESIAN_POINT('Ctrl Pts',(0.00296663176830873,-0.0405167172989409,
-0.011707370721134));
#33665=CARTESIAN_POINT('Ctrl Pts',(0.00299405510528987,-0.0405047420096543,
-0.0119577932318347));
#33666=CARTESIAN_POINT('Ctrl Pts',(0.0030000061268486,-0.0404995086955379,
-0.0120668689222672));
#33667=CARTESIAN_POINT('Ctrl Pts',(0.00299999565021975,-0.040490317626161,
-0.0122533712474678));
#33668=CARTESIAN_POINT('Ctrl Pts',(0.0029969998723812,-0.0404864369948116,
-0.0123306870493325));
#33669=CARTESIAN_POINT('Ctrl Pts',(0.00298876169002086,-0.040480967829138,
-0.0124369220926438));
#33670=CARTESIAN_POINT('Ctrl Pts',(0.00298607791883728,-0.0404794561517935,
-0.0124660117742412));
#33671=CARTESIAN_POINT('Ctrl Pts',(0.00298077556634881,-0.0404768553253285,
-0.0125155624431293));
#33672=CARTESIAN_POINT('Ctrl Pts',(0.00297836996422824,-0.0404757727012125,
-0.0125360443699115));
#33673=CARTESIAN_POINT('Ctrl Pts',(0.00297338539539684,-0.0404736979990825,
-0.0125750119088238));
#33674=CARTESIAN_POINT('Ctrl Pts',(0.00297084470699352,-0.0404727071347163,
-0.0125935014894876));
#33675=CARTESIAN_POINT('Ctrl Pts',(0.00296448897942972,-0.0404703735081709,
-0.0126367578327425));
#33676=CARTESIAN_POINT('Ctrl Pts',(0.00296053585755001,-0.0404690266053592,
-0.0126615026409925));
#33677=CARTESIAN_POINT('Ctrl Pts',(0.00294559992202271,-0.0404642743089021,
-0.0127480226059367));
#33678=CARTESIAN_POINT('Ctrl Pts',(0.00293299013605131,-0.040460820385791,
-0.0128094972915569));
#33679=CARTESIAN_POINT('Ctrl Pts',(0.00286956058495486,-0.0404455098138617,
-0.0130759768735808));
#33680=CARTESIAN_POINT('Ctrl Pts',(0.00279910450280392,-0.040433095513478,
-0.0132756695412901));
#33681=CARTESIAN_POINT('Ctrl Pts',(0.00265818961569454,-0.0404139799100914,
-0.013571414100777));
#33682=CARTESIAN_POINT('Ctrl Pts',(0.00260201391340249,-0.0404072425115315,
-0.0136735480038217));
#33683=CARTESIAN_POINT('Ctrl Pts',(0.00252480006973463,-0.0403991722025544,
-0.0137964102106676));
#33684=CARTESIAN_POINT('Ctrl Pts',(0.00250921473316229,-0.040397595812251,
-0.0138204388490633));
#33685=CARTESIAN_POINT('Ctrl Pts',(0.00248543905272108,-0.0403952720352007,
-0.0138559699092001));
#33686=CARTESIAN_POINT('Ctrl Pts',(0.0024775081064065,-0.0403945097821374,
-0.0138676430927767));
#33687=CARTESIAN_POINT('Ctrl Pts',(0.00246308087557972,-0.040393146780609,
-0.0138885588089788));
#33688=CARTESIAN_POINT('Ctrl Pts',(0.00245661433980383,-0.0403925442145641,
-0.0138978212316271));
#33689=CARTESIAN_POINT('Ctrl Pts',(0.00244191226338605,-0.0403911930484467,
-0.0139186285402674));
#33690=CARTESIAN_POINT('Ctrl Pts',(0.00243364702012821,-0.0403904463853412,
-0.0139301518027545));
#33691=CARTESIAN_POINT('Ctrl Pts',(0.00240780591699792,-0.0403881502051173,
-0.0139656449207905));
#33692=CARTESIAN_POINT('Ctrl Pts',(0.00238995486302466,-0.0403866177372581,
-0.0139894131296663));
#33693=CARTESIAN_POINT('Ctrl Pts',(0.00228766265239588,-0.0403781086559713,
-0.0141214784378251));
#33694=CARTESIAN_POINT('Ctrl Pts',(0.00219620949879302,-0.0403715113958629,
-0.0142241521112112));
#33695=CARTESIAN_POINT('Ctrl Pts',(0.00201370293991924,-0.0403593556999734,
-0.0144027167035425));
#33696=CARTESIAN_POINT('Ctrl Pts',(0.00192457595399876,-0.0403537923047462,
-0.0144801812288325));
#33697=CARTESIAN_POINT('Ctrl Pts',(0.00176300407091633,-0.0403439796037956,
-0.0146046825232077));
#33698=CARTESIAN_POINT('Ctrl Pts',(0.001692665572248,-0.0403397886847267,
-0.0146542150151867));
#33699=CARTESIAN_POINT('Ctrl Pts',(0.00156970597375033,-0.0403325030016915,
-0.014733124701304));
#33700=CARTESIAN_POINT('Ctrl Pts',(0.00151815014602399,-0.0403294598911116,
-0.0147640637623415));
#33701=CARTESIAN_POINT('Ctrl Pts',(0.00144261009357475,-0.0403249991113226,
-0.0148063620828304));
#33702=CARTESIAN_POINT('Ctrl Pts',(0.00141934887838025,-0.040323625294301,
-0.0148189857299882));
#33703=CARTESIAN_POINT('Ctrl Pts',(0.00137822418399705,-0.0403211947113337,
-0.0148406042998392));
#33704=CARTESIAN_POINT('Ctrl Pts',(0.00136043192009853,-0.0403201425808426,
-0.0148497315241323));
#33705=CARTESIAN_POINT('Ctrl Pts',(0.00132313367568664,-0.0403179352565859,
-0.0148683964485055));
#33706=CARTESIAN_POINT('Ctrl Pts',(0.00130361278204073,-0.0403167790319272,
-0.0148779015992171));
#33707=CARTESIAN_POINT('Ctrl Pts',(0.00125205471136081,-0.0403137220116079,
-0.0149023175975434));
#33708=CARTESIAN_POINT('Ctrl Pts',(0.00121985491628539,-0.0403118095254279,
-0.0149168754460356));
#33709=CARTESIAN_POINT('Ctrl Pts',(0.00106230148050335,-0.0403024328539316,
-0.0149847808724365));
#33710=CARTESIAN_POINT('Ctrl Pts',(0.000933683416954394,-0.0402947104725204,
-0.0150301109051748));
#33711=CARTESIAN_POINT('Ctrl Pts',(0.000626722277476678,-0.0402762373237819,
-0.0151153220215603));
#33712=CARTESIAN_POINT('Ctrl Pts',(0.000446927347611358,-0.0402653734004754,
-0.0151479754470612));
#33713=CARTESIAN_POINT('Ctrl Pts',(0.000183769610370934,-0.0402500847053172,
-0.0151713375144694));
#33714=CARTESIAN_POINT('Ctrl Pts',(0.000101986409596025,-0.0402454227535879,
-0.0151752361904458));
#33715=CARTESIAN_POINT('Ctrl Pts',(-7.10287049814954E-7,-0.0402397593314459,
-0.0151759256650622));
#33716=CARTESIAN_POINT('Ctrl Pts',(-2.15626867610429E-5,-0.040238619285167,
-0.0151758482663919));
#33717=CARTESIAN_POINT('Ctrl Pts',(-5.47104820396596E-5,-0.0402368245539899,
-0.0151753795854766));
#33718=CARTESIAN_POINT('Ctrl Pts',(-6.70068523135331E-5,-0.0402361626246399,
-0.0151751300905804));
#33719=CARTESIAN_POINT('Ctrl Pts',(-9.05986260739049E-5,-0.0402349004628171,
-0.0151745062511431));
#33720=CARTESIAN_POINT('Ctrl Pts',(-0.00010189384314063,-0.0402342996626474,
-0.0151741436926928));
#33721=CARTESIAN_POINT('Ctrl Pts',(-0.000129456880718558,-0.0402328416536381,
-0.0151731030268803));
#33722=CARTESIAN_POINT('Ctrl Pts',(-0.000145721954295245,-0.0402319881214045,
-0.0151723562859015));
#33723=CARTESIAN_POINT('Ctrl Pts',(-0.000205350289779144,-0.0402288815833001,
-0.0151691320402153));
#33724=CARTESIAN_POINT('Ctrl Pts',(-0.000248666154669872,-0.0402266686303352,
-0.015165845250389));
#33725=CARTESIAN_POINT('Ctrl Pts',(-0.000361145506699171,-0.0402210018226433,
-0.0151548489326624));
#33726=CARTESIAN_POINT('Ctrl Pts',(-0.0004301407063033,-0.0402176042235468,
-0.0151456716407745));
#33727=CARTESIAN_POINT('Ctrl Pts',(-0.000625350959277983,-0.0402080676315979,
-0.0151127594231186));
#33728=CARTESIAN_POINT('Ctrl Pts',(-0.000750446269556413,-0.04020204348561,
-0.0150833115107572));
#33729=CARTESIAN_POINT('Ctrl Pts',(-0.00103110949125309,-0.0401880903968969,
-0.0149979149648303));
#33730=CARTESIAN_POINT('Ctrl Pts',(-0.00118470396521038,-0.0401801212133555,
-0.0149369559532378));
#33731=CARTESIAN_POINT('Ctrl Pts',(-0.0013645136149081,-0.0401699078832326,
-0.0148478150214952));
#33732=CARTESIAN_POINT('Ctrl Pts',(-0.00139624222860681,-0.0401680712270034,
-0.0148313729003655));
#33733=CARTESIAN_POINT('Ctrl Pts',(-0.00144669697266912,-0.040165091209939,
-0.0148040724457243));
#33734=CARTESIAN_POINT('Ctrl Pts',(-0.00146561291330338,-0.0401639602988138,
-0.0147935711543631));
#33735=CARTESIAN_POINT('Ctrl Pts',(-0.00150154481459948,-0.0401617850485254,
-0.0147731118046841));
#33736=CARTESIAN_POINT('Ctrl Pts',(-0.0015185794801785,-0.0401607419912673,
-0.0147631887842549));
#33737=CARTESIAN_POINT('Ctrl Pts',(-0.00155765497805228,-0.0401583214147595,
-0.0147399077239977));
#33738=CARTESIAN_POINT('Ctrl Pts',(-0.00157962372534291,-0.040156939721628,
-0.0147264322441178));
#33739=CARTESIAN_POINT('Ctrl Pts',(-0.00164963526617186,-0.0401524679235596,
-0.0146822361743953));
#33740=CARTESIAN_POINT('Ctrl Pts',(-0.001696974727142,-0.0401493386928709,
-0.0146504295869694));
#33741=CARTESIAN_POINT('Ctrl Pts',(-0.00180844172346869,-0.0401417103717177,
-0.0145708335762152));
#33742=CARTESIAN_POINT('Ctrl Pts',(-0.00187161906712831,-0.0401371689255701,
-0.0145217929038094));
#33743=CARTESIAN_POINT('Ctrl Pts',(-0.00202926132435129,-0.0401252883990066,
-0.014389000195465));
#33744=CARTESIAN_POINT('Ctrl Pts',(-0.00212053496248324,-0.0401178575547624,
-0.0143017059476906));
#33745=CARTESIAN_POINT('Ctrl Pts',(-0.0022174373159377,-0.0401094469106787,
-0.0141965597787505));
#33746=CARTESIAN_POINT('Ctrl Pts',(-0.00222873319655102,-0.0401084578831224,
-0.0141840941384101));
#33747=CARTESIAN_POINT('Ctrl Pts',(-0.00233152887545786,-0.040099381494069,
-0.0140687177369802));
#33748=CARTESIAN_POINT('Ctrl Pts',(-0.00241595464481703,-0.0400913599467195,
-0.0139597065533433));
#33749=CARTESIAN_POINT('Ctrl Pts',(-0.00250500095086284,-0.0400825120918266,
-0.0138267521562276));
#33750=CARTESIAN_POINT('Ctrl Pts',(-0.00251719828008138,-0.040081290702434,
-0.013808093991366));
#33751=CARTESIAN_POINT('Ctrl Pts',(-0.00253600131703588,-0.0400793949696446,
-0.013778618978742));
#33752=CARTESIAN_POINT('Ctrl Pts',(-0.0025427481482677,-0.0400787120524843,
-0.0137678936158807));
#33753=CARTESIAN_POINT('Ctrl Pts',(-0.00255530963138453,-0.0400774359357042,
-0.0137476412010889));
#33754=CARTESIAN_POINT('Ctrl Pts',(-0.00256113930954321,-0.0400768418216707,
-0.0137381240695144));
#33755=CARTESIAN_POINT('Ctrl Pts',(-0.00257483634965178,-0.0400754410128577,
-0.0137154805012945));
#33756=CARTESIAN_POINT('Ctrl Pts',(-0.0025826567407554,-0.0400746372526873,
-0.013702325810599));
#33757=CARTESIAN_POINT('Ctrl Pts',(-0.00260884008133195,-0.040071930617449,
-0.0136575055015148));
#33758=CARTESIAN_POINT('Ctrl Pts',(-0.00262672465101543,-0.0400700552214901,
-0.0136255628049344));
#33759=CARTESIAN_POINT('Ctrl Pts',(-0.00273586123447575,-0.040058387866461,
-0.0134219858358367));
#33760=CARTESIAN_POINT('Ctrl Pts',(-0.00281084316255062,-0.0400493172240128,
-0.013242135644124));
#33761=CARTESIAN_POINT('Ctrl Pts',(-0.00289558616303424,-0.0400356016518335,
-0.0129660943663709));
#33762=CARTESIAN_POINT('Ctrl Pts',(-0.00291900253868639,-0.0400310943487473,
-0.0128746546558181));
#33763=CARTESIAN_POINT('Ctrl Pts',(-0.00295676732285468,-0.0400219758964842,
-0.0126916843449128));
#33764=CARTESIAN_POINT('Ctrl Pts',(-0.00297126309730216,-0.0400173734528224,
-0.0126002921505042));
#33765=CARTESIAN_POINT('Ctrl Pts',(-0.00298501596369903,-0.040011026572921,
-0.0124769810296456));
#33766=CARTESIAN_POINT('Ctrl Pts',(-0.0029880216525534,-0.0400093960774991,
-0.0124455285153653));
#33767=CARTESIAN_POINT('Ctrl Pts',(-0.00299218877698966,-0.0400066620897498,
-0.0123932075219325));
#33768=CARTESIAN_POINT('Ctrl Pts',(-0.00299362994397026,-0.0400055672142554,
-0.0123723635162052));
#33769=CARTESIAN_POINT('Ctrl Pts',(-0.00299594895766515,-0.0400034789638127,
-0.0123328247810819));
#33770=CARTESIAN_POINT('Ctrl Pts',(-0.00299686982764377,-0.0400024869604999,
-0.0123141335163856));
#33771=CARTESIAN_POINT('Ctrl Pts',(-0.00299836853126886,-0.0400004830281664,
-0.0122765647918212));
#33772=CARTESIAN_POINT('Ctrl Pts',(-0.00299894309789592,-0.03999947104557,
-0.012257688060272));
#33773=CARTESIAN_POINT('Ctrl Pts',(-0.00299978707736779,-0.0399973042605326,
-0.0122174781542378));
#33774=CARTESIAN_POINT('Ctrl Pts',(-0.00300000722478825,-0.0399961480195609,
-0.0121961450931526));
#33775=CARTESIAN_POINT('Ctrl Pts',(-0.0029999998192441,-0.0399949849792216,
-0.0121748118762893));
#33776=CARTESIAN_POINT('Origin',(1.7347234759768E-18,-0.0298787743898723,
-0.0121758532865581));
#33777=CARTESIAN_POINT('',(-0.00250000000000292,-0.0304787743898694,-0.0121758532865581));
#33778=CARTESIAN_POINT('Origin',(1.00024155624823E-14,-0.0304787743898623,
-0.0121758532865681));
#33779=CARTESIAN_POINT('',(-0.0031,-0.0298787743898723,-0.0121758532865581));
#33780=CARTESIAN_POINT('Origin',(1.00024155624823E-14,-0.0304787743898623,
-0.0121758532865681));
#33781=CARTESIAN_POINT('Origin',(0.,-0.0424924495244671,-0.0121758532865581));
#33782=CARTESIAN_POINT('Origin',(1.00024155624823E-14,-0.0304787743898623,
-0.0121758532865681));
#33783=CARTESIAN_POINT('Ctrl Pts',(0.00667266361729431,-0.0408411507555838,
-0.0135686213491869));
#33784=CARTESIAN_POINT('Ctrl Pts',(0.00621453914932291,-0.0408149751823628,
-0.0137898879259038));
#33785=CARTESIAN_POINT('Ctrl Pts',(0.00507072224427489,-0.040762628119428,
-0.0137417506490211));
#33786=CARTESIAN_POINT('Ctrl Pts',(0.00417951551514757,-0.0406841095667795,
-0.0122616719912261));
#33787=CARTESIAN_POINT('Ctrl Pts',(0.00492533652721776,-0.0406055950976381,
-0.0107057736276615));
#33788=CARTESIAN_POINT('Ctrl Pts',(0.00663317335312316,-0.0405270806284968,
-0.0104680447707994));
#33789=CARTESIAN_POINT('Ctrl Pts',(0.00777404656683587,-0.0404485661593554,
-0.011762495846534));
#33790=CARTESIAN_POINT('Ctrl Pts',(0.00732306899069569,-0.0403700516902141,
-0.0134276029751788));
#33791=CARTESIAN_POINT('Ctrl Pts',(0.0056855439467377,-0.0402915372210728,
-0.0139699426948976));
#33792=CARTESIAN_POINT('Ctrl Pts',(0.00432995641023964,-0.0402130227519315,
-0.0129029294162582));
#33793=CARTESIAN_POINT('Ctrl Pts',(0.00447248538985062,-0.0401345082827901,
-0.0111837377979531));
#33794=CARTESIAN_POINT('Ctrl Pts',(0.0059851779029977,-0.0400559938136489,
-0.0103544763934777));
#33795=CARTESIAN_POINT('Ctrl Pts',(0.00751118377554786,-0.0399774793445075,
-0.0111590157052924));
#33796=CARTESIAN_POINT('Ctrl Pts',(0.00768163121117975,-0.0398989648753662,
-0.0128756677943404));
#33797=CARTESIAN_POINT('Ctrl Pts',(0.00634364059981585,-0.0398204504062249,
-0.013964579343715));
#33798=CARTESIAN_POINT('Ctrl Pts',(0.0046973980185026,-0.0397419359370836,
-0.0134489822855388));
#33799=CARTESIAN_POINT('Ctrl Pts',(0.00421960572095684,-0.0396634214679422,
-0.0117913740701257));
#33800=CARTESIAN_POINT('Ctrl Pts',(0.0053388471060399,-0.0395849069988008,
-0.0104786480096583));
#33801=CARTESIAN_POINT('Ctrl Pts',(0.00705115061506779,-0.0395063925296596,
-0.0106883348320183));
#33802=CARTESIAN_POINT('Ctrl Pts',(0.00782055967922068,-0.0394278780605182,
-0.0122323429056206));
#33803=CARTESIAN_POINT('Ctrl Pts',(0.00695690569528211,-0.0393493635913769,
-0.0137256791573249));
#33804=CARTESIAN_POINT('Ctrl Pts',(0.00523489617102149,-0.0392708491222356,
-0.0138288036313886));
#33805=CARTESIAN_POINT('Ctrl Pts',(0.00419919366962196,-0.0391923346530943,
-0.0124492124957124));
#33806=CARTESIAN_POINT('Ctrl Pts',(0.00477883530496066,-0.0391138201839529,
-0.010824414978702));
#33807=CARTESIAN_POINT('Ctrl Pts',(0.00645387582937621,-0.0390353057148116,
-0.010411873286939));
#33808=CARTESIAN_POINT('Ctrl Pts',(0.00772178447199111,-0.0389567912456703,
-0.0115816420968184));
#33809=CARTESIAN_POINT('Ctrl Pts',(0.00744523249116456,-0.0388782767765289,
-0.0132844252303561));
#33810=CARTESIAN_POINT('Ctrl Pts',(0.00587229021614751,-0.0387997623073876,
-0.0139928064833142));
#33811=CARTESIAN_POINT('Ctrl Pts',(0.00441390509800126,-0.0387212478382463,
-0.0130713596616639));
#33812=CARTESIAN_POINT('Ctrl Pts',(0.00437826548718945,-0.038642733369105,
-0.0113466332448878));
#33813=CARTESIAN_POINT('Ctrl Pts',(0.00579734052997675,-0.0385642188999636,
-0.010365726812645));
#33814=CARTESIAN_POINT('Ctrl Pts',(0.00739820346327778,-0.0384857044308223,
-0.0110085248100627));
#33815=CARTESIAN_POINT('Ctrl Pts',(0.00774486169156298,-0.038407189961681,
-0.0126984299688818));
#33816=CARTESIAN_POINT('Ctrl Pts',(0.00652635875128295,-0.0383286754925397,
-0.0139195778073208));
#33817=CARTESIAN_POINT('Ctrl Pts',(0.00483570593105475,-0.0382501610233984,
-0.0135765845040604));
#33818=CARTESIAN_POINT('Ctrl Pts',(0.00418943834467669,-0.038171646554257,
-0.0119771191414636));
#33819=CARTESIAN_POINT('Ctrl Pts',(0.00516726562172514,-0.0380931320851157,
-0.0105559204619115));
#33820=CARTESIAN_POINT('Ctrl Pts',(0.00689206513754615,-0.0380146176159744,
-0.0105878205894473));
#33821=CARTESIAN_POINT('Ctrl Pts',(0.00781667217861196,-0.037936103146833,
-0.012044203882063));
#33822=CARTESIAN_POINT('Ctrl Pts',(0.00711170265126494,-0.0378575886776917,
-0.01361867932755));
#33823=CARTESIAN_POINT('Ctrl Pts',(0.00540952407975407,-0.0377790742085504,
-0.0138989209182331));
#33824=CARTESIAN_POINT('Ctrl Pts',(0.00423700706452516,-0.0377005597394091,
-0.0126335551323258));
#33825=CARTESIAN_POINT('Ctrl Pts',(0.00464591942445379,-0.0376220452702677,
-0.0109576171533986));
#33826=CARTESIAN_POINT('Ctrl Pts',(0.00626944937421679,-0.0375435308011264,
-0.0103744674140466));
#33827=CARTESIAN_POINT('Ctrl Pts',(0.0076512965121535,-0.0374650163319851,
-0.0114071497552607));
#33828=CARTESIAN_POINT('Ctrl Pts',(0.007551879443792,-0.0373865018628437,
-0.013129430554788));
#33829=CARTESIAN_POINT('Ctrl Pts',(0.006060471354512,-0.0373079873937024,
-0.0139962191982324));
#33830=CARTESIAN_POINT('Ctrl Pts',(0.00451469679310158,-0.0372294729245611,
-0.0132303578992094));
#33831=CARTESIAN_POINT('Ctrl Pts',(0.0043014971156851,-0.0371509584554198,
-0.0115181250952989));
#33832=CARTESIAN_POINT('Ctrl Pts',(0.00561140292832371,-0.0370724439862784,
-0.0103968007018607));
#33833=CARTESIAN_POINT('Ctrl Pts',(0.00727080916413441,-0.0369939295171371,
-0.0108694947301078));
#33834=CARTESIAN_POINT('Ctrl Pts',(0.00778849486716388,-0.0369154089680987,
-0.0125178380097699));
#33835=CARTESIAN_POINT('Ctrl Pts',(0.00706639652799099,-0.036863059908774,
-0.013406293288968));
#33836=CARTESIAN_POINT('Ctrl Pts',(0.0065970260151864,-0.0368368823391631,
-0.0136026816399946));
#33837=CARTESIAN_POINT('Ctrl Pts',(0.00663125973307481,-0.0408961160367515,
-0.0134828934963237));
#33838=CARTESIAN_POINT('Ctrl Pts',(0.00620133380586334,-0.0408699404635307,
-0.0136905406420376));
#33839=CARTESIAN_POINT('Ctrl Pts',(0.00512792127751624,-0.0408175934005959,
-0.0136453663174946));
#33840=CARTESIAN_POINT('Ctrl Pts',(0.00429157022852352,-0.0407390748479473,
-0.0122563896664198));
#33841=CARTESIAN_POINT('Ctrl Pts',(0.00499148436226952,-0.040660560378806,
-0.0107962601746154));
#33842=CARTESIAN_POINT('Ctrl Pts',(0.00659420017911819,-0.0405820459096646,
-0.010573164037306));
#33843=CARTESIAN_POINT('Ctrl Pts',(0.00766485020662715,-0.0405035314405233,
-0.011787938880984));
#33844=CARTESIAN_POINT('Ctrl Pts',(0.00724163126477025,-0.040425016971382,
-0.0133505551048212));
#33845=CARTESIAN_POINT('Ctrl Pts',(0.00570489938931959,-0.0403465025022407,
-0.0138595126549301));
#33846=CARTESIAN_POINT('Ctrl Pts',(0.00443275116478599,-0.0402679880330993,
-0.0128581763255321));
#33847=CARTESIAN_POINT('Ctrl Pts',(0.00456650718088586,-0.0401894735639581,
-0.0112448046280396));
#33848=CARTESIAN_POINT('Ctrl Pts',(0.00598609023476707,-0.0401109590948166,
-0.0104665860364886));
#33849=CARTESIAN_POINT('Ctrl Pts',(0.00741816718230774,-0.0400324446256754,
-0.0112216042330534));
#33850=CARTESIAN_POINT('Ctrl Pts',(0.00757812321375344,-0.0399539301565341,
-0.0128325927147457));
#33851=CARTESIAN_POINT('Ctrl Pts',(0.00632248878597894,-0.0398754156873926,
-0.0138544794294832));
#33852=CARTESIAN_POINT('Ctrl Pts',(0.00477757595624066,-0.0397969012182514,
-0.0133706184729063));
#33853=CARTESIAN_POINT('Ctrl Pts',(0.00432919279642726,-0.0397183867491099,
-0.011815039588154));
#33854=CARTESIAN_POINT('Ctrl Pts',(0.0053795424806211,-0.0396398722799688,
-0.0105831146241368));
#33855=CARTESIAN_POINT('Ctrl Pts',(0.00698645004669358,-0.0395613578108274,
-0.0107798947741392));
#33856=CARTESIAN_POINT('Ctrl Pts',(0.00770850033747063,-0.0394828433416861,
-0.0122288658487573));
#33857=CARTESIAN_POINT('Ctrl Pts',(0.00689800610327526,-0.0394043288725447,
-0.0136302840604831));
#33858=CARTESIAN_POINT('Ctrl Pts',(0.00528198994796513,-0.0393258144034035,
-0.0137270610026236));
#33859=CARTESIAN_POINT('Ctrl Pts',(0.00431003715050586,-0.0392472999342621,
-0.0124323866517762));
#33860=CARTESIAN_POINT('Ctrl Pts',(0.00485400060355347,-0.0391687854651208,
-0.01090759889677));
#33861=CARTESIAN_POINT('Ctrl Pts',(0.00642593880140802,-0.0390902709959795,
-0.0105204500284067));
#33862=CARTESIAN_POINT('Ctrl Pts',(0.00761580495548908,-0.0390117565268381,
-0.0116182170663417));
#33863=CARTESIAN_POINT('Ctrl Pts',(0.00735627534052331,-0.0389332420576968,
-0.0132161902563959));
#33864=CARTESIAN_POINT('Ctrl Pts',(0.00588015102646683,-0.0388547275885554,
-0.0138809691282728));
#33865=CARTESIAN_POINT('Ctrl Pts',(0.00451153263128116,-0.0387762131194141,
-0.013016239329124));
#33866=CARTESIAN_POINT('Ctrl Pts',(0.00447808671473453,-0.0386976986502728,
-0.0113976735118431));
#33867=CARTESIAN_POINT('Ctrl Pts',(0.00580981465376934,-0.0386191841811315,
-0.0104771439682956));
#33868=CARTESIAN_POINT('Ctrl Pts',(0.00731214104988036,-0.0385406697119902,
-0.0110803763742686));
#33869=CARTESIAN_POINT('Ctrl Pts',(0.00763746172284284,-0.0384621552428488,
-0.0126662642564893));
#33870=CARTESIAN_POINT('Ctrl Pts',(0.00649396024445763,-0.0383836407737075,
-0.0138122478338953));
#33871=CARTESIAN_POINT('Ctrl Pts',(0.00490737072098658,-0.0383051263045662,
-0.0134903665019845));
#33872=CARTESIAN_POINT('Ctrl Pts',(0.00430088228667392,-0.0382266118354249,
-0.0119893516531119));
#33873=CARTESIAN_POINT('Ctrl Pts',(0.0052185222036143,-0.0381480973662836,
-0.010655630791697));
#33874=CARTESIAN_POINT('Ctrl Pts',(0.00683715662053758,-0.0380695828971422,
-0.0106855673981607));
#33875=CARTESIAN_POINT('Ctrl Pts',(0.00770485212083813,-0.0379910684280009,
-0.0120523071844584));
#33876=CARTESIAN_POINT('Ctrl Pts',(0.00704327497556473,-0.0379125539588594,
-0.0135298702990634));
#33877=CARTESIAN_POINT('Ctrl Pts',(0.00544586913545169,-0.0378340394897182,
-0.0137928624205084));
#33878=CARTESIAN_POINT('Ctrl Pts',(0.00434552305008409,-0.0377555250205769,
-0.0126053826048663));
#33879=CARTESIAN_POINT('Ctrl Pts',(0.00472926597974898,-0.0376770105514356,
-0.0110326021927446));
#33880=CARTESIAN_POINT('Ctrl Pts',(0.00625286418898258,-0.0375984960822943,
-0.0104853465669882));
#33881=CARTESIAN_POINT('Ctrl Pts',(0.00754965568032684,-0.0375199816131529,
-0.0114544651015805));
#33882=CARTESIAN_POINT('Ctrl Pts',(0.00745635794513875,-0.0374414671440116,
-0.0130707358345845));
#33883=CARTESIAN_POINT('Ctrl Pts',(0.0060567492133162,-0.0373629526748703,
-0.0138841717832892));
#33884=CARTESIAN_POINT('Ctrl Pts',(0.00460612038199239,-0.037284438205729,
-0.0131654508851109));
#33885=CARTESIAN_POINT('Ctrl Pts',(0.0044060436006751,-0.0372059237365876,
-0.0115586096721047));
#33886=CARTESIAN_POINT('Ctrl Pts',(0.00563532190914864,-0.0371274092674463,
-0.0105063051931748));
#33887=CARTESIAN_POINT('Ctrl Pts',(0.00719258814229796,-0.037048894798305,
-0.010949903893068));
#33888=CARTESIAN_POINT('Ctrl Pts',(0.00767840918317049,-0.0369703742492665,
-0.0124967881186791));
#33889=CARTESIAN_POINT('Ctrl Pts',(0.007000757541071,-0.0369180251899419,
-0.0133305570753701));
#33890=CARTESIAN_POINT('Ctrl Pts',(0.006560277787137,-0.0368918476203311,
-0.01351485730339));
#33891=CARTESIAN_POINT('Ctrl Pts',(0.0065898558488552,-0.0409510813179196,
-0.0133971656434607));
#33892=CARTESIAN_POINT('Ctrl Pts',(0.00618812846240375,-0.0409249057446983,
-0.0135911933581714));
#33893=CARTESIAN_POINT('Ctrl Pts',(0.00518512031075758,-0.0408725586817636,
-0.0135489819859681));
#33894=CARTESIAN_POINT('Ctrl Pts',(0.00440362494189948,-0.0407940401291151,
-0.0122511073416135));
#33895=CARTESIAN_POINT('Ctrl Pts',(0.00505763219732118,-0.0407155256599738,
-0.0108867467215694));
#33896=CARTESIAN_POINT('Ctrl Pts',(0.00655522700511323,-0.0406370111908325,
-0.0106782833038126));
#33897=CARTESIAN_POINT('Ctrl Pts',(0.00755565384641844,-0.0405584967216911,
-0.0118133819154339));
#33898=CARTESIAN_POINT('Ctrl Pts',(0.00716019353884481,-0.0404799822525498,
-0.0132735072344637));
#33899=CARTESIAN_POINT('Ctrl Pts',(0.00572425483190137,-0.0404014677834084,
-0.0137490826149629));
#33900=CARTESIAN_POINT('Ctrl Pts',(0.00453554591933244,-0.0403229533142671,
-0.0128134232348059));
#33901=CARTESIAN_POINT('Ctrl Pts',(0.00466052897192121,-0.0402444388451258,
-0.0113058714581259));
#33902=CARTESIAN_POINT('Ctrl Pts',(0.00598700256653645,-0.0401659243759845,
-0.0105786956794995));
#33903=CARTESIAN_POINT('Ctrl Pts',(0.00732515058906774,-0.0400874099068432,
-0.0112841927608144));
#33904=CARTESIAN_POINT('Ctrl Pts',(0.00747461521632705,-0.0400088954377018,
-0.0127895176351511));
#33905=CARTESIAN_POINT('Ctrl Pts',(0.00630133697214193,-0.0399303809685605,
-0.0137443795152512));
#33906=CARTESIAN_POINT('Ctrl Pts',(0.00485775389397871,-0.0398518664994192,
-0.0132922546602737));
#33907=CARTESIAN_POINT('Ctrl Pts',(0.00443877987189778,-0.0397733520302779,
-0.0118387051061822));
#33908=CARTESIAN_POINT('Ctrl Pts',(0.0054202378552023,-0.0396948375611365,
-0.0106875812386152));
#33909=CARTESIAN_POINT('Ctrl Pts',(0.00692174947831937,-0.0396163230919952,
-0.01087145471626));
#33910=CARTESIAN_POINT('Ctrl Pts',(0.00759644099572046,-0.0395378086228539,
-0.0122253887918938));
#33911=CARTESIAN_POINT('Ctrl Pts',(0.00683910651126841,-0.0394592941537125,
-0.0135348889636414));
#33912=CARTESIAN_POINT('Ctrl Pts',(0.00532908372490877,-0.0393807796845712,
-0.0136253183738586));
#33913=CARTESIAN_POINT('Ctrl Pts',(0.00442088063138974,-0.0393022652154299,
-0.01241556080784));
#33914=CARTESIAN_POINT('Ctrl Pts',(0.00492916590214617,-0.0392237507462886,
-0.010990782814838));
#33915=CARTESIAN_POINT('Ctrl Pts',(0.00639800177343982,-0.0391452362771472,
-0.0106290267698747));
#33916=CARTESIAN_POINT('Ctrl Pts',(0.00750982543898704,-0.0390667218080059,
-0.0116547920358649));
#33917=CARTESIAN_POINT('Ctrl Pts',(0.00726731818988206,-0.0389882073388646,
-0.0131479552824357));
#33918=CARTESIAN_POINT('Ctrl Pts',(0.00588801183678637,-0.0389096928697233,
-0.0137691317732312));
#33919=CARTESIAN_POINT('Ctrl Pts',(0.00460916016456105,-0.038831178400582,
-0.012961118996584));
#33920=CARTESIAN_POINT('Ctrl Pts',(0.00457790794227973,-0.0387526639314406,
-0.0114487137787985));
#33921=CARTESIAN_POINT('Ctrl Pts',(0.00582228877756173,-0.0386741494622993,
-0.0105885611239463));
#33922=CARTESIAN_POINT('Ctrl Pts',(0.00722607863648303,-0.038595634993158,
-0.0111522279384746));
#33923=CARTESIAN_POINT('Ctrl Pts',(0.00753006175412259,-0.0385171205240167,
-0.0126340985440969));
#33924=CARTESIAN_POINT('Ctrl Pts',(0.0064615617376323,-0.0384386060548753,
-0.01370491786047));
#33925=CARTESIAN_POINT('Ctrl Pts',(0.00497903551091831,-0.038360091585734,
-0.0134041484999088));
#33926=CARTESIAN_POINT('Ctrl Pts',(0.00441232622867113,-0.0382815771165927,
-0.0120015841647602));
#33927=CARTESIAN_POINT('Ctrl Pts',(0.00526977878550357,-0.0382030626474514,
-0.0107553411214825));
#33928=CARTESIAN_POINT('Ctrl Pts',(0.006782248103529,-0.03812454817831,
-0.0107833142068739));
#33929=CARTESIAN_POINT('Ctrl Pts',(0.0075930320630644,-0.0380460337091687,
-0.0120604104868537));
#33930=CARTESIAN_POINT('Ctrl Pts',(0.00697484729986451,-0.0379675192400273,
-0.0134410612705769));
#33931=CARTESIAN_POINT('Ctrl Pts',(0.00548221419114921,-0.037889004770886,
-0.0136868039227835));
#33932=CARTESIAN_POINT('Ctrl Pts',(0.00445403903564292,-0.0378104903017447,
-0.0125772100774068));
#33933=CARTESIAN_POINT('Ctrl Pts',(0.00481261253504416,-0.0377319758326034,
-0.0111075872320905));
#33934=CARTESIAN_POINT('Ctrl Pts',(0.00623627900374848,-0.037653461363462,
-0.0105962257199298));
#33935=CARTESIAN_POINT('Ctrl Pts',(0.00744801484850009,-0.0375749468943207,
-0.0115017804479003));
#33936=CARTESIAN_POINT('Ctrl Pts',(0.00736083644648552,-0.0374964324251795,
-0.0130120411143809));
#33937=CARTESIAN_POINT('Ctrl Pts',(0.0060530270721205,-0.037417917956038,
-0.013772124368346));
#33938=CARTESIAN_POINT('Ctrl Pts',(0.00469754397088331,-0.0373394034868968,
-0.0131005438710126));
#33939=CARTESIAN_POINT('Ctrl Pts',(0.0045105900856651,-0.0372608890177554,
-0.0115990942489104));
#33940=CARTESIAN_POINT('Ctrl Pts',(0.00565924088997368,-0.0371823745486141,
-0.010615809684489));
#33941=CARTESIAN_POINT('Ctrl Pts',(0.00711436712046152,-0.0371038600794727,
-0.0110303130560284));
#33942=CARTESIAN_POINT('Ctrl Pts',(0.0075683234991771,-0.0370253395304344,
-0.0124757382275885));
#33943=CARTESIAN_POINT('Ctrl Pts',(0.00693511855415113,-0.0369729904711097,
-0.0132548208617724));
#33944=CARTESIAN_POINT('Ctrl Pts',(0.00652352955908771,-0.0369468129014988,
-0.0134270329667855));
#33945=CARTESIAN_POINT('Ctrl Pts',(0.0065484519646357,-0.0410060465990872,
-0.0133114377905975));
#33946=CARTESIAN_POINT('Ctrl Pts',(0.00617492311894418,-0.0409798710258663,
-0.0134918460743052));
#33947=CARTESIAN_POINT('Ctrl Pts',(0.00524231934399881,-0.0409275239629315,
-0.0134525976544415));
#33948=CARTESIAN_POINT('Ctrl Pts',(0.00451567965527543,-0.0408490054102829,
-0.0122458250168071));
#33949=CARTESIAN_POINT('Ctrl Pts',(0.00512378003237285,-0.0407704909411417,
-0.0109772332685232));
#33950=CARTESIAN_POINT('Ctrl Pts',(0.00651625383110827,-0.0406919764720003,
-0.0107834025703192));
#33951=CARTESIAN_POINT('Ctrl Pts',(0.00744645748620972,-0.0406134620028589,
-0.0118388249498838));
#33952=CARTESIAN_POINT('Ctrl Pts',(0.00707875581291927,-0.0405349475337177,
-0.0131964593641061));
#33953=CARTESIAN_POINT('Ctrl Pts',(0.00574361027448316,-0.0404564330645763,
-0.0136386525749953));
#33954=CARTESIAN_POINT('Ctrl Pts',(0.00463834067387879,-0.040377918595435,
-0.01276867014408));
#33955=CARTESIAN_POINT('Ctrl Pts',(0.00475455076295656,-0.0402994041262936,
-0.0113669382882124));
#33956=CARTESIAN_POINT('Ctrl Pts',(0.00598791489830592,-0.0402208896571524,
-0.0106908053225104));
#33957=CARTESIAN_POINT('Ctrl Pts',(0.00723213399582761,-0.040142375188011,
-0.0113467812885753));
#33958=CARTESIAN_POINT('Ctrl Pts',(0.00737110721890075,-0.0400638607188697,
-0.0127464425555564));
#33959=CARTESIAN_POINT('Ctrl Pts',(0.00628018515830493,-0.0399853462497283,
-0.0136342796010194));
#33960=CARTESIAN_POINT('Ctrl Pts',(0.00493793183171677,-0.0399068317805871,
-0.0132138908476413));
#33961=CARTESIAN_POINT('Ctrl Pts',(0.0045483669473682,-0.0398283173114457,
-0.0118623706242104));
#33962=CARTESIAN_POINT('Ctrl Pts',(0.0054609332297836,-0.0397498028423044,
-0.0107920478530937));
#33963=CARTESIAN_POINT('Ctrl Pts',(0.00685704890994516,-0.0396712883731631,
-0.0109630146583807));
#33964=CARTESIAN_POINT('Ctrl Pts',(0.00748438165397041,-0.0395927739040217,
-0.0122219117350304));
#33965=CARTESIAN_POINT('Ctrl Pts',(0.00678020691926156,-0.0395142594348804,
-0.0134394938667997));
#33966=CARTESIAN_POINT('Ctrl Pts',(0.00537617750185241,-0.0394357449657391,
-0.0135235757450938));
#33967=CARTESIAN_POINT('Ctrl Pts',(0.00453172411227353,-0.0393572304965978,
-0.0123987349639038));
#33968=CARTESIAN_POINT('Ctrl Pts',(0.00500433120073897,-0.0392787160274565,
-0.0110739667329061));
#33969=CARTESIAN_POINT('Ctrl Pts',(0.00637006474547161,-0.0392002015583151,
-0.0107376035113427));
#33970=CARTESIAN_POINT('Ctrl Pts',(0.00740384592248502,-0.0391216870891738,
-0.0116913670053881));
#33971=CARTESIAN_POINT('Ctrl Pts',(0.00717836103924093,-0.0390431726200324,
-0.0130797203084755));
#33972=CARTESIAN_POINT('Ctrl Pts',(0.00589587264710569,-0.0389646581508911,
-0.0136572944181898));
#33973=CARTESIAN_POINT('Ctrl Pts',(0.00470678769784105,-0.0388861436817498,
-0.0129059986640441));
#33974=CARTESIAN_POINT('Ctrl Pts',(0.0046777291698248,-0.0388076292126085,
-0.0114997540457538));
#33975=CARTESIAN_POINT('Ctrl Pts',(0.00583476290135422,-0.0387291147434672,
-0.0106999782795971));
#33976=CARTESIAN_POINT('Ctrl Pts',(0.00714001622308571,-0.0386506002743258,
-0.0112240795026805));
#33977=CARTESIAN_POINT('Ctrl Pts',(0.00742266178540245,-0.0385720858051845,
-0.0126019328317044));
#33978=CARTESIAN_POINT('Ctrl Pts',(0.00642916323080688,-0.0384935713360431,
-0.0135975878870446));
#33979=CARTESIAN_POINT('Ctrl Pts',(0.00505070030085003,-0.0384150568669019,
-0.013317930497833));
#33980=CARTESIAN_POINT('Ctrl Pts',(0.00452377017066826,-0.0383365423977605,
-0.0120138166764086));
#33981=CARTESIAN_POINT('Ctrl Pts',(0.00532103536739272,-0.0382580279286192,
-0.010855051451268));
#33982=CARTESIAN_POINT('Ctrl Pts',(0.00672733958652042,-0.0381795134594779,
-0.0108810610155872));
#33983=CARTESIAN_POINT('Ctrl Pts',(0.00748121200529069,-0.0381009989903365,
-0.0120685137892491));
#33984=CARTESIAN_POINT('Ctrl Pts',(0.00690641962416429,-0.0380224845211952,
-0.0133522522420902));
#33985=CARTESIAN_POINT('Ctrl Pts',(0.00551855924684682,-0.0379439700520539,
-0.0135807454250589));
#33986=CARTESIAN_POINT('Ctrl Pts',(0.00456255502120176,-0.0378654555829126,
-0.0125490375499473));
#33987=CARTESIAN_POINT('Ctrl Pts',(0.00489595909033924,-0.0377869411137712,
-0.0111825722714365));
#33988=CARTESIAN_POINT('Ctrl Pts',(0.00621969381851428,-0.0377084266446299,
-0.0107071048728713));
#33989=CARTESIAN_POINT('Ctrl Pts',(0.00734637401667343,-0.0376299121754886,
-0.0115490957942202));
#33990=CARTESIAN_POINT('Ctrl Pts',(0.00726531494783229,-0.0375513977063472,
-0.0129533463941774));
#33991=CARTESIAN_POINT('Ctrl Pts',(0.0060493049309247,-0.037472883237206,
-0.0136600769534027));
#33992=CARTESIAN_POINT('Ctrl Pts',(0.00478896755977412,-0.0373943687680646,
-0.0130356368569142));
#33993=CARTESIAN_POINT('Ctrl Pts',(0.00461513657065499,-0.0373158542989233,
-0.0116395788257163));
#33994=CARTESIAN_POINT('Ctrl Pts',(0.00568315987079862,-0.0372373398297819,
-0.010725314175803));
#33995=CARTESIAN_POINT('Ctrl Pts',(0.00703614609862507,-0.0371588253606407,
-0.0111107222189887));
#33996=CARTESIAN_POINT('Ctrl Pts',(0.00745823781518362,-0.0370803048116022,
-0.0124546883364978));
#33997=CARTESIAN_POINT('Ctrl Pts',(0.00686947956723124,-0.0370279557522776,
-0.0131790846481745));
#33998=CARTESIAN_POINT('Ctrl Pts',(0.00648678133103831,-0.0370017781826666,
-0.0133392086301809));
#33999=CARTESIAN_POINT('Ctrl Pts',(0.00680869722628235,-0.0368513852118003,
-0.0134899528977776));
#34000=CARTESIAN_POINT('Ctrl Pts',(0.00706735492668958,-0.0368670469798486,
-0.0133307713422738));
#34001=CARTESIAN_POINT('Ctrl Pts',(0.00748740299124012,-0.0368983794779675,
-0.0128554401592746));
#34002=CARTESIAN_POINT('Ctrl Pts',(0.00761399556669309,-0.036945382706157,
-0.0119117220579786));
#34003=CARTESIAN_POINT('Ctrl Pts',(0.00719343876865978,-0.0369923574079242,
-0.0110581054138011));
#34004=CARTESIAN_POINT('Ctrl Pts',(0.00664452962814855,-0.0370236613796206,
-0.0107415249439345));
#34005=CARTESIAN_POINT('Ctrl Pts',(0.00634923972919489,-0.0370392946212466,
-0.010672896044278));
#34006=CARTESIAN_POINT('Ctrl Pts',(0.00445700002442818,-0.0406839559076129,
-0.0121761278505149));
#34007=CARTESIAN_POINT('Ctrl Pts',(0.00445699610157866,-0.0406827676486519,
-0.0121540821429041));
#34008=CARTESIAN_POINT('Ctrl Pts',(0.00445746464932956,-0.0406815592236051,
-0.0121320397232979));
#34009=CARTESIAN_POINT('Ctrl Pts',(0.00446156087853884,-0.0406762331732241,
-0.0120361258433312));
#34010=CARTESIAN_POINT('Ctrl Pts',(0.00447002471206943,-0.0406719777460916,
-0.0119625611665503));
#34011=CARTESIAN_POINT('Ctrl Pts',(0.00450200642077586,-0.0406621029460487,
-0.0117929836898513));
#34012=CARTESIAN_POINT('Ctrl Pts',(0.00452953269981767,-0.0406565356122923,
-0.0116980411010296));
#34013=CARTESIAN_POINT('Ctrl Pts',(0.00457463140256198,-0.0406499852539944,
-0.0115844750880577));
#34014=CARTESIAN_POINT('Ctrl Pts',(0.00458382523766999,-0.0406487381886269,
-0.0115627848288545));
#34015=CARTESIAN_POINT('Ctrl Pts',(0.00459988476268503,-0.0406466973971073,
-0.0115271881703461));
#34016=CARTESIAN_POINT('Ctrl Pts',(0.00460646965420429,-0.0406458946660406,
-0.0115131600629839));
#34017=CARTESIAN_POINT('Ctrl Pts',(0.00461987221006823,-0.040644325122731,
-0.0114856914810224));
#34018=CARTESIAN_POINT('Ctrl Pts',(0.00462667765992274,-0.0406435580169627,
-0.0114722470012902));
#34019=CARTESIAN_POINT('Ctrl Pts',(0.00464393981669878,-0.0406416825463828,
-0.0114393497688382));
#34020=CARTESIAN_POINT('Ctrl Pts',(0.00465461941167596,-0.0406405818082087,
-0.0114200174686332));
#34021=CARTESIAN_POINT('Ctrl Pts',(0.0047003606599803,-0.0406360947328233,
-0.0113412595959409));
#34022=CARTESIAN_POINT('Ctrl Pts',(0.0047389748587225,-0.0406328295109826,
-0.0112839868539343));
#34023=CARTESIAN_POINT('Ctrl Pts',(0.00483288730224696,-0.0406256990940078,
-0.01116304883702));
#34024=CARTESIAN_POINT('Ctrl Pts',(0.00488982378172016,-0.0406218727514404,
-0.0111009427466056));
#34025=CARTESIAN_POINT('Ctrl Pts',(0.00498023015181734,-0.0406160276615646,
-0.0110172126458984));
#34026=CARTESIAN_POINT('Ctrl Pts',(0.0050099234258388,-0.0406141378072767,
-0.0109917389892215));
#34027=CARTESIAN_POINT('Ctrl Pts',(0.00505052177962872,-0.0406115456802015,
-0.0109595053832507));
#34028=CARTESIAN_POINT('Ctrl Pts',(0.0050605906932869,-0.0406109021456263,
-0.0109517122619234));
#34029=CARTESIAN_POINT('Ctrl Pts',(0.00507760783578008,-0.0406098113526726,
-0.0109388749559681));
#34030=CARTESIAN_POINT('Ctrl Pts',(0.00508450402403877,-0.0406093684477241,
-0.0109337623838509));
#34031=CARTESIAN_POINT('Ctrl Pts',(0.00509908128073857,-0.0406084296674785,
-0.0109231427130448));
#34032=CARTESIAN_POINT('Ctrl Pts',(0.00510677085686588,-0.0406079330586185,
-0.0109176482123518));
#34033=CARTESIAN_POINT('Ctrl Pts',(0.0051287495830447,-0.0406065108169485,
-0.0109022465828717));
#34034=CARTESIAN_POINT('Ctrl Pts',(0.00514315603632636,-0.0406055752556271,
-0.0108925101137455));
#34035=CARTESIAN_POINT('Ctrl Pts',(0.00521103014543226,-0.0406011634196553,
-0.0108482903692046));
#34036=CARTESIAN_POINT('Ctrl Pts',(0.0052664305215898,-0.0405975531958185,
-0.0108168935806533));
#34037=CARTESIAN_POINT('Ctrl Pts',(0.00539748420550416,-0.0405892245417142,
-0.0107529759235915));
#34038=CARTESIAN_POINT('Ctrl Pts',(0.00547412838128347,-0.0405845083626427,
-0.0107229025251984));
#34039=CARTESIAN_POINT('Ctrl Pts',(0.00559877509581852,-0.0405772712952236,
-0.0106851573210044));
#34040=CARTESIAN_POINT('Ctrl Pts',(0.00564537132426037,-0.0405746545509841,
-0.0106733903033605));
#34041=CARTESIAN_POINT('Ctrl Pts',(0.00571161381318462,-0.0405710645317597,
-0.0106599162518569));
#34042=CARTESIAN_POINT('Ctrl Pts',(0.00573085658234744,-0.0405700366596072,
-0.0106563818151584));
#34043=CARTESIAN_POINT('Ctrl Pts',(0.00576466437083863,-0.0405682562475722,
-0.0106508345574724));
#34044=CARTESIAN_POINT('Ctrl Pts',(0.00577920034588751,-0.0405674989135889,
-0.0106486622328876));
#34045=CARTESIAN_POINT('Ctrl Pts',(0.00580971851370332,-0.0405659253011414,
-0.0106445463007741));
#34046=CARTESIAN_POINT('Ctrl Pts',(0.00582570460195273,-0.0405651103844024,
-0.0106426444725222));
#34047=CARTESIAN_POINT('Ctrl Pts',(0.00586874362620771,-0.0405629399170064,
-0.0106382060835627));
#34048=CARTESIAN_POINT('Ctrl Pts',(0.00589583910960418,-0.0405615984467416,
-0.0106361332559867));
#34049=CARTESIAN_POINT('Ctrl Pts',(0.00604250753895965,-0.0405544492504777,
-0.0106288026954927));
#34050=CARTESIAN_POINT('Ctrl Pts',(0.00616232398331993,-0.040549050050643,
-0.0106367547653879));
#34051=CARTESIAN_POINT('Ctrl Pts',(0.00634446625848518,-0.040540483688935,
-0.0106703677706405));
#34052=CARTESIAN_POINT('Ctrl Pts',(0.00640808321580915,-0.0405374112501371,
-0.010686353286068));
#34053=CARTESIAN_POINT('Ctrl Pts',(0.00648405816422829,-0.0405334481924993,
-0.0107106775967714));
#34054=CARTESIAN_POINT('Ctrl Pts',(0.00649756980070762,-0.0405327316741058,
-0.010715210833702));
#34055=CARTESIAN_POINT('Ctrl Pts',(0.00651927400125313,-0.0405315588967731,
-0.0107228288192166));
#34056=CARTESIAN_POINT('Ctrl Pts',(0.00652750674736777,-0.0405311089228818,
-0.0107257973512768));
#34057=CARTESIAN_POINT('Ctrl Pts',(0.00654388351128701,-0.0405302027661414,
-0.0107318603426371));
#34058=CARTESIAN_POINT('Ctrl Pts',(0.00655202741224689,-0.0405297466170746,
-0.0107349540454444));
#34059=CARTESIAN_POINT('Ctrl Pts',(0.00657340879416736,-0.0405285352403709,
-0.0107432842640634));
#34060=CARTESIAN_POINT('Ctrl Pts',(0.00658660055445618,-0.0405277738395995,
-0.0107486352193798));
#34061=CARTESIAN_POINT('Ctrl Pts',(0.00666077149675907,-0.0405234208719857,
-0.0107799230772966));
#34062=CARTESIAN_POINT('Ctrl Pts',(0.00672010007344723,-0.0405196643354348,
-0.0108095829422025));
#34063=CARTESIAN_POINT('Ctrl Pts',(0.00685064442419358,-0.0405110244120001,
-0.0108857155068935));
#34064=CARTESIAN_POINT('Ctrl Pts',(0.00692030822830832,-0.0405061408877977,
-0.0109344484631835));
#34065=CARTESIAN_POINT('Ctrl Pts',(0.00702316218686836,-0.0404987009356184,
-0.011019838640222));
#34066=CARTESIAN_POINT('Ctrl Pts',(0.00705921345389497,-0.040496039235344,
-0.0110527779329401));
#34067=CARTESIAN_POINT('Ctrl Pts',(0.0071074299575915,-0.0404924080911202,
-0.0111012232446214));
#34068=CARTESIAN_POINT('Ctrl Pts',(0.00712095060435605,-0.0404913811374663,
-0.0111153342500687));
#34069=CARTESIAN_POINT('Ctrl Pts',(0.00714407125483256,-0.0404896087988136,
-0.0111404007577633));
#34070=CARTESIAN_POINT('Ctrl Pts',(0.00715379076095117,-0.0404888584651087,
-0.0111512422020941));
#34071=CARTESIAN_POINT('Ctrl Pts',(0.00717374921729286,-0.0404873058563317,
-0.0111741486894487));
#34072=CARTESIAN_POINT('Ctrl Pts',(0.00718395898396545,-0.0404865048110825,
-0.0111862369605131));
#34073=CARTESIAN_POINT('Ctrl Pts',(0.00721067848335506,-0.0404843884115581,
-0.0112188781181165));
#34074=CARTESIAN_POINT('Ctrl Pts',(0.00722685078702089,-0.0404830862719446,
-0.0112397009972574));
#34075=CARTESIAN_POINT('Ctrl Pts',(0.00731389407794713,-0.0404759351358193,
-0.0113579071945071));
#34076=CARTESIAN_POINT('Ctrl Pts',(0.00737370471020973,-0.0404705085761867,
-0.0114629088327208));
#34077=CARTESIAN_POINT('Ctrl Pts',(0.00744447072214441,-0.0404621319215776,
-0.0116298995096336));
#34078=CARTESIAN_POINT('Ctrl Pts',(0.00746489839236045,-0.0404592819162149,
-0.0116873527649018));
#34079=CARTESIAN_POINT('Ctrl Pts',(0.00748659493362031,-0.0404554479791744,
-0.0117621246470168));
#34080=CARTESIAN_POINT('Ctrl Pts',(0.00749104669321343,-0.0404546024919145,
-0.0117784673287728));
#34081=CARTESIAN_POINT('Ctrl Pts',(0.00749751571499807,-0.0404532728482512,
-0.0118038566373665));
#34082=CARTESIAN_POINT('Ctrl Pts',(0.00749972211588009,-0.0404527985405521,
-0.0118128541260811));
#34083=CARTESIAN_POINT('Ctrl Pts',(0.00750374374615377,-0.040451892289061,
-0.0118299167589125));
#34084=CARTESIAN_POINT('Ctrl Pts',(0.0075055754037722,-0.0404514612376108,
-0.0118379775285717));
#34085=CARTESIAN_POINT('Ctrl Pts',(0.00750995898399796,-0.0404503832093031,
-0.0118580125093438));
#34086=CARTESIAN_POINT('Ctrl Pts',(0.00751243330170728,-0.0404497321888876,
-0.011870003024546));
#34087=CARTESIAN_POINT('Ctrl Pts',(0.00752110556584302,-0.040447286361925,
-0.011914710344225));
#34088=CARTESIAN_POINT('Ctrl Pts',(0.00752638634419614,-0.0404454508780432,
-0.0119475941422348));
#34089=CARTESIAN_POINT('Ctrl Pts',(0.00754497888917948,-0.040437226605193,
-0.012093357462402));
#34090=CARTESIAN_POINT('Ctrl Pts',(0.00754686015598122,-0.0404305949312341,
-0.0122073390250365));
#34091=CARTESIAN_POINT('Ctrl Pts',(0.00753100969887862,-0.0404211283651119,
-0.0123756783733293));
#34092=CARTESIAN_POINT('Ctrl Pts',(0.00752284458999184,-0.040418089782384,
-0.0124305414650205));
#34093=CARTESIAN_POINT('Ctrl Pts',(0.00750765375979262,-0.0404140515349914,
-0.0125048613369007));
#34094=CARTESIAN_POINT('Ctrl Pts',(0.00750316658639405,-0.0404129762687513,
-0.0125247894159469));
#34095=CARTESIAN_POINT('Ctrl Pts',(0.00749474935935628,-0.0404111433315053,
-0.0125589879895818));
#34096=CARTESIAN_POINT('Ctrl Pts',(0.00749100730240655,-0.0404103799286316,
-0.0125733015119272));
#34097=CARTESIAN_POINT('Ctrl Pts',(0.0074828709071067,-0.0404088196240522,
-0.0126026897296793));
#34098=CARTESIAN_POINT('Ctrl Pts',(0.0074784511532174,-0.0404080236265632,
-0.0126177556362907));
#34099=CARTESIAN_POINT('Ctrl Pts',(0.00746631116520551,-0.0404059634079913,
-0.0126569151840046));
#34100=CARTESIAN_POINT('Ctrl Pts',(0.00745822685667998,-0.0404047107968064,
-0.0126808914083417));
#34101=CARTESIAN_POINT('Ctrl Pts',(0.00740805250009144,-0.0403975576465919,
-0.012818428830889));
#34102=CARTESIAN_POINT('Ctrl Pts',(0.00735330142664926,-0.0403920863542759,
-0.012926913522509));
#34103=CARTESIAN_POINT('Ctrl Pts',(0.00725285110060169,-0.0403836684960879,
-0.0130785770801653));
#34104=CARTESIAN_POINT('Ctrl Pts',(0.00721631094840985,-0.0403808201076095,
-0.0131272379060661));
#34105=CARTESIAN_POINT('Ctrl Pts',(0.00716601669639092,-0.0403769876693734,
-0.0131865671440192));
#34106=CARTESIAN_POINT('Ctrl Pts',(0.00715482184829609,-0.0403761395138823,
-0.0131993394338739));
#34107=CARTESIAN_POINT('Ctrl Pts',(0.00713715072272266,-0.0403748035501098,
-0.0132188414827236));
#34108=CARTESIAN_POINT('Ctrl Pts',(0.00713082005269487,-0.0403743254874568,
-0.0132257019154294));
#34109=CARTESIAN_POINT('Ctrl Pts',(0.00711873780685018,-0.0403734131778912,
-0.0132385591514045));
#34110=CARTESIAN_POINT('Ctrl Pts',(0.00711299942685477,-0.0403729798366347,
-0.0132445676076484));
#34111=CARTESIAN_POINT('Ctrl Pts',(0.0070985989195325,-0.0403718927614918,
-0.0132594041062761));
#34112=CARTESIAN_POINT('Ctrl Pts',(0.00708987873219968,-0.0403712348863931,
-0.0132681748030421));
#34113=CARTESIAN_POINT('Ctrl Pts',(0.0070566187878232,-0.0403687305111979,
-0.0133008326219144));
#34114=CARTESIAN_POINT('Ctrl Pts',(0.00703139269156884,-0.0403668409588275,
-0.0133240042320652));
#34115=CARTESIAN_POINT('Ctrl Pts',(0.00692010081944446,-0.0403586214392957,
-0.0134196030894155));
#34116=CARTESIAN_POINT('Ctrl Pts',(0.00682702524387715,-0.0403520626058266,
-0.013483343505906));
#34117=CARTESIAN_POINT('Ctrl Pts',(0.00667920837637894,-0.0403426792068573,
-0.0135624199784625));
#34118=CARTESIAN_POINT('Ctrl Pts',(0.00662921079737098,-0.040339655832678,
-0.0135858128318754));
#34119=CARTESIAN_POINT('Ctrl Pts',(0.00655917756140508,-0.0403356350369595,
-0.0136141106948176));
#34120=CARTESIAN_POINT('Ctrl Pts',(0.00654014170196335,-0.0403345627209437,
-0.0136213673512695));
#34121=CARTESIAN_POINT('Ctrl Pts',(0.00650707195655613,-0.0403327343628347,
-0.013633229335486));
#34122=CARTESIAN_POINT('Ctrl Pts',(0.00649310569013887,-0.0403319726169784,
-0.0136380139190129));
#34123=CARTESIAN_POINT('Ctrl Pts',(0.00646417579907839,-0.0403304154388767,
-0.0136474630909198));
#34124=CARTESIAN_POINT('Ctrl Pts',(0.00644920542371297,-0.0403296209134209,
-0.0136521016053768));
#34125=CARTESIAN_POINT('Ctrl Pts',(0.00640993197412165,-0.0403275643903645,
-0.0136636175800836));
#34126=CARTESIAN_POINT('Ctrl Pts',(0.00638552576299623,-0.0403263139982011,
-0.0136701279567808));
#34127=CARTESIAN_POINT('Ctrl Pts',(0.00623320364824762,-0.0403186601895055,
-0.013706779273515));
#34128=CARTESIAN_POINT('Ctrl Pts',(0.00610204122454998,-0.0403127777734839,
-0.0137210736470574));
#34129=CARTESIAN_POINT('Ctrl Pts',(0.00591345249454654,-0.0403040111900056,
-0.0137174860241215));
#34130=CARTESIAN_POINT('Ctrl Pts',(0.00585636212974602,-0.0403013071018868,
-0.0137132176141899));
#34131=CARTESIAN_POINT('Ctrl Pts',(0.00578588165647265,-0.0402977721336892,
-0.0137039877813217));
#34132=CARTESIAN_POINT('Ctrl Pts',(0.0057721429582911,-0.0402970736313834,
-0.0137019996893812));
#34133=CARTESIAN_POINT('Ctrl Pts',(0.00574987531796092,-0.0402959235191177,
-0.0136984700224787));
#34134=CARTESIAN_POINT('Ctrl Pts',(0.0057413289620749,-0.0402954777799242,
-0.0136970414307356));
#34135=CARTESIAN_POINT('Ctrl Pts',(0.0057251653300398,-0.0402946258109353,
-0.0136941993997607));
#34136=CARTESIAN_POINT('Ctrl Pts',(0.00571754579026297,-0.0402942204276567,
-0.0136928004279197));
#34137=CARTESIAN_POINT('Ctrl Pts',(0.00569662647892313,-0.0402930977046662,
-0.0136887965024294));
#34138=CARTESIAN_POINT('Ctrl Pts',(0.00568335025939411,-0.0402923743131018,
-0.0136860736630137));
#34139=CARTESIAN_POINT('Ctrl Pts',(0.00562415315508727,-0.0402891053116787,
-0.0136731179736892));
#34140=CARTESIAN_POINT('Ctrl Pts',(0.00557868142717328,-0.0402864773429017,
-0.0136609635241214));
#34141=CARTESIAN_POINT('Ctrl Pts',(0.00543821427708631,-0.0402781281298423,
-0.0136164463705754));
#34142=CARTESIAN_POINT('Ctrl Pts',(0.00534576417179183,-0.0402723104351218,
-0.0135768847893157));
#34143=CARTESIAN_POINT('Ctrl Pts',(0.00521155400225171,-0.04026375968715,
-0.0135032512796518));
#34144=CARTESIAN_POINT('Ctrl Pts',(0.00516662819587161,-0.0402608731294837,
-0.0134755166229041));
#34145=CARTESIAN_POINT('Ctrl Pts',(0.00510667925255735,-0.0402569977364808,
-0.013434118176001));
#34146=CARTESIAN_POINT('Ctrl Pts',(0.00509037432770296,-0.0402559409159203,
-0.0134223819368332));
#34147=CARTESIAN_POINT('Ctrl Pts',(0.0050625381934056,-0.0402541310681055,
-0.0134015084539686));
#34148=CARTESIAN_POINT('Ctrl Pts',(0.00505090015735443,-0.0402533726133902,
-0.0133925187033156));
#34149=CARTESIAN_POINT('Ctrl Pts',(0.00502707169803573,-0.0402518153237023,
-0.0133735625070618));
#34150=CARTESIAN_POINT('Ctrl Pts',(0.0050149017174851,-0.0402510175137377,
-0.0133635730575938));
#34151=CARTESIAN_POINT('Ctrl Pts',(0.00498328798146628,-0.0402489370394154,
-0.0133368034064114));
#34152=CARTESIAN_POINT('Ctrl Pts',(0.00496410625415742,-0.0402476665561709,
-0.0133197207388894));
#34153=CARTESIAN_POINT('Ctrl Pts',(0.00486887362719248,-0.0402412991041479,
-0.0132305482003861));
#34154=CARTESIAN_POINT('Ctrl Pts',(0.00479988196266337,-0.0402365091211676,
-0.0131513258032048));
#34155=CARTESIAN_POINT('Ctrl Pts',(0.00469250865091143,-0.0402279443321174,
-0.0129992244577492));
#34156=CARTESIAN_POINT('Ctrl Pts',(0.0046509079311341,-0.0402241865076432,
-0.0129291273235219));
#34157=CARTESIAN_POINT('Ctrl Pts',(0.00460859068870627,-0.0402194246455536,
-0.0128429684761729));
#34158=CARTESIAN_POINT('Ctrl Pts',(0.00460233529864465,-0.040218690819738,
-0.0128297614618998));
#34159=CARTESIAN_POINT('Ctrl Pts',(0.00459260879323672,-0.0402174973655215,
-0.0128084484958542));
#34160=CARTESIAN_POINT('Ctrl Pts',(0.00458901782168303,-0.0402170444771133,
-0.0128003979150007));
#34161=CARTESIAN_POINT('Ctrl Pts',(0.0045820272196626,-0.0402161371802396,
-0.012784357667434));
#34162=CARTESIAN_POINT('Ctrl Pts',(0.00457862566748462,-0.0402156828997755,
-0.0127763692196311));
#34163=CARTESIAN_POINT('Ctrl Pts',(0.0045699320362051,-0.0402144886410961,
-0.012755464747554));
#34164=CARTESIAN_POINT('Ctrl Pts',(0.00456474756445648,-0.0402137428537678,
-0.0127425050729073));
#34165=CARTESIAN_POINT('Ctrl Pts',(0.00453997078154124,-0.0402100132472505,
-0.01267804794355));
#34166=CARTESIAN_POINT('Ctrl Pts',(0.00452297206170388,-0.0402069161419197,
-0.0126256002669764));
#34167=CARTESIAN_POINT('Ctrl Pts',(0.00448478516591968,-0.0401984585186114,
-0.0124819869868053));
#34168=CARTESIAN_POINT('Ctrl Pts',(0.00446901849805195,-0.0401930544215412,
-0.0123896088971841));
#34169=CARTESIAN_POINT('Ctrl Pts',(0.00445857228063263,-0.0401855955796433,
-0.0122562726149411));
#34170=CARTESIAN_POINT('Ctrl Pts',(0.00445700000019507,-0.0401833878786776,
-0.0122160697976288));
#34171=CARTESIAN_POINT('Ctrl Pts',(0.004457,-0.0401812248373849,-0.0121758532940426));
#34172=CARTESIAN_POINT('Ctrl Pts',(0.00510755223020394,-0.0408418305049472,
-0.0112835843270982));
#34173=CARTESIAN_POINT('Ctrl Pts',(0.00540310700475264,-0.0408154711366772,
-0.0109879656812376));
#34174=CARTESIAN_POINT('Ctrl Pts',(0.0063059411121766,-0.0407627550577508,
-0.0107184895915512));
#34175=CARTESIAN_POINT('Ctrl Pts',(0.00739033724866104,-0.0406836822681679,
-0.0116385674487439));
#34176=CARTESIAN_POINT('Ctrl Pts',(0.00720783737929209,-0.0406046121361985,
-0.0130470858798218));
#34177=CARTESIAN_POINT('Ctrl Pts',(0.00592950186608492,-0.0405255420042292,
-0.0136637827569462));
#34178=CARTESIAN_POINT('Ctrl Pts',(0.00471435818957979,-0.0404464718722598,
-0.0129284907266282));
#34179=CARTESIAN_POINT('Ctrl Pts',(0.00466790546059575,-0.0403674017402905,
-0.0115092477749536));
#34180=CARTESIAN_POINT('Ctrl Pts',(0.00583168420583166,-0.0402883316083211,
-0.0106957608437662));
#34181=CARTESIAN_POINT('Ctrl Pts',(0.00714852543999728,-0.0402092614763518,
-0.0112272060724861));
#34182=CARTESIAN_POINT('Ctrl Pts',(0.00742165614668327,-0.0401301913443825,
-0.0126206807356106));
#34183=CARTESIAN_POINT('Ctrl Pts',(0.00640297533227296,-0.0400511212124132,
-0.0136099434274877));
#34184=CARTESIAN_POINT('Ctrl Pts',(0.00501810018683856,-0.0399720510804438,
-0.0132960670082253));
#34185=CARTESIAN_POINT('Ctrl Pts',(0.00452547350724074,-0.0398929809484745,
-0.0119642651766415));
#34186=CARTESIAN_POINT('Ctrl Pts',(0.00537272725475431,-0.0398139108165052,
-0.0108247312644503));
#34187=CARTESIAN_POINT('Ctrl Pts',(0.0067899782676088,-0.0397348406845358,
-0.0109129454936839));
#34188=CARTESIAN_POINT('Ctrl Pts',(0.00748938447730575,-0.0396557705525665,
-0.0121487489266506));
#34189=CARTESIAN_POINT('Ctrl Pts',(0.00683540547876292,-0.0395767004205972,
-0.0134091817184311));
#34190=CARTESIAN_POINT('Ctrl Pts',(0.00542230329908635,-0.0394976302886279,
-0.013548903831367));
#34191=CARTESIAN_POINT('Ctrl Pts',(0.00453414730039512,-0.0394185601566585,
-0.0124409514268199));
#34192=CARTESIAN_POINT('Ctrl Pts',(0.00497799393576915,-0.0393394900246892,
-0.0110921075389659));
#34193=CARTESIAN_POINT('Ctrl Pts',(0.00635052521873909,-0.0392604198927198,
-0.0107280503657344));
#34194=CARTESIAN_POINT('Ctrl Pts',(0.00740453843513532,-0.0391813497607505,
-0.0116795942838205));
#34195=CARTESIAN_POINT('Ctrl Pts',(0.0071822644889926,-0.0391022796287812,
-0.0130820827843013));
#34196=CARTESIAN_POINT('Ctrl Pts',(0.00588568102543133,-0.0390232094968118,
-0.0136610914472305));
#34197=CARTESIAN_POINT('Ctrl Pts',(0.00469297784078796,-0.0389441393648425,
-0.0128904820682789));
#34198=CARTESIAN_POINT('Ctrl Pts',(0.00468794996067798,-0.0388650692328732,
-0.0114704981162847));
#34199=CARTESIAN_POINT('Ctrl Pts',(0.00587516616144298,-0.0387859991009039,
-0.0106914619181288));
#34200=CARTESIAN_POINT('Ctrl Pts',(0.00717581736826139,-0.0387069289689345,
-0.0112612742922497));
#34201=CARTESIAN_POINT('Ctrl Pts',(0.00740801748443278,-0.0386278588369652,
-0.0126621535902753));
#34202=CARTESIAN_POINT('Ctrl Pts',(0.00636076905686384,-0.0385487887049958,
-0.0136211376572347));
#34203=CARTESIAN_POINT('Ctrl Pts',(0.00498569413162669,-0.0384697185730265,
-0.0132668092063614));
#34204=CARTESIAN_POINT('Ctrl Pts',(0.00453230673704881,-0.0383906484410572,
-0.0119211422494873));
#34205=CARTESIAN_POINT('Ctrl Pts',(0.00541259455569142,-0.0383115783090878,
-0.0108069281298219));
#34206=CARTESIAN_POINT('Ctrl Pts',(0.00682665061441721,-0.0382325081771185,
-0.0109366398575666));
#34207=CARTESIAN_POINT('Ctrl Pts',(0.00748953924320393,-0.0381534380451492,
-0.0121924098502718));
#34208=CARTESIAN_POINT('Ctrl Pts',(0.00679890142091577,-0.0380743679131799,
-0.0134331352177383));
#34209=CARTESIAN_POINT('Ctrl Pts',(0.00538231162445055,-0.0379952977812105,
-0.0135313833814939));
#34210=CARTESIAN_POINT('Ctrl Pts',(0.00452700756245122,-0.0379162276492412,
-0.0123978781399435));
#34211=CARTESIAN_POINT('Ctrl Pts',(0.00501019450630097,-0.0378371575172719,
-0.0110626206513034));
#34212=CARTESIAN_POINT('Ctrl Pts',(0.0063928048011601,-0.0377580873853025,
-0.0107389460890354));
#34213=CARTESIAN_POINT('Ctrl Pts',(0.00741848003443745,-0.0376790172533332,
-0.0117209682272295));
#34214=CARTESIAN_POINT('Ctrl Pts',(0.00715519574970712,-0.0375999471213639,
-0.0131163459396875));
#34215=CARTESIAN_POINT('Ctrl Pts',(0.00584220638794218,-0.0375208769893944,
-0.0136570956147497));
#34216=CARTESIAN_POINT('Ctrl Pts',(0.00467258771297713,-0.0374418068574252,
-0.0128518849746824));
#34217=CARTESIAN_POINT('Ctrl Pts',(0.00470920090848562,-0.0373627367254559,
-0.0114323201325417));
#34218=CARTESIAN_POINT('Ctrl Pts',(0.00591869234964484,-0.0372836665934865,
-0.0106884972982332));
#34219=CARTESIAN_POINT('Ctrl Pts',(0.00720217534268384,-0.0372045964615172,
-0.0112960166958557));
#34220=CARTESIAN_POINT('Ctrl Pts',(0.00739304429033509,-0.0371255263295479,
-0.0127034247991513));
#34221=CARTESIAN_POINT('Ctrl Pts',(0.0063184850578249,-0.0370464561975785,
-0.0136306675820344));
#34222=CARTESIAN_POINT('Ctrl Pts',(0.00495370982778676,-0.0369673860656093,
-0.0132374514271274));
#34223=CARTESIAN_POINT('Ctrl Pts',(0.00454129505257269,-0.0368883158002724,
-0.0118764800191924));
#34224=CARTESIAN_POINT('Ctrl Pts',(0.00514779084977581,-0.0368356022455921,
-0.0111555318307725));
#34225=CARTESIAN_POINT('Ctrl Pts',(0.00553656972522908,-0.0368092454015681,
-0.0110020392895787));
#34226=CARTESIAN_POINT('Ctrl Pts',(0.00504057926485683,-0.0408965082243162,
-0.011216624780417));
#34227=CARTESIAN_POINT('Ctrl Pts',(0.00535831368996204,-0.0408701488560462,
-0.0108988216908329));
#34228=CARTESIAN_POINT('Ctrl Pts',(0.00632890019639147,-0.0408174327771198,
-0.0106091230027746));
#34229=CARTESIAN_POINT('Ctrl Pts',(0.00749467389616782,-0.0407383599875368,
-0.0115982473011506));
#34230=CARTESIAN_POINT('Ctrl Pts',(0.00729847848310348,-0.0406592898555674,
-0.0131124667707295));
#34231=CARTESIAN_POINT('Ctrl Pts',(0.00592421139504614,-0.0405802197235982,
-0.0137754431277062));
#34232=CARTESIAN_POINT('Ctrl Pts',(0.00461787832002084,-0.0405011495916288,
-0.0129849717475897));
#34233=CARTESIAN_POINT('Ctrl Pts',(0.0045679395864617,-0.0404220794596595,
-0.0114592229451094));
#34234=CARTESIAN_POINT('Ctrl Pts',(0.00581905309370203,-0.0403430093276902,
-0.0105846885959143));
#34235=CARTESIAN_POINT('Ctrl Pts',(0.00723471553099929,-0.0402639391957208,
-0.0111560156688065));
#34236=CARTESIAN_POINT('Ctrl Pts',(0.00752834309360578,-0.0401848690637515,
-0.0126540624239728));
#34237=CARTESIAN_POINT('Ctrl Pts',(0.00643321626499464,-0.0401057989317822,
-0.0137175634726755));
#34238=CARTESIAN_POINT('Ctrl Pts',(0.00494441437083125,-0.0400267287998128,
-0.0133801324709917));
#34239=CARTESIAN_POINT('Ctrl Pts',(0.00441481895125976,-0.0399476586678434,
-0.0119483867312771));
#34240=CARTESIAN_POINT('Ctrl Pts',(0.00532565411809312,-0.0398685885358742,
-0.0107233374894542));
#34241=CARTESIAN_POINT('Ctrl Pts',(0.00684926149843999,-0.0397895184039048,
-0.0108181716786648));
#34242=CARTESIAN_POINT('Ctrl Pts',(0.00760115403779219,-0.0397104482719355,
-0.0121467149035757));
#34243=CARTESIAN_POINT('Ctrl Pts',(0.0068980977550771,-0.0396313781399662,
-0.0135017357760746));
#34244=CARTESIAN_POINT('Ctrl Pts',(0.00537895055347951,-0.0395523080079968,
-0.0136519432132442));
#34245=CARTESIAN_POINT('Ctrl Pts',(0.00442414366166439,-0.0394732378760275,
-0.0124608454857914));
#34246=CARTESIAN_POINT('Ctrl Pts',(0.0049012983810927,-0.0393941677440582,
-0.0110107787835418));
#34247=CARTESIAN_POINT('Ctrl Pts',(0.00637683007838732,-0.0393150976120888,
-0.0106194012569266));
#34248=CARTESIAN_POINT('Ctrl Pts',(0.00750994079830842,-0.0392360274801195,
-0.0116423529593213));
#34249=CARTESIAN_POINT('Ctrl Pts',(0.00727098649753159,-0.0391569573481502,
-0.0131500899874149));
#34250=CARTESIAN_POINT('Ctrl Pts',(0.00587710205758417,-0.0390778872161808,
-0.0137725498509977));
#34251=CARTESIAN_POINT('Ctrl Pts',(0.00459489350158125,-0.0389988170842115,
-0.0129441107625892));
#34252=CARTESIAN_POINT('Ctrl Pts',(0.0045894883085889,-0.0389197469522422,
-0.0114175653520659));
#34253=CARTESIAN_POINT('Ctrl Pts',(0.00586579811478878,-0.0388406768202728,
-0.0105800670611478));
#34254=CARTESIAN_POINT('Ctrl Pts',(0.00726405555824212,-0.0387616066883035,
-0.0111926405084406));
#34255=CARTESIAN_POINT('Ctrl Pts',(0.00751368092982937,-0.0386825365563341,
-0.0126986475728829));
#34256=CARTESIAN_POINT('Ctrl Pts',(0.00638784265641935,-0.0386034664243649,
-0.013729597763641));
#34257=CARTESIAN_POINT('Ctrl Pts',(0.00490957643143956,-0.0385243962923955,
-0.0133486790428774));
#34258=CARTESIAN_POINT('Ctrl Pts',(0.00442216497484537,-0.0384453261604262,
-0.0119020276816251));
#34259=CARTESIAN_POINT('Ctrl Pts',(0.00536851322589506,-0.0383662560284569,
-0.0107041983340985));
#34260=CARTESIAN_POINT('Ctrl Pts',(0.00688868588956419,-0.0382871858964875,
-0.0108436441654417));
#34261=CARTESIAN_POINT('Ctrl Pts',(0.00760132041796233,-0.0382081157645182,
-0.0121936523231709));
#34262=CARTESIAN_POINT('Ctrl Pts',(0.00685885428201276,-0.0381290456325488,
-0.013527486844868));
#34263=CARTESIAN_POINT('Ctrl Pts',(0.00533595773846292,-0.0380499755005795,
-0.0136331079564748));
#34264=CARTESIAN_POINT('Ctrl Pts',(0.00441646812830693,-0.0379709053686102,
-0.0124145398016286));
#34265=CARTESIAN_POINT('Ctrl Pts',(0.00493591541538556,-0.0378918352366409,
-0.0109790790780847));
#34266=CARTESIAN_POINT('Ctrl Pts',(0.00642228249523544,-0.0378127651046715,
-0.01063111464029));
#34267=CARTESIAN_POINT('Ctrl Pts',(0.00752492863278372,-0.0377336949727022,
-0.0116868317742668));
#34268=CARTESIAN_POINT('Ctrl Pts',(0.00724188640828986,-0.0376546248407329,
-0.0131869243914458));
#34269=CARTESIAN_POINT('Ctrl Pts',(0.0058303649038016,-0.0375755547087635,
-0.0137682541547496));
#34270=CARTESIAN_POINT('Ctrl Pts',(0.00457297321439364,-0.0374964845767942,
-0.0129026171837311));
#34271=CARTESIAN_POINT('Ctrl Pts',(0.00461233401526018,-0.0374174144448248,
-0.011376522334795));
#34272=CARTESIAN_POINT('Ctrl Pts',(0.00591259068786246,-0.0373383443128556,
-0.010576879963935));
#34273=CARTESIAN_POINT('Ctrl Pts',(0.00729239154389094,-0.0372592741808862,
-0.0112299901254563));
#34274=CARTESIAN_POINT('Ctrl Pts',(0.00749758408542575,-0.0371802040489169,
-0.0127430159436719));
#34275=CARTESIAN_POINT('Ctrl Pts',(0.00634238549151208,-0.0371011339169475,
-0.0137398428533443));
#34276=CARTESIAN_POINT('Ctrl Pts',(0.004875191893384,-0.0370220637849782,
-0.0133171181346785));
#34277=CARTESIAN_POINT('Ctrl Pts',(0.00443182781067669,-0.0369429935196414,
-0.0118540138131692));
#34278=CARTESIAN_POINT('Ctrl Pts',(0.00508383755657679,-0.0368902799649611,
-0.011078962696069));
#34279=CARTESIAN_POINT('Ctrl Pts',(0.00550179200401839,-0.0368639231209372,
-0.0109139514408505));
#34280=CARTESIAN_POINT('Ctrl Pts',(0.0049736062995096,-0.0409511859436854,
-0.0111496652337357));
#34281=CARTESIAN_POINT('Ctrl Pts',(0.00531352037517144,-0.0409248265754152,
-0.0108096777004281));
#34282=CARTESIAN_POINT('Ctrl Pts',(0.00635185928060625,-0.0408721104964888,
-0.0104997564139979));
#34283=CARTESIAN_POINT('Ctrl Pts',(0.00759901054367472,-0.0407930377069059,
-0.0115579271535574));
#34284=CARTESIAN_POINT('Ctrl Pts',(0.00738911958691479,-0.0407139675749367,
-0.0131778476616374));
#34285=CARTESIAN_POINT('Ctrl Pts',(0.00591892092400736,-0.0406348974429673,
-0.0138871034984661));
#34286=CARTESIAN_POINT('Ctrl Pts',(0.0045213984504619,-0.040555827310998,
-0.0130414527685509));
#34287=CARTESIAN_POINT('Ctrl Pts',(0.00446797371232754,-0.0404767571790286,
-0.0114091981152651));
#34288=CARTESIAN_POINT('Ctrl Pts',(0.00580642198157228,-0.0403976870470593,
-0.0104736163480623));
#34289=CARTESIAN_POINT('Ctrl Pts',(0.00732090562200129,-0.0403186169150899,
-0.011084825265127));
#34290=CARTESIAN_POINT('Ctrl Pts',(0.0076350300405283,-0.0402395467831207,
-0.0126874441123349));
#34291=CARTESIAN_POINT('Ctrl Pts',(0.00646345719771645,-0.0401604766511513,
-0.0138251835178632));
#34292=CARTESIAN_POINT('Ctrl Pts',(0.00487072855482406,-0.040081406519182,
-0.0134641979337579));
#34293=CARTESIAN_POINT('Ctrl Pts',(0.00430416439527867,-0.0400023363872126,
-0.0119325082859126));
#34294=CARTESIAN_POINT('Ctrl Pts',(0.00527858098143203,-0.0399232662552434,
-0.0106219437144581));
#34295=CARTESIAN_POINT('Ctrl Pts',(0.00690854472927117,-0.039844196123274,
-0.0107233978636457));
#34296=CARTESIAN_POINT('Ctrl Pts',(0.00771292359827863,-0.0397651259913046,
-0.0121446808805009));
#34297=CARTESIAN_POINT('Ctrl Pts',(0.0069607900313913,-0.0396860558593353,
-0.0135942898337181));
#34298=CARTESIAN_POINT('Ctrl Pts',(0.00533559780787254,-0.039606985727366,
-0.0137549825951213));
#34299=CARTESIAN_POINT('Ctrl Pts',(0.00431414002293365,-0.0395279155953967,
-0.012480739544763));
#34300=CARTESIAN_POINT('Ctrl Pts',(0.00482460282641615,-0.0394488454634273,
-0.0109294500281175));
#34301=CARTESIAN_POINT('Ctrl Pts',(0.00640313493803564,-0.039369775331458,
-0.0105107521481187));
#34302=CARTESIAN_POINT('Ctrl Pts',(0.0076153431614815,-0.0392907051994886,
-0.0116051116348221));
#34303=CARTESIAN_POINT('Ctrl Pts',(0.00735970850607058,-0.0392116350675194,
-0.0132180971905287));
#34304=CARTESIAN_POINT('Ctrl Pts',(0.00586852308973702,-0.03913256493555,
-0.0138840082547647));
#34305=CARTESIAN_POINT('Ctrl Pts',(0.00449680916237462,-0.0390534948035806,
-0.0129977394568994));
#34306=CARTESIAN_POINT('Ctrl Pts',(0.00449102665649993,-0.0389744246716113,
-0.0113646325878472));
#34307=CARTESIAN_POINT('Ctrl Pts',(0.00585643006813467,-0.0388953545396419,
-0.0104686722041668));
#34308=CARTESIAN_POINT('Ctrl Pts',(0.00735229374822285,-0.0388162844076727,
-0.0111240067246316));
#34309=CARTESIAN_POINT('Ctrl Pts',(0.00761934437522596,-0.0387372142757033,
-0.0127351415554907));
#34310=CARTESIAN_POINT('Ctrl Pts',(0.00641491625597485,-0.038658144143734,
-0.0138380578700472));
#34311=CARTESIAN_POINT('Ctrl Pts',(0.00483345873125242,-0.0385790740117646,
-0.0134305488793935));
#34312=CARTESIAN_POINT('Ctrl Pts',(0.00431202321264183,-0.0385000038797954,
-0.0118829131137628));
#34313=CARTESIAN_POINT('Ctrl Pts',(0.00532443189609871,-0.038420933747826,
-0.0106014685383751));
#34314=CARTESIAN_POINT('Ctrl Pts',(0.00695072116471118,-0.0383418636158567,
-0.0107506484733166));
#34315=CARTESIAN_POINT('Ctrl Pts',(0.00771310159272074,-0.0382627934838874,
-0.01219489479607));
#34316=CARTESIAN_POINT('Ctrl Pts',(0.00691880714310953,-0.038183723351918,
-0.0136218384719977));
#34317=CARTESIAN_POINT('Ctrl Pts',(0.00528960385247539,-0.0381046532199487,
-0.0137348325314557));
#34318=CARTESIAN_POINT('Ctrl Pts',(0.00430592869416266,-0.0380255830879794,
-0.0124312014633137));
#34319=CARTESIAN_POINT('Ctrl Pts',(0.00486163632447015,-0.03794651295601,
-0.0108955375048661));
#34320=CARTESIAN_POINT('Ctrl Pts',(0.0064517601893108,-0.0378674428240407,
-0.0105232831915444));
#34321=CARTESIAN_POINT('Ctrl Pts',(0.00763137723112998,-0.0377883726920714,
-0.0116526953213039));
#34322=CARTESIAN_POINT('Ctrl Pts',(0.0073285770668726,-0.037709302560102,
-0.013257502843204));
#34323=CARTESIAN_POINT('Ctrl Pts',(0.00581852341966102,-0.0376302324281327,
-0.0138794126947496));
#34324=CARTESIAN_POINT('Ctrl Pts',(0.00447335871581017,-0.0375511622961633,
-0.0129533493927798));
#34325=CARTESIAN_POINT('Ctrl Pts',(0.00451546712203466,-0.0374720921641941,
-0.0113207245370486));
#34326=CARTESIAN_POINT('Ctrl Pts',(0.00590648902608009,-0.0373930220322247,
-0.0104652626296369));
#34327=CARTESIAN_POINT('Ctrl Pts',(0.00738260774509806,-0.0373139519002554,
-0.0111639635550568));
#34328=CARTESIAN_POINT('Ctrl Pts',(0.00760212388051653,-0.037234881768286,
-0.0127826070881925));
#34329=CARTESIAN_POINT('Ctrl Pts',(0.00636628592519926,-0.0371558116363166,
-0.0138490181246544));
#34330=CARTESIAN_POINT('Ctrl Pts',(0.00479667395898134,-0.0370767415043474,
-0.0133967848422295));
#34331=CARTESIAN_POINT('Ctrl Pts',(0.00432236056878079,-0.0369976712390105,
-0.011831547607146));
#34332=CARTESIAN_POINT('Ctrl Pts',(0.00501988426337788,-0.0369449576843301,
-0.0110023935613656));
#34333=CARTESIAN_POINT('Ctrl Pts',(0.0054670142828077,-0.0369186008403063,
-0.010825863592122));
#34334=CARTESIAN_POINT('Ctrl Pts',(0.0049066333341625,-0.0410058636630544,
-0.0110827056870545));
#34335=CARTESIAN_POINT('Ctrl Pts',(0.00526872706038073,-0.0409795042947844,
-0.0107205337100233));
#34336=CARTESIAN_POINT('Ctrl Pts',(0.00637481836482103,-0.0409267882158579,
-0.0103903898252213));
#34337=CARTESIAN_POINT('Ctrl Pts',(0.00770334719118149,-0.040847715426275,
-0.0115176070059642));
#34338=CARTESIAN_POINT('Ctrl Pts',(0.00747976069072619,-0.0407686452943056,
-0.0132432285525452));
#34339=CARTESIAN_POINT('Ctrl Pts',(0.00591363045296858,-0.0406895751623363,
-0.0139987638692261));
#34340=CARTESIAN_POINT('Ctrl Pts',(0.00442491858090285,-0.040610505030367,
-0.0130979337895123));
#34341=CARTESIAN_POINT('Ctrl Pts',(0.0043680078381935,-0.0405314348983977,
-0.0113591732854209));
#34342=CARTESIAN_POINT('Ctrl Pts',(0.00579379086944254,-0.0404523647664283,
-0.0103625441002104));
#34343=CARTESIAN_POINT('Ctrl Pts',(0.0074070957130034,-0.0403732946344591,
-0.0110136348614473));
#34344=CARTESIAN_POINT('Ctrl Pts',(0.00774171698745092,-0.0402942245024896,
-0.0127208258006971));
#34345=CARTESIAN_POINT('Ctrl Pts',(0.00649369813043813,-0.0402151543705203,
-0.013932803563051));
#34346=CARTESIAN_POINT('Ctrl Pts',(0.00479704273881685,-0.0401360842385509,
-0.0135482633965242));
#34347=CARTESIAN_POINT('Ctrl Pts',(0.00419350983929769,-0.0400570141065816,
-0.0119166298405482));
#34348=CARTESIAN_POINT('Ctrl Pts',(0.00523150784477083,-0.0399779439746123,
-0.0105205499394621));
#34349=CARTESIAN_POINT('Ctrl Pts',(0.00696782796010235,-0.0398988738426429,
-0.0106286240486267));
#34350=CARTESIAN_POINT('Ctrl Pts',(0.00782469315876507,-0.0398198037106736,
-0.0121426468574261));
#34351=CARTESIAN_POINT('Ctrl Pts',(0.00702348230770549,-0.0397407335787043,
-0.0136868438913615));
#34352=CARTESIAN_POINT('Ctrl Pts',(0.00529224506226558,-0.039661663446735,
-0.0138580219769984));
#34353=CARTESIAN_POINT('Ctrl Pts',(0.00420413638420291,-0.0395825933147656,
-0.0125006336037345));
#34354=CARTESIAN_POINT('Ctrl Pts',(0.0047479072717396,-0.0395035231827963,
-0.0108481212726933));
#34355=CARTESIAN_POINT('Ctrl Pts',(0.00642943979768396,-0.0394244530508269,
-0.0104021030393109));
#34356=CARTESIAN_POINT('Ctrl Pts',(0.0077207455246546,-0.0393453829188576,
-0.011567870310323));
#34357=CARTESIAN_POINT('Ctrl Pts',(0.00744843051460957,-0.0392663127868883,
-0.0132861043936424));
#34358=CARTESIAN_POINT('Ctrl Pts',(0.00585994412188996,-0.039187242654919,
-0.0139954666585319));
#34359=CARTESIAN_POINT('Ctrl Pts',(0.00439872482316802,-0.0391081725229496,
-0.0130513681512097));
#34360=CARTESIAN_POINT('Ctrl Pts',(0.00439256500441095,-0.0390291023909803,
-0.0113116998236284));
#34361=CARTESIAN_POINT('Ctrl Pts',(0.00584706202148047,-0.038950032259011,
-0.0103572773471858));
#34362=CARTESIAN_POINT('Ctrl Pts',(0.00744053193820359,-0.0388709621270416,
-0.0110553729408225));
#34363=CARTESIAN_POINT('Ctrl Pts',(0.00772500782062244,-0.0387918919950723,
-0.0127716355380983));
#34364=CARTESIAN_POINT('Ctrl Pts',(0.00644198985553047,-0.038712821863103,
-0.0139465179764535));
#34365=CARTESIAN_POINT('Ctrl Pts',(0.00475734103106529,-0.0386337517311336,
-0.0135124187159094));
#34366=CARTESIAN_POINT('Ctrl Pts',(0.0042018814504384,-0.0385546815991643,
-0.0118637985459005));
#34367=CARTESIAN_POINT('Ctrl Pts',(0.00528035056630226,-0.038475611467195,
-0.0104987387426518));
#34368=CARTESIAN_POINT('Ctrl Pts',(0.00701275643985817,-0.0383965413352256,
-0.0106576527811916));
#34369=CARTESIAN_POINT('Ctrl Pts',(0.00782488276747915,-0.0383174712032563,
-0.0121961372689691));
#34370=CARTESIAN_POINT('Ctrl Pts',(0.00697876000420641,-0.038238401071287,
-0.0137161900991274));
#34371=CARTESIAN_POINT('Ctrl Pts',(0.00524324996648776,-0.0381593309393176,
-0.0138365571064366));
#34372=CARTESIAN_POINT('Ctrl Pts',(0.00419538926001839,-0.0380802608073483,
-0.0124478631249988));
#34373=CARTESIAN_POINT('Ctrl Pts',(0.00478735723355475,-0.038001190675379,
-0.0108119959316474));
#34374=CARTESIAN_POINT('Ctrl Pts',(0.00648123788338614,-0.0379221205434096,
-0.010415451742799));
#34375=CARTESIAN_POINT('Ctrl Pts',(0.00773782582947614,-0.0378430504114403,
-0.0116185588683412));
#34376=CARTESIAN_POINT('Ctrl Pts',(0.00741526772545535,-0.037763980279471,
-0.0133280812949623));
#34377=CARTESIAN_POINT('Ctrl Pts',(0.00580668193552033,-0.0376849101475016,
-0.0139905712347495));
#34378=CARTESIAN_POINT('Ctrl Pts',(0.00437374421722668,-0.0376058400155324,
-0.0130040816018285));
#34379=CARTESIAN_POINT('Ctrl Pts',(0.00441860022880923,-0.037526769883563,
-0.0112649267393021));
#34380=CARTESIAN_POINT('Ctrl Pts',(0.00590038736429771,-0.0374476997515936,
-0.0103536452953387));
#34381=CARTESIAN_POINT('Ctrl Pts',(0.00747282394630516,-0.0373686296196243,
-0.0110979369846573));
#34382=CARTESIAN_POINT('Ctrl Pts',(0.0077066636756073,-0.037289559487655,
-0.0128221982327131));
#34383=CARTESIAN_POINT('Ctrl Pts',(0.00639018635888645,-0.0372104893556857,
-0.0139581933959644));
#34384=CARTESIAN_POINT('Ctrl Pts',(0.00471815602457857,-0.0371314192237164,
-0.0134764515497806));
#34385=CARTESIAN_POINT('Ctrl Pts',(0.00421289332688479,-0.0370523489583796,
-0.0118090814011229));
#34386=CARTESIAN_POINT('Ctrl Pts',(0.00495593097017897,-0.0369996354036992,
-0.0109258244266621));
#34387=CARTESIAN_POINT('Ctrl Pts',(0.00543223656159701,-0.0369732785596753,
-0.0107377757433937));
#34388=CARTESIAN_POINT('',(0.00445700003781045,-0.0405679514195094,-0.0121755116975483));
#34389=CARTESIAN_POINT('Ctrl Pts',(0.00445700003781045,-0.0405679514195094,
-0.0121755116975483));
#34390=CARTESIAN_POINT('Ctrl Pts',(0.00445700301761374,-0.0405672476957248,
-0.0121620515561686));
#34391=CARTESIAN_POINT('Ctrl Pts',(0.00445718212343988,-0.0405665385763963,
-0.0121485923059843));
#34392=CARTESIAN_POINT('Ctrl Pts',(0.00445802931760553,-0.0405648343653531,
-0.0121164975946681));
#34393=CARTESIAN_POINT('Ctrl Pts',(0.00445885916667054,-0.0405638345050433,
-0.0120978688272803));
#34394=CARTESIAN_POINT('Ctrl Pts',(0.00446660927761155,-0.0405571317217464,
-0.0119743096298569));
#34395=CARTESIAN_POINT('Ctrl Pts',(0.00448390293192045,-0.0405511225439535,
-0.0118703186347209));
#34396=CARTESIAN_POINT('Ctrl Pts',(0.00452569449924638,-0.0405420351721237,
-0.0117174689997002));
#34397=CARTESIAN_POINT('Ctrl Pts',(0.00454241680909747,-0.0405389832279566,
-0.0116667908739223));
#34398=CARTESIAN_POINT('Ctrl Pts',(0.00457283306441903,-0.0405342953142253,
-0.0115885002902892));
#34399=CARTESIAN_POINT('Ctrl Pts',(0.0045847859545511,-0.0405326102753515,
-0.0115602572874876));
#34400=CARTESIAN_POINT('Ctrl Pts',(0.00460233303742628,-0.0405303548848834,
-0.0115220135971565));
#34401=CARTESIAN_POINT('Ctrl Pts',(0.00460720800297794,-0.0405297489031321,
-0.0115116923528811));
#34402=CARTESIAN_POINT('Ctrl Pts',(0.00461571486029345,-0.0405287269962117,
-0.0114941873700126));
#34403=CARTESIAN_POINT('Ctrl Pts',(0.00461928918985885,-0.0405283077731754,
-0.0114869763462131));
#34404=CARTESIAN_POINT('Ctrl Pts',(0.0046270987701427,-0.0405274136454441,
-0.0114715259314694));
#34405=CARTESIAN_POINT('Ctrl Pts',(0.00463135201963233,-0.0405269398170757,
-0.0114632962542935));
#34406=CARTESIAN_POINT('Ctrl Pts',(0.00464364934464731,-0.040525605133667,
-0.0114400183630903));
#34407=CARTESIAN_POINT('Ctrl Pts',(0.00465186946591345,-0.0405247543672459,
-0.0114250642069838));
#34408=CARTESIAN_POINT('Ctrl Pts',(0.00469296533736947,-0.0405206812399618,
-0.0113531541550091));
#34409=CARTESIAN_POINT('Ctrl Pts',(0.00472921379575197,-0.0405176221086522,
-0.0112981988720777));
#34410=CARTESIAN_POINT('Ctrl Pts',(0.00481868615956656,-0.0405107910158406,
-0.0111797717459593));
#34411=CARTESIAN_POINT('Ctrl Pts',(0.00487372973224963,-0.0405070438407399,
-0.0111179327794487));
#34412=CARTESIAN_POINT('Ctrl Pts',(0.0049682166488859,-0.0405008789541652,
-0.011027556517288));
#34413=CARTESIAN_POINT('Ctrl Pts',(0.0050045073728012,-0.0404985657521315,
-0.0109959565641567));
#34414=CARTESIAN_POINT('Ctrl Pts',(0.00505724066377667,-0.0404952359539612,
-0.010954206350628));
#34415=CARTESIAN_POINT('Ctrl Pts',(0.00507248857654536,-0.04049427673922,
-0.0109425897621374));
#34416=CARTESIAN_POINT('Ctrl Pts',(0.00509940407724372,-0.0404925875743147,
-0.0109228657824191));
#34417=CARTESIAN_POINT('Ctrl Pts',(0.00511097472269373,-0.0404918626853937,
-0.0109146297772545));
#34418=CARTESIAN_POINT('Ctrl Pts',(0.00513527106277933,-0.0404903423847992,
-0.0108978360752631));
#34419=CARTESIAN_POINT('Ctrl Pts',(0.00514801390652434,-0.0404895460433777,
-0.0108893060463693));
#34420=CARTESIAN_POINT('Ctrl Pts',(0.00518205914660631,-0.0404874203061145,
-0.0108672438743938));
#34421=CARTESIAN_POINT('Ctrl Pts',(0.00520356940942222,-0.0404860790587345,
-0.0108540423893678));
#34422=CARTESIAN_POINT('Ctrl Pts',(0.00533579934686101,-0.0404778423415594,
-0.0107772886264239));
#34423=CARTESIAN_POINT('Ctrl Pts',(0.00545371997776377,-0.040470473157869,
-0.0107271592989575));
#34424=CARTESIAN_POINT('Ctrl Pts',(0.00563634119169197,-0.0404596098027992,
-0.0106750261729495));
#34425=CARTESIAN_POINT('Ctrl Pts',(0.00569722955898793,-0.0404560839389985,
-0.0106615676297317));
#34426=CARTESIAN_POINT('Ctrl Pts',(0.005772470192972,-0.0404519653661404,
-0.0106496581444446));
#34427=CARTESIAN_POINT('Ctrl Pts',(0.00578620044358163,-0.0404512234567575,
-0.0106476742392438));
#34428=CARTESIAN_POINT('Ctrl Pts',(0.00580837411008537,-0.0404500428994715,
-0.010644775041075));
#34429=CARTESIAN_POINT('Ctrl Pts',(0.00581680132489728,-0.040449598302531,
-0.0106437438493416));
#34430=CARTESIAN_POINT('Ctrl Pts',(0.00583360070876016,-0.0404487207200846,
-0.0106418287953362));
#34431=CARTESIAN_POINT('Ctrl Pts',(0.00584197242801135,-0.0404482876957185,
-0.0106409437922207));
#34432=CARTESIAN_POINT('Ctrl Pts',(0.00586383724602124,-0.0404471670186347,
-0.0106388131743079));
#34433=CARTESIAN_POINT('Ctrl Pts',(0.00587734051983284,-0.0404464851002116,
-0.010637676678446));
#34434=CARTESIAN_POINT('Ctrl Pts',(0.00594227547400257,-0.0404432474614542,
-0.0106330720357617));
#34435=CARTESIAN_POINT('Ctrl Pts',(0.00599384813652307,-0.0404408006717884,
-0.0106320044958175));
#34436=CARTESIAN_POINT('Ctrl Pts',(0.00614361500215606,-0.0404338229875484,
-0.0106364111776378));
#34437=CARTESIAN_POINT('Ctrl Pts',(0.00624134770538443,-0.0404294158626033,
-0.0106486796896947));
#34438=CARTESIAN_POINT('Ctrl Pts',(0.00638823661725556,-0.0404223508074989,
-0.0106815804683772));
#34439=CARTESIAN_POINT('Ctrl Pts',(0.0064386054520579,-0.0404198483817655,
-0.0106955818395151));
#34440=CARTESIAN_POINT('Ctrl Pts',(0.00650681854332323,-0.0404162939743058,
-0.0107183311998621));
#34441=CARTESIAN_POINT('Ctrl Pts',(0.00652535120527398,-0.0404153111816445,
-0.0107249081682775));
#34442=CARTESIAN_POINT('Ctrl Pts',(0.00655710121066071,-0.0404135954396204,
-0.0107368638176332));
#34443=CARTESIAN_POINT('Ctrl Pts',(0.00657037915965547,-0.0404128680815828,
-0.0107420750446032));
#34444=CARTESIAN_POINT('Ctrl Pts',(0.00659758083910213,-0.0404113568610635,
-0.0107531886044942));
#34445=CARTESIAN_POINT('Ctrl Pts',(0.00661149382758474,-0.0404105723150985,
-0.0107591130372277));
#34446=CARTESIAN_POINT('Ctrl Pts',(0.00664747666319189,-0.0404085121191546,
-0.0107750640417832));
#34447=CARTESIAN_POINT('Ctrl Pts',(0.00666940069386643,-0.0404072258642573,
-0.0107854076169645));
#34448=CARTESIAN_POINT('Ctrl Pts',(0.00679577104057577,-0.0403996267428555,
-0.0108487096745987));
#34449=CARTESIAN_POINT('Ctrl Pts',(0.00689414695991099,-0.0403929195475568,
-0.0109128982910897));
#34450=CARTESIAN_POINT('Ctrl Pts',(0.00702318350109659,-0.0403833073684436,
-0.0110197851465529));
#34451=CARTESIAN_POINT('Ctrl Pts',(0.00706046201418208,-0.0403804216564015,
-0.0110538823623851));
#34452=CARTESIAN_POINT('Ctrl Pts',(0.00711687587008837,-0.04037595238858,
-0.0111108102703621));
#34453=CARTESIAN_POINT('Ctrl Pts',(0.00713713856100051,-0.0403743240875982,
-0.0111324720352807));
#34454=CARTESIAN_POINT('Ctrl Pts',(0.00716421219055398,-0.0403721320234571,
-0.0111631412882262));
#34455=CARTESIAN_POINT('Ctrl Pts',(0.00717156666670154,-0.0403715347956552,
-0.0111716584965681));
#34456=CARTESIAN_POINT('Ctrl Pts',(0.00718399166949294,-0.0403705239276032,
-0.0111863701978207));
#34457=CARTESIAN_POINT('Ctrl Pts',(0.00718910825526529,-0.0403701071261388,
-0.0111925249469508));
#34458=CARTESIAN_POINT('Ctrl Pts',(0.00720006800680869,-0.0403692134634119,
-0.0112059191055391));
#34459=CARTESIAN_POINT('Ctrl Pts',(0.00720589390455731,-0.0403687377556948,
-0.011213171908399));
#34460=CARTESIAN_POINT('Ctrl Pts',(0.00722235105476872,-0.0403673906434058,
-0.0112340436578774));
#34461=CARTESIAN_POINT('Ctrl Pts',(0.00723281992394978,-0.0403665296495844,
-0.011247789410233));
#34462=CARTESIAN_POINT('Ctrl Pts',(0.0072842819686224,-0.0403622606215341,
-0.0113177676206833));
#34463=CARTESIAN_POINT('Ctrl Pts',(0.00732167195999868,-0.0403590357549089,
-0.0113765560972033));
#34464=CARTESIAN_POINT('Ctrl Pts',(0.00738531630127132,-0.0403529227231774,
-0.0114933783939187));
#34465=CARTESIAN_POINT('Ctrl Pts',(0.00741220053659239,-0.0403500354241956,
-0.0115509030932052));
#34466=CARTESIAN_POINT('Ctrl Pts',(0.00745748577726506,-0.0403442809440113,
-0.0116657668982553));
#34467=CARTESIAN_POINT('Ctrl Pts',(0.00747622470702912,-0.0403414259387455,
-0.0117228492555738));
#34468=CARTESIAN_POINT('Ctrl Pts',(0.0074968372540085,-0.0403374541892639,
-0.0118006900942998));
#34469=CARTESIAN_POINT('Ctrl Pts',(0.00750168891075866,-0.0403364315077939,
-0.0118206075240896));
#34470=CARTESIAN_POINT('Ctrl Pts',(0.00750927442345102,-0.0403346681066388,
-0.0118546873591697));
#34471=CARTESIAN_POINT('Ctrl Pts',(0.00751220918272555,-0.0403339338421727,
-0.0118688024639827));
#34472=CARTESIAN_POINT('Ctrl Pts',(0.007517439300735,-0.0403325184288825,
-0.0118958541084151));
#34473=CARTESIAN_POINT('Ctrl Pts',(0.00751976807005864,-0.0403318384098902,
-0.0119087829395005));
#34474=CARTESIAN_POINT('Ctrl Pts',(0.00752546818548569,-0.0403300329188543,
-0.0119429219400548));
#34475=CARTESIAN_POINT('Ctrl Pts',(0.00752856220884581,-0.04032889888979,
-0.011964174971697));
#34476=CARTESIAN_POINT('Ctrl Pts',(0.00753907045443044,-0.040324347603729,
-0.012048697164316));
#34477=CARTESIAN_POINT('Ctrl Pts',(0.00754300673222017,-0.0403208263147395,
-0.0121123289554273));
#34478=CARTESIAN_POINT('Ctrl Pts',(0.00754299363468279,-0.0403138357438406,
-0.0122360752528632));
#34479=CARTESIAN_POINT('Ctrl Pts',(0.00753948075027893,-0.040310381362184,
-0.0122960806343023));
#34480=CARTESIAN_POINT('Ctrl Pts',(0.00752464214422209,-0.0403030819248212,
-0.0124225025366504));
#34481=CARTESIAN_POINT('Ctrl Pts',(0.00751244756973687,-0.040299246965904,
-0.012488700055835));
#34482=CARTESIAN_POINT('Ctrl Pts',(0.007491777459145,-0.0402946442035614,
-0.0125704951364037));
#34483=CARTESIAN_POINT('Ctrl Pts',(0.00748730619594309,-0.0402937213372485,
-0.0125870253956281));
#34484=CARTESIAN_POINT('Ctrl Pts',(0.00747999081126814,-0.0402923203577272,
-0.0126123875631331));
#34485=CARTESIAN_POINT('Ctrl Pts',(0.00747734077131737,-0.0402918323652687,
-0.0126212735712009));
#34486=CARTESIAN_POINT('Ctrl Pts',(0.00747224957979907,-0.0402909308680515,
-0.0126377997031975));
#34487=CARTESIAN_POINT('Ctrl Pts',(0.00746982875414881,-0.040290516320024,
-0.012645445398858));
#34488=CARTESIAN_POINT('Ctrl Pts',(0.00746384371102012,-0.0402895241320731,
-0.0126638481598918));
#34489=CARTESIAN_POINT('Ctrl Pts',(0.0074602203541576,-0.0402889498051573,
-0.0126745856179936));
#34490=CARTESIAN_POINT('Ctrl Pts',(0.00744650860343296,-0.0402868665418217,
-0.0127137880749279));
#34491=CARTESIAN_POINT('Ctrl Pts',(0.00743570298600019,-0.040285393932746,
-0.0127419964834778));
#34492=CARTESIAN_POINT('Ctrl Pts',(0.00740405424159433,-0.0402814606177515,
-0.0128178699894255));
#34493=CARTESIAN_POINT('Ctrl Pts',(0.00738161775109788,-0.040279056021971,
-0.01286482836826));
#34494=CARTESIAN_POINT('Ctrl Pts',(0.00730257127607069,-0.0402714295646993,
-0.0130108097373296));
#34495=CARTESIAN_POINT('Ctrl Pts',(0.00723735442326272,-0.0402662609593681,
-0.0131047217027002));
#34496=CARTESIAN_POINT('Ctrl Pts',(0.00714619465120043,-0.0402594895565454,
-0.0132091457545853));
#34497=CARTESIAN_POINT('Ctrl Pts',(0.00712955750886972,-0.0402582704283589,
-0.0132273071629746));
#34498=CARTESIAN_POINT('Ctrl Pts',(0.00710195540869737,-0.0402562692446052,
-0.0132560266751178));
#34499=CARTESIAN_POINT('Ctrl Pts',(0.00709125614038842,-0.0402554984815776,
-0.0132668346278284));
#34500=CARTESIAN_POINT('Ctrl Pts',(0.00707023003018678,-0.0402539922359212,
-0.0132874555334687));
#34501=CARTESIAN_POINT('Ctrl Pts',(0.00705992358778738,-0.0402532576882166,
-0.0132972871200758));
#34502=CARTESIAN_POINT('Ctrl Pts',(0.00703520729260259,-0.0402515042566375,
-0.0133202195228351));
#34503=CARTESIAN_POINT('Ctrl Pts',(0.00702068285259519,-0.0402504801701176,
-0.0133331927741724));
#34504=CARTESIAN_POINT('Ctrl Pts',(0.00696757253860754,-0.0402467563739465,
-0.0133788534799981));
#34505=CARTESIAN_POINT('Ctrl Pts',(0.00692763372871506,-0.0402439932862024,
-0.0134099120365688));
#34506=CARTESIAN_POINT('Ctrl Pts',(0.0068114018217784,-0.0402360697866959,
-0.0134914654130546));
#34507=CARTESIAN_POINT('Ctrl Pts',(0.00673204235351503,-0.0402307818460033,
-0.0135372202990062));
#34508=CARTESIAN_POINT('Ctrl Pts',(0.00659482577633572,-0.0402221378613781,
-0.0136008485070819));
#34509=CARTESIAN_POINT('Ctrl Pts',(0.0065391212700711,-0.0402187567995619,
-0.013622842736316));
#34510=CARTESIAN_POINT('Ctrl Pts',(0.00646903628206338,-0.040214767076841,
-0.0136459037082862));
#34511=CARTESIAN_POINT('Ctrl Pts',(0.00645573742270655,-0.0402140215003565,
-0.0136500807806306));
#34512=CARTESIAN_POINT('Ctrl Pts',(0.00643423630405216,-0.0402128365602255,
-0.0136565153516891));
#34513=CARTESIAN_POINT('Ctrl Pts',(0.00642606905079611,-0.0402123911736499,
-0.0136588861552256));
#34514=CARTESIAN_POINT('Ctrl Pts',(0.00640978564714478,-0.0402115131379154,
-0.0136634673057992));
#34515=CARTESIAN_POINT('Ctrl Pts',(0.00640167022233017,-0.0402110804315408,
-0.0136656790430655));
#34516=CARTESIAN_POINT('Ctrl Pts',(0.0063804829877849,-0.0402099625236005,
-0.0136712675964416));
#34517=CARTESIAN_POINT('Ctrl Pts',(0.00636738396481212,-0.0402092829928113,
-0.0136745394805046));
#34518=CARTESIAN_POINT('Ctrl Pts',(0.00630120246256232,-0.0402059004767904,
-0.0136901504627736));
#34519=CARTESIAN_POINT('Ctrl Pts',(0.00624753154893221,-0.040203320313985,
-0.0136998440837757));
#34520=CARTESIAN_POINT('Ctrl Pts',(0.00607883964329059,-0.0401954181763324,
-0.0137211623565376));
#34521=CARTESIAN_POINT('Ctrl Pts',(0.00596296217540964,-0.0401902583719616,
-0.0137227290113307));
#34522=CARTESIAN_POINT('Ctrl Pts',(0.0058105679022793,-0.0401829425867689,
-0.0137076427269774));
#34523=CARTESIAN_POINT('Ctrl Pts',(0.00577329221115343,-0.0401811136345478,
-0.0137025709165474));
#34524=CARTESIAN_POINT('Ctrl Pts',(0.00571887632306444,-0.0401783665276171,
-0.0136931301472994));
#34525=CARTESIAN_POINT('Ctrl Pts',(0.00570156540977394,-0.0401774810805772,
-0.0136898203790236));
#34526=CARTESIAN_POINT('Ctrl Pts',(0.00567059380385307,-0.04017587450769,
-0.0136833469236624));
#34527=CARTESIAN_POINT('Ctrl Pts',(0.00565691222451923,-0.040175156898776,
-0.0136802921418639));
#34528=CARTESIAN_POINT('Ctrl Pts',(0.00562757210221092,-0.0401736002078394,
-0.0136733201300485));
#34529=CARTESIAN_POINT('Ctrl Pts',(0.00561192968306698,-0.0401727592769231,
-0.013669342787428));
#34530=CARTESIAN_POINT('Ctrl Pts',(0.00556803411134551,-0.0401703674623307,
-0.0136574454497776));
#34531=CARTESIAN_POINT('Ctrl Pts',(0.00553994140173687,-0.0401687989056851,
-0.0136489642117284));
#34532=CARTESIAN_POINT('Ctrl Pts',(0.00544037245825868,-0.0401631021784236,
-0.0136157782047824));
#34533=CARTESIAN_POINT('Ctrl Pts',(0.00537049787839429,-0.0401588405396027,
-0.0135866302939539));
#34534=CARTESIAN_POINT('Ctrl Pts',(0.00521523389267398,-0.0401488866767666,
-0.0135080240204686));
#34535=CARTESIAN_POINT('Ctrl Pts',(0.00513187306148297,-0.0401431681972347,
-0.0134552647863316));
#34536=CARTESIAN_POINT('Ctrl Pts',(0.00503938843387431,-0.0401367626469985,
-0.0133835044565315));
#34537=CARTESIAN_POINT('Ctrl Pts',(0.00502487997886895,-0.0401357563713039,
-0.0133718202311756));
#34538=CARTESIAN_POINT('Ctrl Pts',(0.00500332313841348,-0.0401342636271399,
-0.0133538065192534));
#34539=CARTESIAN_POINT('Ctrl Pts',(0.00499611603124252,-0.0401337649755924,
-0.0133476704954765));
#34540=CARTESIAN_POINT('Ctrl Pts',(0.00498354693693273,-0.0401328967934447,
-0.0133367682809583));
#34541=CARTESIAN_POINT('Ctrl Pts',(0.00497816125846767,-0.0401325253300547,
-0.0133320306267527));
#34542=CARTESIAN_POINT('Ctrl Pts',(0.00496500621493986,-0.0401316190870195,
-0.0133202947181631));
#34543=CARTESIAN_POINT('Ctrl Pts',(0.00495727467599045,-0.0401310873409846,
-0.0133132548144854));
#34544=CARTESIAN_POINT('Ctrl Pts',(0.00493187871816833,-0.0401293413109231,
-0.0132896540688937));
#34545=CARTESIAN_POINT('Ctrl Pts',(0.00491453188351238,-0.0401281496542151,
-0.0132727554418182));
#34546=CARTESIAN_POINT('Ctrl Pts',(0.00487176531018632,-0.0401251926184072,
-0.0132290853135259));
#34547=CARTESIAN_POINT('Ctrl Pts',(0.00484689467674212,-0.0401234547917817,
-0.0132017965503136));
#34548=CARTESIAN_POINT('Ctrl Pts',(0.00474878601273222,-0.0401164029261517,
-0.0130860691439521));
#34549=CARTESIAN_POINT('Ctrl Pts',(0.00468455339088075,-0.0401112747257682,
-0.0129904882228372));
#34550=CARTESIAN_POINT('Ctrl Pts',(0.00461386333023939,-0.0401039707727769,
-0.0128547747284036));
#34551=CARTESIAN_POINT('Ctrl Pts',(0.00459747652041293,-0.0401021137308062,
-0.0128202419913573));
#34552=CARTESIAN_POINT('Ctrl Pts',(0.004575390220447,-0.0400993324930915,
-0.0127688542346881));
#34553=CARTESIAN_POINT('Ctrl Pts',(0.00456867273681648,-0.0400984422383127,
-0.012752451397434));
#34554=CARTESIAN_POINT('Ctrl Pts',(0.00455714755953665,-0.0400968304100547,
-0.0127228657341133));
#34555=CARTESIAN_POINT('Ctrl Pts',(0.00455223425630502,-0.0400961124515623,
-0.0127097260402703));
#34556=CARTESIAN_POINT('Ctrl Pts',(0.0045420764996996,-0.040094558898561,
-0.0126813891200141));
#34557=CARTESIAN_POINT('Ctrl Pts',(0.00453688905817036,-0.0400937215260027,
-0.0126661733427898));
#34558=CARTESIAN_POINT('Ctrl Pts',(0.00452301252276451,-0.0400913516626143,
-0.0126232881858243));
#34559=CARTESIAN_POINT('Ctrl Pts',(0.00451486468955921,-0.0400898020214516,
-0.0125954518525099));
#34560=CARTESIAN_POINT('Ctrl Pts',(0.00448662158125346,-0.040083764457735,
-0.0124877960722624));
#34561=CARTESIAN_POINT('Ctrl Pts',(0.00447214163801477,-0.0400791119384198,
-0.0124066534941163));
#34562=CARTESIAN_POINT('Ctrl Pts',(0.00445940319010193,-0.0400715496481565,
-0.0122752641998871));
#34563=CARTESIAN_POINT('Ctrl Pts',(0.00445699999999992,-0.04006868578093,
-0.0122255734026042));
#34564=CARTESIAN_POINT('Ctrl Pts',(0.004457,-0.0400658559061629,-0.0121758532865556));
#34565=CARTESIAN_POINT('Ctrl Pts',(0.004457,-0.0405679692773165,-0.012175853286558));
#34566=CARTESIAN_POINT('Ctrl Pts',(0.004457,-0.0405679633251033,-0.0121757394235622));
#34567=CARTESIAN_POINT('Ctrl Pts',(0.00445700001260348,-0.040567957372501,
-0.0121756255605583));
#34568=CARTESIAN_POINT('Ctrl Pts',(0.00445700003781045,-0.0405679514195094,
-0.0121755116975483));
#34569=CARTESIAN_POINT('Ctrl Pts',(0.00517003826372136,-0.0368388088258703,
-0.0112226527283813));
#34570=CARTESIAN_POINT('Ctrl Pts',(0.00496318803061621,-0.0368566041514186,
-0.0114031443924197));
#34571=CARTESIAN_POINT('Ctrl Pts',(0.00481517121886622,-0.0368716613977715,
-0.0116537046307317));
#34572=CARTESIAN_POINT('Ctrl Pts',(0.00476045244943773,-0.0368890231487594,
-0.0119228284334495));
#34573=CARTESIAN_POINT('Ctrl Pts',(0.00475804259485334,-0.0368897877729577,
-0.011934680842349));
#34574=CARTESIAN_POINT('Ctrl Pts',(0.00475581169755592,-0.0368905568669409,
-0.0119465719172147));
#34575=CARTESIAN_POINT('Ctrl Pts',(0.00475375746819469,-0.0368913308614504,
-0.0119584969221675));
#34576=CARTESIAN_POINT('Ctrl Pts',(0.00472994900992145,-0.0369003014351997,
-0.0120967073811281));
#34577=CARTESIAN_POINT('Ctrl Pts',(0.00472969925662481,-0.0369100660923477,
-0.0122383423209631));
#34578=CARTESIAN_POINT('Ctrl Pts',(0.00475183331331961,-0.0369192107959462,
-0.0123755348980974));
#34579=CARTESIAN_POINT('Ctrl Pts',(0.00479405294068054,-0.0369366538694675,
-0.0126372230090101));
#34580=CARTESIAN_POINT('Ctrl Pts',(0.00492069786421945,-0.0369513027772182,
-0.0128890197323158));
#34581=CARTESIAN_POINT('Ctrl Pts',(0.00511161730525771,-0.036968058701728,
-0.0130769904122617));
#34582=CARTESIAN_POINT('Ctrl Pts',(0.00512542591996926,-0.0369692706061021,
-0.0130905857521723));
#34583=CARTESIAN_POINT('Ctrl Pts',(0.00513957437411001,-0.0369704935326665,
-0.013103852713356));
#34584=CARTESIAN_POINT('Ctrl Pts',(0.0051540427324716,-0.0369717293358099,
-0.0131167880484792));
#34585=CARTESIAN_POINT('Ctrl Pts',(0.00525891627092471,-0.0369806870243903,
-0.0132105495058292));
#34586=CARTESIAN_POINT('Ctrl Pts',(0.00537951599478848,-0.0369904541203737,
-0.0132863860868721));
#34587=CARTESIAN_POINT('Ctrl Pts',(0.00550872901378148,-0.0369996339059789,
-0.0133406619611183));
#34588=CARTESIAN_POINT('Origin',(0.006,-0.0418165664398416,-0.0121758532865581));
#34589=CARTESIAN_POINT('Origin',(0.0078,-0.0299787743898723,-0.00817585328655812));
#34590=CARTESIAN_POINT('Origin',(-0.0125,-0.0298787743898723,-0.0121758532865581));
#34591=CARTESIAN_POINT('',(-0.0137645000000023,-0.03021427438987,-0.0121758532865581));
#34592=CARTESIAN_POINT('Origin',(-0.01249999999999,-0.0302142743898623,
-0.0121758532865681));
#34593=CARTESIAN_POINT('',(-0.0141,-0.0298787743898723,-0.0121758532865581));
#34594=CARTESIAN_POINT('Origin',(-0.01249999999999,-0.0302142743898623,
-0.0121758532865681));
#34595=CARTESIAN_POINT('Origin',(-0.0148,-0.0299787743898723,-0.0161758532865581));
#34596=CARTESIAN_POINT('Origin',(-0.0125,-0.0302142743898723,-0.0121758532865581));
#34597=CARTESIAN_POINT('Origin',(0.006,-0.0418165664398416,-0.0121758532865581));
#34598=CARTESIAN_POINT('',(0.00753652184170541,-0.0364251782306474,-0.0123170964455508));
#34599=CARTESIAN_POINT('Origin',(0.00600000000001,-0.036425178177226,-0.0121758532865681));
#34600=CARTESIAN_POINT('Ctrl Pts',(0.00753652184170541,-0.0364251782306474,
-0.0123170964455508));
#34601=CARTESIAN_POINT('Ctrl Pts',(0.00756822434111586,-0.0364430425111789,
-0.0119722189794262));
#34602=CARTESIAN_POINT('Ctrl Pts',(0.00747951616489019,-0.0364609067917104,
-0.0116174390738647));
#34603=CARTESIAN_POINT('Ctrl Pts',(0.00728922782690805,-0.0364787710722419,
-0.0113280675764132));
#34604=CARTESIAN_POINT('Ctrl Pts',(0.0072673963600219,-0.0364808206116566,
-0.0112948684622089));
#34605=CARTESIAN_POINT('Ctrl Pts',(0.00724428189505873,-0.0364828701510714,
-0.0112625130653046));
#34606=CARTESIAN_POINT('Ctrl Pts',(0.00721995334505698,-0.0364849196904862,
-0.0112310978494823));
#34607=CARTESIAN_POINT('Origin',(0.006,-0.036425178177236,-0.0121758532865581));
#34608=CARTESIAN_POINT('Origin',(0.0064207661241384,-0.0364251781806992,
-0.0121386924149705));
#34609=CARTESIAN_POINT('Ctrl Pts',(0.0072199533450484,-0.0364849196904962,
-0.0112310978494712));
#34610=CARTESIAN_POINT('Ctrl Pts',(0.0074098002074744,-0.0364689287443744,
-0.0114762452238835));
#34611=CARTESIAN_POINT('Ctrl Pts',(0.0076367749937228,-0.0364369468521306,
-0.0120839293008583));
#34612=CARTESIAN_POINT('Ctrl Pts',(0.0074792699890148,-0.0364049649598869,
-0.0127132063976075));
#34613=CARTESIAN_POINT('Ctrl Pts',(0.0073180661489925,-0.036388974013765,
-0.0129780693589976));
#34614=CARTESIAN_POINT('Ctrl Pts',(0.00714655018737591,-0.0365385211752087,
-0.0112879426727523));
#34615=CARTESIAN_POINT('Ctrl Pts',(0.00732497418741711,-0.0365225302290869,
-0.0115183398180267));
#34616=CARTESIAN_POINT('Ctrl Pts',(0.00753829216778011,-0.0364905483368431,
-0.0120894602589426));
#34617=CARTESIAN_POINT('Ctrl Pts',(0.00739026405392343,-0.0364585664445993,
-0.012680874493034));
#34618=CARTESIAN_POINT('Ctrl Pts',(0.00723875965932221,-0.0364425754984775,
-0.0129298009616103));
#34619=CARTESIAN_POINT('Ctrl Pts',(0.0070731470297034,-0.0365921226599213,
-0.0113447874960334));
#34620=CARTESIAN_POINT('Ctrl Pts',(0.00724014816735991,-0.0365761317137994,
-0.0115604344121699));
#34621=CARTESIAN_POINT('Ctrl Pts',(0.00743980934183733,-0.0365441498215557,
-0.0120949912170268));
#34622=CARTESIAN_POINT('Ctrl Pts',(0.00730125811883206,-0.036512167929312,
-0.0126485425884606));
#34623=CARTESIAN_POINT('Ctrl Pts',(0.00715945316965194,-0.0364961769831901,
-0.0128815325642231));
#34624=CARTESIAN_POINT('Ctrl Pts',(0.0069997438720308,-0.0366457241446337,
-0.0114016323193146));
#34625=CARTESIAN_POINT('Ctrl Pts',(0.00715532214730263,-0.0366297331985119,
-0.0116025290063132));
#34626=CARTESIAN_POINT('Ctrl Pts',(0.00734132651589453,-0.0365977513062682,
-0.0121005221751111));
#34627=CARTESIAN_POINT('Ctrl Pts',(0.0072122521837407,-0.0365657694140244,
-0.0126162106838871));
#34628=CARTESIAN_POINT('Ctrl Pts',(0.00708014667998167,-0.0365497784679025,
-0.0128332641668358));
#34629=CARTESIAN_POINT('Ctrl Pts',(0.00708453011998519,-0.0366362514743427,
-0.0115256574169581));
#34630=CARTESIAN_POINT('Ctrl Pts',(0.00723825165049006,-0.0366174374253146,
-0.0117820657359241));
#34631=CARTESIAN_POINT('Ctrl Pts',(0.00729678566547772,-0.0365986233762864,
-0.0120941053643385));
#34632=CARTESIAN_POINT('Ctrl Pts',(0.00724644164534432,-0.0365798093272583,
-0.0123887933597039));
#34633=CARTESIAN_POINT('Ctrl Pts',(0.00722898096775414,-0.0365732841025469,
-0.0124909991840131));
#34634=CARTESIAN_POINT('Ctrl Pts',(0.00719888732060191,-0.0365667588778354,
-0.0125910404109786));
#34635=CARTESIAN_POINT('Ctrl Pts',(0.00715706304473573,-0.036560233653124,
-0.0126859173614613));
#34636=CARTESIAN_POINT('Origin',(0.006,-0.0412787743898723,-0.0121758532865581));
#34637=CARTESIAN_POINT('Ctrl Pts',(0.0071049221523962,-0.036616763538703,
-0.0127891486670682));
#34638=CARTESIAN_POINT('Ctrl Pts',(0.00722758846935883,-0.0366330987428971,
-0.0125677025948817));
#34639=CARTESIAN_POINT('Ctrl Pts',(0.00728449242226235,-0.0366477660520011,
-0.01230803163059));
#34640=CARTESIAN_POINT('Ctrl Pts',(0.00726021773649979,-0.0366635671619898,
-0.0120563276956654));
#34641=CARTESIAN_POINT('Ctrl Pts',(0.00725576839945219,-0.0366664633668987,
-0.0120101925714606));
#34642=CARTESIAN_POINT('Ctrl Pts',(0.00724860265255448,-0.0366693976626142,
-0.0119643005706726));
#34643=CARTESIAN_POINT('Ctrl Pts',(0.00723890064348258,-0.0366723873013995,
-0.0119188749448376));
#34644=CARTESIAN_POINT('Ctrl Pts',(0.00719971714612425,-0.0366844615535031,
-0.011735414501056));
#34645=CARTESIAN_POINT('Ctrl Pts',(0.00711972216632024,-0.0366973265713535,
-0.0115610957458025));
#34646=CARTESIAN_POINT('Ctrl Pts',(0.00700648721588952,-0.0367089394431721,
-0.0114117479980388));
#34647=CARTESIAN_POINT('Ctrl Pts',(0.00658722785536586,-0.036742294363837,
-0.0110560653534979));
#34648=CARTESIAN_POINT('Ctrl Pts',(0.00695797246101722,-0.0367159475964203,
-0.0112504847865641));
#34649=CARTESIAN_POINT('Ctrl Pts',(0.00748293891467684,-0.0366632540613929,
-0.0120352036662368));
#34650=CARTESIAN_POINT('Ctrl Pts',(0.00711485957225081,-0.0366105605263656,
-0.012904623644283));
#34651=CARTESIAN_POINT('Ctrl Pts',(0.00678727634316453,-0.0365842137587548,
-0.0131652761125726));
#34652=CARTESIAN_POINT('Ctrl Pts',(0.00663053159797881,-0.0367961275404045,
-0.010973489215477));
#34653=CARTESIAN_POINT('Ctrl Pts',(0.00702861589610487,-0.0367697807729879,
-0.0111822456542074));
#34654=CARTESIAN_POINT('Ctrl Pts',(0.00759229477115595,-0.0367170872379605,
-0.0120248317894578));
#34655=CARTESIAN_POINT('Ctrl Pts',(0.00719707227984838,-0.0366643937029331,
-0.0129583651071692));
#34656=CARTESIAN_POINT('Ctrl Pts',(0.00684533219289669,-0.0366380469353223,
-0.0132382387811545));
#34657=CARTESIAN_POINT('Ctrl Pts',(0.00667383534059177,-0.0368499607169721,
-0.0108909130774562));
#34658=CARTESIAN_POINT('Ctrl Pts',(0.00709925933119253,-0.0368236139495555,
-0.0111140065218506));
#34659=CARTESIAN_POINT('Ctrl Pts',(0.00770165062763507,-0.0367709204145281,
-0.0120144599126789));
#34660=CARTESIAN_POINT('Ctrl Pts',(0.00727928498744596,-0.0367182268795007,
-0.0130121065700554));
#34661=CARTESIAN_POINT('Ctrl Pts',(0.00690338804262885,-0.0366918801118899,
-0.0133112014497364));
#34662=CARTESIAN_POINT('Ctrl Pts',(0.00671713908320482,-0.0369037938935395,
-0.0108083369394354));
#34663=CARTESIAN_POINT('Ctrl Pts',(0.00716990276628018,-0.0368774471261231,
-0.0110457673894939));
#34664=CARTESIAN_POINT('Ctrl Pts',(0.00781100648411419,-0.0368247535910955,
-0.0120040880358999));
#34665=CARTESIAN_POINT('Ctrl Pts',(0.00736149769504353,-0.0367720600560681,
-0.0130658480329415));
#34666=CARTESIAN_POINT('Ctrl Pts',(0.00696144389236101,-0.0367457132884574,
-0.0133841641183183));
#34667=CARTESIAN_POINT('Ctrl Pts',(0.00671669833492856,-0.0369031264224378,
-0.0108094007638883));
#34668=CARTESIAN_POINT('Ctrl Pts',(0.00701188501977547,-0.0368859357702769,
-0.0109642248810918));
#34669=CARTESIAN_POINT('Ctrl Pts',(0.0072554276123368,-0.036868745118116,
-0.0112188246564027));
#34670=CARTESIAN_POINT('Ctrl Pts',(0.00747237848207918,-0.0368424001339865,
-0.0116814132518847));
#34671=CARTESIAN_POINT('Ctrl Pts',(0.00751947603869318,-0.0368332458020179,
-0.0118548192245139));
#34672=CARTESIAN_POINT('Ctrl Pts',(0.00756733595801313,-0.0368069008178862,
-0.0123594301513162));
#34673=CARTESIAN_POINT('Ctrl Pts',(0.0074885971694383,-0.036789710165723,
-0.0127017865636874));
#34674=CARTESIAN_POINT('Ctrl Pts',(0.00721964017367036,-0.0367633651813997,
-0.0131376204535356));
#34675=CARTESIAN_POINT('Ctrl Pts',(0.00709970046774227,-0.0367542108492395,
-0.0132726735662828));
#34676=CARTESIAN_POINT('Ctrl Pts',(0.00696081100483646,-0.0367450565170793,
-0.0133832021230528));
#34677=CARTESIAN_POINT('Origin',(0.006,-0.0418165664398416,-0.0121758532865581));
#34678=CARTESIAN_POINT('Origin',(0.006,-0.0412787743898723,-0.0121758532865581));
#34679=CARTESIAN_POINT('Ctrl Pts',(0.0053235011610246,-0.0369233529358344,
-0.0132441741984872));
#34680=CARTESIAN_POINT('Ctrl Pts',(0.00523505662430941,-0.0369167648474377,
-0.0131881679687734));
#34681=CARTESIAN_POINT('Ctrl Pts',(0.00515392214402666,-0.0369097144759522,
-0.0131214057275732));
#34682=CARTESIAN_POINT('Ctrl Pts',(0.00500976886549827,-0.0368958757947603,
-0.0129692115297485));
#34683=CARTESIAN_POINT('Ctrl Pts',(0.00494735345119867,-0.0368891524433538,
-0.0128843145970702));
#34684=CARTESIAN_POINT('Ctrl Pts',(0.00481584137034549,-0.0368726379308069,
-0.0126489587493082));
#34685=CARTESIAN_POINT('Ctrl Pts',(0.00476439120123418,-0.0368635400229235,
-0.0124909884384143));
#34686=CARTESIAN_POINT('Ctrl Pts',(0.00472487521828434,-0.0368427862176367,
-0.0121641285889202));
#34687=CARTESIAN_POINT('Ctrl Pts',(0.00473723272218724,-0.0368312891618365,
-0.0119983443282033));
#34688=CARTESIAN_POINT('Ctrl Pts',(0.00480893333673192,-0.0368138833665868,
-0.0117384487674225));
#34689=CARTESIAN_POINT('Ctrl Pts',(0.00484930331121405,-0.0368074684757722,
-0.011641189466955));
#34690=CARTESIAN_POINT('Ctrl Pts',(0.00495301550513732,-0.0367949520902989,
-0.0114591025077254));
#34691=CARTESIAN_POINT('Ctrl Pts',(0.00501587895403898,-0.0367888825209941,
-0.0113749731264201));
#34692=CARTESIAN_POINT('Ctrl Pts',(0.00508837275135261,-0.0367823435972233,
-0.0112995565277352));
#34693=CARTESIAN_POINT('Ctrl Pts',(0.0051742753449155,-0.0367620604347684,
-0.0134803778190167));
#34694=CARTESIAN_POINT('Ctrl Pts',(0.00478645345963078,-0.0367384031130101,
-0.0132349052736592));
#34695=CARTESIAN_POINT('Ctrl Pts',(0.00424919073978731,-0.0366910919663293,
-0.0123774938115404));
#34696=CARTESIAN_POINT('Ctrl Pts',(0.00457748608479308,-0.0366437808196484,
-0.0114204297049166));
#34697=CARTESIAN_POINT('Ctrl Pts',(0.00489928336256372,-0.0366201269947257,
-0.0110932507042787));
#34698=CARTESIAN_POINT('Ctrl Pts',(0.0052243777953317,-0.0368161458631363,
-0.0134012232542332));
#34699=CARTESIAN_POINT('Ctrl Pts',(0.00486008775768916,-0.0367924885413782,
-0.0131706452332872));
#34700=CARTESIAN_POINT('Ctrl Pts',(0.00435542449895617,-0.0367451773946972,
-0.0123652588802681));
#34701=CARTESIAN_POINT('Ctrl Pts',(0.00466379988499779,-0.0366978662480164,
-0.0114662665008865));
#34702=CARTESIAN_POINT('Ctrl Pts',(0.00496607148667975,-0.0366742124230938,
-0.0111589397228459));
#34703=CARTESIAN_POINT('Ctrl Pts',(0.00527448024574789,-0.0368702312915042,
-0.0133220686894497));
#34704=CARTESIAN_POINT('Ctrl Pts',(0.00493372205574744,-0.036846573969746,
-0.0131063851929151));
#34705=CARTESIAN_POINT('Ctrl Pts',(0.00446165825812503,-0.0367992628230653,
-0.0123530239489957));
#34706=CARTESIAN_POINT('Ctrl Pts',(0.00475011368520242,-0.0367519516763844,
-0.0115121032968564));
#34707=CARTESIAN_POINT('Ctrl Pts',(0.00503285961079578,-0.0367282978514617,
-0.0112246287414129));
#34708=CARTESIAN_POINT('Ctrl Pts',(0.00532458269616408,-0.0369243167198722,
-0.0132429141246661));
#34709=CARTESIAN_POINT('Ctrl Pts',(0.00500735635380582,-0.036900659398114,
-0.0130421251525431));
#34710=CARTESIAN_POINT('Ctrl Pts',(0.0045678920172939,-0.0368533482514331,
-0.0123407890177234));
#34711=CARTESIAN_POINT('Ctrl Pts',(0.00483642748540704,-0.0368060371047523,
-0.0115579400928262));
#34712=CARTESIAN_POINT('Ctrl Pts',(0.00509964773491181,-0.0367823832798296,
-0.0112903177599799));
#34713=CARTESIAN_POINT('Ctrl Pts',(0.00489985734136315,-0.0366206471528947,
-0.0110939405679678));
#34714=CARTESIAN_POINT('Ctrl Pts',(0.00466420781315652,-0.0366379795411557,
-0.0113335607277211));
#34715=CARTESIAN_POINT('Ctrl Pts',(0.00450992989288636,-0.0366553119294167,
-0.0116531134538887));
#34716=CARTESIAN_POINT('Ctrl Pts',(0.00446868682950251,-0.0366726443176777,
-0.0119863038896692));
#34717=CARTESIAN_POINT('Ctrl Pts',(0.00445672246310587,-0.0366776723400085,
-0.0120829604453774));
#34718=CARTESIAN_POINT('Ctrl Pts',(0.004453955327891,-0.0366827003623392,
-0.0121806314281746));
#34719=CARTESIAN_POINT('Ctrl Pts',(0.00446035287725328,-0.03668772838467,
-0.012277518115372));
#34720=CARTESIAN_POINT('Ctrl Pts',(0.00448240549051054,-0.0367050601824617,
-0.0126114904728402));
#34721=CARTESIAN_POINT('Ctrl Pts',(0.00461749012905982,-0.0367223919802533,
-0.0129392208664159));
#34722=CARTESIAN_POINT('Ctrl Pts',(0.00483915438748629,-0.036739723778045,
-0.0131923602781266));
#34723=CARTESIAN_POINT('Ctrl Pts',(0.00490339558020791,-0.0367447467590616,
-0.0132657233807241));
#34724=CARTESIAN_POINT('Ctrl Pts',(0.00497459353102844,-0.0367497697400783,
-0.0133329516444489));
#34725=CARTESIAN_POINT('Ctrl Pts',(0.00505141064578676,-0.0367547927210949,
-0.013392827911221));
#34726=CARTESIAN_POINT('Origin',(0.006,-0.0418165664398416,-0.0121758532865581));
#34727=CARTESIAN_POINT('Ctrl Pts',(0.00490822568141441,-0.036629014744178,
-0.0132662100342682));
#34728=CARTESIAN_POINT('Ctrl Pts',(0.00466938135519506,-0.0366115831763784,
-0.0130270551869636));
#34729=CARTESIAN_POINT('Ctrl Pts',(0.00451241393214875,-0.0365941516085787,
-0.0127067464029452));
#34730=CARTESIAN_POINT('Ctrl Pts',(0.00446454380236732,-0.0365747000596988,
-0.012333183817743));
#34731=CARTESIAN_POINT('Ctrl Pts',(0.00446105042715403,-0.0365726800786186,
-0.0122942175049728));
#34732=CARTESIAN_POINT('Ctrl Pts',(0.00444170231516779,-0.0365532285297388,
-0.0119184373241344));
#34733=CARTESIAN_POINT('Ctrl Pts',(0.00453897781770981,-0.0365357969619391,
-0.0115753543699202));
#34734=CARTESIAN_POINT('Ctrl Pts',(0.00475379842566362,-0.0365163454130592,
-0.0112651579623936));
#34735=CARTESIAN_POINT('Ctrl Pts',(0.00477733077671506,-0.0365143254319789,
-0.0112338007169063));
#34736=CARTESIAN_POINT('Ctrl Pts',(0.00480201558775486,-0.0365123054508986,
-0.0112033912831782));
#34737=CARTESIAN_POINT('Ctrl Pts',(0.00509572370535752,-0.0364760372027012,
-0.013078987754096));
#34738=CARTESIAN_POINT('Ctrl Pts',(0.004874960106594,-0.0364565851795555,
-0.0128579454042039));
#34739=CARTESIAN_POINT('Ctrl Pts',(0.0046039989248781,-0.0364176811332647,
-0.012247730374574));
#34740=CARTESIAN_POINT('Ctrl Pts',(0.00481085609633788,-0.0363787770869738,
-0.0116129135072826));
#34741=CARTESIAN_POINT('Ctrl Pts',(0.00500775049564412,-0.0363593250638284,
-0.0113703668468132));
#34742=CARTESIAN_POINT('Ctrl Pts',(0.00503316372018776,-0.036527084977588,
-0.0131414687449504));
#34743=CARTESIAN_POINT('Ctrl Pts',(0.00479712717050601,-0.0365076329544425,
-0.0129051341594739));
#34744=CARTESIAN_POINT('Ctrl Pts',(0.0045074202496723,-0.0364687289081516,
-0.0122527030025053));
#34745=CARTESIAN_POINT('Ctrl Pts',(0.00472858829232875,-0.0364298248618607,
-0.0115739679942225));
#34746=CARTESIAN_POINT('Ctrl Pts',(0.00493910431455436,-0.0364103728387155,
-0.0113146413788082));
#34747=CARTESIAN_POINT('Ctrl Pts',(0.004970603735018,-0.0365781327524749,
-0.013203949735805));
#34748=CARTESIAN_POINT('Ctrl Pts',(0.00471929423441792,-0.0365586807293294,
-0.0129523229147439));
#34749=CARTESIAN_POINT('Ctrl Pts',(0.00441084157446649,-0.0365197766830385,
-0.0122576756304366));
#34750=CARTESIAN_POINT('Ctrl Pts',(0.00464632048831952,-0.0364808726367475,
-0.0115350224811624));
#34751=CARTESIAN_POINT('Ctrl Pts',(0.00487045813346461,-0.0364614206136023,
-0.0112589159108031));
#34752=CARTESIAN_POINT('Ctrl Pts',(0.00490804374984815,-0.0366291805273617,
-0.0132664307266594));
#34753=CARTESIAN_POINT('Ctrl Pts',(0.00464146129832983,-0.0366097285042163,
-0.0129995116700138));
#34754=CARTESIAN_POINT('Ctrl Pts',(0.0043142628992607,-0.0365708244579254,
-0.0122626482583679));
#34755=CARTESIAN_POINT('Ctrl Pts',(0.00456405268431038,-0.0365319204116345,
-0.0114960769681023));
#34756=CARTESIAN_POINT('Ctrl Pts',(0.00480181195237485,-0.0365124683884891,
-0.0112031904427979));
#34757=CARTESIAN_POINT('Ctrl Pts',(0.00473550000001001,-0.036425178177236,
-0.0117172854002574));
#34758=CARTESIAN_POINT('Ctrl Pts',(0.00470881837868537,-0.036425178177236,
-0.0118237756649726));
#34759=CARTESIAN_POINT('Ctrl Pts',(0.0046949074287484,-0.0364251781770394,
-0.0119335309693111));
#34760=CARTESIAN_POINT('Ctrl Pts',(0.00469488166357817,-0.0364251781770394,
-0.0121504784412239));
#34761=CARTESIAN_POINT('Ctrl Pts',(0.00470813137606538,-0.036425178177236,
-0.012256680250331));
#34762=CARTESIAN_POINT('Ctrl Pts',(0.00473547236319308,-0.036425178177236,
-0.0123610727438316));
#34763=CARTESIAN_POINT('Origin',(0.006,-0.036425178177236,-0.0121758532865581));
#34764=CARTESIAN_POINT('Origin',(1.7347234759768E-18,-0.0304787743898723,
-0.0121758532865581));
#34765=CARTESIAN_POINT('',(0.,0.,0.));
#34766=CARTESIAN_POINT('Origin',(0.00578869086912964,-0.0359819282833906,
-0.0013758532865581));
#34767=CARTESIAN_POINT('',(0.00568303630369446,-0.0362085052301498,-0.0043758532865581));
#34768=CARTESIAN_POINT('Origin',(0.00578869086912542,-0.0359819282833998,
-0.0043758532865481));
#34769=CARTESIAN_POINT('',(0.00568303630369446,-0.0362085052301498,-0.0013758532865381));
#34770=CARTESIAN_POINT('',(0.00568303630369446,-0.0362085052301498,-0.0013758532865581));
#34771=CARTESIAN_POINT('',(0.00556211392236143,-0.0358762737179513,-0.0013758532865581));
#34772=CARTESIAN_POINT('Origin',(0.00578869086912542,-0.0359819282833998,
-0.0013758532865481));
#34773=CARTESIAN_POINT('Origin',(0.00578869086912542,-0.0359819282833998,
-0.0013758532865481));
#34774=CARTESIAN_POINT('Origin',(0.0030697675080197,-0.0347140734981686,
-0.0013758532865581));
#34775=CARTESIAN_POINT('',(0.00306976750801062,-0.0347140734981644,0.0013741467134419));
#34776=CARTESIAN_POINT('Origin',(0.0030697675080197,-0.0347140734981686,
-0.0013758532865581));
#34777=CARTESIAN_POINT('',(0.0029641129425755,-0.0349406504449234,0.0016241467134419));
#34778=CARTESIAN_POINT('Origin',(0.00306976750800641,-0.0347140734981734,
0.0016241467134519));
#34779=CARTESIAN_POINT('Origin',(0.00306976750800641,-0.0347140734981734,
0.0016241467134519));
#34780=CARTESIAN_POINT('Origin',(-0.01052484929753,-0.0283747995720579,
0.00162414671344191));
#34781=CARTESIAN_POINT('',(-0.0106305038629742,-0.0286013765188128,0.00162414671344191));
#34782=CARTESIAN_POINT('',(-0.0106305038629652,-0.0286013765188171,0.00162414671344191));
#34783=CARTESIAN_POINT('Origin',(-0.0105248492975433,-0.0283747995720628,
0.00162414671345191));
#34784=CARTESIAN_POINT('Origin',(0.00578869086912964,-0.0359819282833906,
-0.0043758532865581));
#34785=CARTESIAN_POINT('Origin',(-0.01052484929753,-0.0283747995720579,
0.00162414671344191));
#34786=CARTESIAN_POINT('',(0.,0.,0.));
#34787=CARTESIAN_POINT('Origin',(0.,-0.0288900992552775,-0.0121758532865581));
#34788=CARTESIAN_POINT('',(0.00249999999996746,-0.0263900992552675,-0.0121758405315141));
#34789=CARTESIAN_POINT('',(0.00249999969210765,-0.0253900438073696,-0.0121749724286797));
#34790=CARTESIAN_POINT('Ctrl Pts',(0.00249999999999986,-0.0263900983848402,
-0.0121758541222231));
#34791=CARTESIAN_POINT('Ctrl Pts',(0.0024999998376673,-0.0263591782252352,
-0.0126614929956707));
#34792=CARTESIAN_POINT('Ctrl Pts',(0.00235420814557946,-0.0263282580656303,
-0.0131471076179502));
#34793=CARTESIAN_POINT('Ctrl Pts',(0.00208694255055651,-0.0262973379060254,
-0.0135523236969472));
#34794=CARTESIAN_POINT('Ctrl Pts',(0.00199405292942151,-0.0262865914352314,
-0.013693158764224));
#34795=CARTESIAN_POINT('Ctrl Pts',(0.00188693836179305,-0.0262758449644375,
-0.0138244280014296));
#34796=CARTESIAN_POINT('Ctrl Pts',(0.00176792152173108,-0.0262650984936436,
-0.0139434656572435));
#34797=CARTESIAN_POINT('Ctrl Pts',(0.00143179056821086,-0.0262347479863283,
-0.0142796553992388));
#34798=CARTESIAN_POINT('Ctrl Pts',(0.000995395947558976,-0.0262043974790131,
-0.0145182192446305));
#34799=CARTESIAN_POINT('Ctrl Pts',(0.000529245665941188,-0.0261740469716978,
-0.0146191909679035));
#34800=CARTESIAN_POINT('Ctrl Pts',(0.00035544250978807,-0.0261627308486142,
-0.0146568380634414));
#34801=CARTESIAN_POINT('Ctrl Pts',(0.000177767476799881,-0.0261514147255306,
-0.0146758221771375));
#34802=CARTESIAN_POINT('Ctrl Pts',(4.38041264954561E-7,-0.026140098602447,
-0.0146758532481821));
#34803=CARTESIAN_POINT('Ctrl Pts',(-0.000476928978646773,-0.0261096358429109,
-0.0146759368907647));
#34804=CARTESIAN_POINT('Ctrl Pts',(-0.000955851385580713,-0.0260791730833748,
-0.0145349752078753));
#34805=CARTESIAN_POINT('Ctrl Pts',(-0.00135775933618906,-0.0260487103238387,
-0.0142750173070652));
#34806=CARTESIAN_POINT('Ctrl Pts',(-0.0015055766989595,-0.026037506452976,
-0.0141794076251195));
#34807=CARTESIAN_POINT('Ctrl Pts',(-0.00164311820444229,-0.0260263025821132,
-0.0140682035642993));
#34808=CARTESIAN_POINT('Ctrl Pts',(-0.00176730198346023,-0.0260150987112504,
-0.0139440850867635));
#34809=CARTESIAN_POINT('Ctrl Pts',(-0.00210488795169868,-0.0259846416771423,
-0.0136066766365892));
#34810=CARTESIAN_POINT('Ctrl Pts',(-0.0023438742147858,-0.0259541846430342,
-0.0131684597223472));
#34811=CARTESIAN_POINT('Ctrl Pts',(-0.00244431536234987,-0.025923727608926,
-0.0127005650258783));
#34812=CARTESIAN_POINT('Ctrl Pts',(-0.00248128234709218,-0.0259125180126353,
-0.0125283581512571));
#34813=CARTESIAN_POINT('Ctrl Pts',(-0.00249993823183487,-0.0259013084163446,
-0.0123523861710988));
#34814=CARTESIAN_POINT('Ctrl Pts',(-0.0024999998462029,-0.0258900988200539,
-0.0121767302047395));
#34815=CARTESIAN_POINT('Ctrl Pts',(-0.00250016725552431,-0.0258596417859458,
-0.0116994641534089));
#34816=CARTESIAN_POINT('Ctrl Pts',(-0.00235934708740709,-0.0258291847518377,
-0.0112206008805832));
#34817=CARTESIAN_POINT('Ctrl Pts',(-0.00209955019121586,-0.0257987277177296,
-0.0108186911759149));
#34818=CARTESIAN_POINT('Ctrl Pts',(-0.00200393292547784,-0.0257875181214388,
-0.0106707698281338));
#34819=CARTESIAN_POINT('Ctrl Pts',(-0.00189270211542129,-0.0257763085251481,
-0.0105331307828027));
#34820=CARTESIAN_POINT('Ctrl Pts',(-0.00176854202418612,-0.0257650989288573,
-0.0104088617447878));
#34821=CARTESIAN_POINT('Ctrl Pts',(-0.00143112942651921,-0.0257346361693212,
-0.0100711530776225));
#34822=CARTESIAN_POINT('Ctrl Pts',(-0.000992860182890661,-0.0257041734097852,
-0.00983206793845762));
#34823=CARTESIAN_POINT('Ctrl Pts',(-0.000524883444357732,-0.0256737106502491,
-0.00973157478977441));
#34824=CARTESIAN_POINT('Ctrl Pts',(-0.000352766701647285,-0.0256625067793863,
-0.00969461450523058));
#34825=CARTESIAN_POINT('Ctrl Pts',(-0.000176886159280237,-0.0256513029085235,
-0.00967594603868218));
#34826=CARTESIAN_POINT('Ctrl Pts',(-1.31579507085305E-6,-0.0256400990376607,
-0.00967585363282146));
#34827=CARTESIAN_POINT('Ctrl Pts',(0.000474292116562906,-0.0256097485303454,
-0.00967560331176847));
#34828=CARTESIAN_POINT('Ctrl Pts',(0.000951652707267703,-0.0255793980230303,
-0.00981539592066256));
#34829=CARTESIAN_POINT('Ctrl Pts',(0.00135268560133641,-0.0255490475157151,
-0.0100734162092744));
#34830=CARTESIAN_POINT('Ctrl Pts',(0.00150220987593061,-0.0255377313926314,
-0.0101696185334625));
#34831=CARTESIAN_POINT('Ctrl Pts',(0.00164126741877263,-0.0255264152695477,
-0.0102817414029005));
#34832=CARTESIAN_POINT('Ctrl Pts',(0.001766681045625,-0.0255150991464641,
-0.0104070010928943));
#34833=CARTESIAN_POINT('Ctrl Pts',(0.00210936107218999,-0.0254841789868592,
-0.0107492605025924));
#34834=CARTESIAN_POINT('Ctrl Pts',(0.00235032903843675,-0.0254532588272541,
-0.0111949342399714));
#34835=CARTESIAN_POINT('Ctrl Pts',(0.00244848861379047,-0.0254223386676491,
-0.0116709735898595));
#34836=CARTESIAN_POINT('Ctrl Pts',(0.0024826045117403,-0.0254115921968552,
-0.0118364236727716));
#34837=CARTESIAN_POINT('Ctrl Pts',(0.00249988091828759,-0.0254008457260614,
-0.0120053122063183));
#34838=CARTESIAN_POINT('Ctrl Pts',(0.00249999938422522,-0.0253900992552675,
-0.0121740986146384));
#34839=CARTESIAN_POINT('',(0.00249999952816097,-0.024390152306814,-0.0121770295369509));
#34840=CARTESIAN_POINT('Ctrl Pts',(0.00249999999999008,-0.0253899883594716,
-0.0121758462427209));
#34841=CARTESIAN_POINT('Ctrl Pts',(0.00250000136839726,-0.0253591394204884,
-0.0126615215734826));
#34842=CARTESIAN_POINT('Ctrl Pts',(0.00235419002331737,-0.0253282841355819,
-0.0131471701041643));
#34843=CARTESIAN_POINT('Ctrl Pts',(0.00208688788741109,-0.0252974109206306,
-0.0135524065711704));
#34844=CARTESIAN_POINT('Ctrl Pts',(0.00199397450730698,-0.0252866794884028,
-0.0136932654900987));
#34845=CARTESIAN_POINT('Ctrl Pts',(0.00188683073616151,-0.025275945889803,
-0.0138245546547794));
#34846=CARTESIAN_POINT('Ctrl Pts',(0.00176778032757569,-0.0252652096383225,
-0.013943606864814));
#34847=CARTESIAN_POINT('Ctrl Pts',(0.00143339557831302,-0.0252350540193544,
-0.0142779966739247));
#34848=CARTESIAN_POINT('Ctrl Pts',(0.000999612545386808,-0.0252048774713678,
-0.0145159046057349));
#34849=CARTESIAN_POINT('Ctrl Pts',(0.000536244085537721,-0.0251747123357439,
-0.014617664557055));
#34850=CARTESIAN_POINT('Ctrl Pts',(0.000360026360796584,-0.0251632406193308,
-0.0146563635809317));
#34851=CARTESIAN_POINT('Ctrl Pts',(0.000179805506686608,-0.0251517705534416,
-0.0146758523796725));
#34852=CARTESIAN_POINT('Ctrl Pts',(1.26097002276545E-8,-0.0251403039168796,
-0.0146758532865263));
#34853=CARTESIAN_POINT('Ctrl Pts',(-0.000488388216285484,-0.0251091552182267,
-0.0146758557499615));
#34854=CARTESIAN_POINT('Ctrl Pts',(-0.000977672425016896,-0.0250780318251737,
-0.0145284407289839));
#34855=CARTESIAN_POINT('Ctrl Pts',(-0.00138584435671831,-0.0250468029969821,
-0.0142565828266358));
#34856=CARTESIAN_POINT('Ctrl Pts',(-0.00152303930767185,-0.0250363063478513,
-0.0141652058144451));
#34857=CARTESIAN_POINT('Ctrl Pts',(-0.00165119095954436,-0.0250257977869763,
-0.0140601956449662));
#34858=CARTESIAN_POINT('Ctrl Pts',(-0.00176776249477623,-0.0250152723496241,
-0.0139436246977034));
#34859=CARTESIAN_POINT('Ctrl Pts',(-0.00199945562318164,-0.024994352392594,
-0.0137119327379227));
#34860=CARTESIAN_POINT('Ctrl Pts',(-0.00218550612955122,-0.0249733657666968,
-0.0134323885029887));
#34861=CARTESIAN_POINT('Ctrl Pts',(-0.00230969762490276,-0.0249527093738166,
-0.0131325647799136));
#34862=CARTESIAN_POINT('Ctrl Pts',(-0.00237179337257852,-0.0249423811773765,
-0.0129826529183761));
#34863=CARTESIAN_POINT('Ctrl Pts',(-0.00241920188088303,-0.0249321355391907,
-0.0128282808273792));
#34864=CARTESIAN_POINT('Ctrl Pts',(-0.00245196289350594,-0.024921416087868,
-0.0126635806375135));
#34865=CARTESIAN_POINT('Ctrl Pts',(-0.00248472390612885,-0.0249106966365453,
-0.0124988804476478));
#34866=CARTESIAN_POINT('Ctrl Pts',(-0.00250000000000001,-0.0248995033720857,
-0.01232309132871));
#34867=CARTESIAN_POINT('Ctrl Pts',(-0.0025,-0.024890114936556,-0.012175853286558));
#34868=CARTESIAN_POINT('Ctrl Pts',(-0.00249999999999999,-0.0248807265010263,
-0.0120286152444059));
#34869=CARTESIAN_POINT('Ctrl Pts',(-0.00248916168542769,-0.0248731428944265,
-0.0119098588003648));
#34870=CARTESIAN_POINT('Ctrl Pts',(-0.00246883231316729,-0.0248649169214783,
-0.0117823218272553));
#34871=CARTESIAN_POINT('Ctrl Pts',(-0.0024485029409069,-0.0248566909485302,
-0.0116547848541457));
#34872=CARTESIAN_POINT('Ctrl Pts',(-0.00241621500340535,-0.0248478226092338,
-0.0115190288997562));
#34873=CARTESIAN_POINT('Ctrl Pts',(-0.00237210836288918,-0.0248389128968786,
-0.0113864852388698));
#34874=CARTESIAN_POINT('Ctrl Pts',(-0.00228389508185683,-0.0248210934721682,
-0.011121397917097));
#34875=CARTESIAN_POINT('Ctrl Pts',(-0.00215053058275203,-0.0248031085552227,
-0.0108678864920868));
#34876=CARTESIAN_POINT('Ctrl Pts',(-0.00197052077585615,-0.024784486819113,
-0.0106373319601153));
#34877=CARTESIAN_POINT('Ctrl Pts',(-0.00179051096896026,-0.0247658650830033,
-0.0104067774281438));
#34878=CARTESIAN_POINT('Ctrl Pts',(-0.00156298563825604,-0.0247466065277293,
-0.0102001638565565));
#34879=CARTESIAN_POINT('Ctrl Pts',(-0.00129778925817226,-0.0247268367032592,
-0.0100390933465151));
#34880=CARTESIAN_POINT('Ctrl Pts',(-0.00103259287808847,-0.0247070668787891,
-0.0098780228364736));
#34881=CARTESIAN_POINT('Ctrl Pts',(-0.000730081343127169,-0.0246867857851227,
-0.00976244661799695));
#34882=CARTESIAN_POINT('Ctrl Pts',(-0.00040649663987185,-0.0246659625493172,
-0.00970912255910265));
#34883=CARTESIAN_POINT('Ctrl Pts',(3.52049012454766E-5,-0.0246375382905256,
-0.00963633383097276));
#34884=CARTESIAN_POINT('Ctrl Pts',(0.000514584471571425,-0.0246081038604287,
-0.00968312478566572));
#34885=CARTESIAN_POINT('Ctrl Pts',(0.000956243946241907,-0.0245776671113977,
-0.00986596205204603));
#34886=CARTESIAN_POINT('Ctrl Pts',(0.00116169224343761,-0.0245635087413882,
-0.00995101310879009));
#34887=CARTESIAN_POINT('Ctrl Pts',(0.00135861700196376,-0.0245491334831793,
-0.0100648674701259));
#34888=CARTESIAN_POINT('Ctrl Pts',(0.00153853044578671,-0.0245345421271688,
-0.010205339630836));
#34889=CARTESIAN_POINT('Ctrl Pts',(0.00189055074869411,-0.0245059925454727,
-0.0104801887555733));
#34890=CARTESIAN_POINT('Ctrl Pts',(0.00218016631731741,-0.0244766156723194,
-0.0108631077290133));
#34891=CARTESIAN_POINT('Ctrl Pts',(0.00234507266630632,-0.02444640953421,
-0.0113094618105249));
#34892=CARTESIAN_POINT('Ctrl Pts',(0.00244562968209433,-0.0244279903579601,
-0.011581640745398));
#34893=CARTESIAN_POINT('Ctrl Pts',(0.0025000009689668,-0.0244092628321647,
-0.01187638284372));
#34894=CARTESIAN_POINT('Ctrl Pts',(0.00249999999998691,-0.024390226509356,
-0.0121758613754508));
#34895=CARTESIAN_POINT('',(0.00249999997439014,-0.023390082751053,-0.0121756050547064));
#34896=CARTESIAN_POINT('Ctrl Pts',(0.00249999919082622,-0.0243900992552675,
-0.0121778647209288));
#34897=CARTESIAN_POINT('Ctrl Pts',(0.00249960845783168,-0.0243591775128979,
-0.0126635043144498));
#34898=CARTESIAN_POINT('Ctrl Pts',(0.00235342576395591,-0.0243282557705284,
-0.0131490022570672));
#34899=CARTESIAN_POINT('Ctrl Pts',(0.00208583353260368,-0.0242973340281588,
-0.0135540036681442));
#34900=CARTESIAN_POINT('Ctrl Pts',(0.00199284853085276,-0.0242865891038617,
-0.0136947366659888));
#34901=CARTESIAN_POINT('Ctrl Pts',(0.0018856518032898,-0.0242758441795646,
-0.0138258961121601));
#34902=CARTESIAN_POINT('Ctrl Pts',(0.00176656675632587,-0.0242650992552675,
-0.0139448196218636));
#34903=CARTESIAN_POINT('Ctrl Pts',(0.00143017696340042,-0.0242347471417868,
-0.0142807531065711));
#34904=CARTESIAN_POINT('Ctrl Pts',(0.00099359785863377,-0.0242043950283061,
-0.0145189828434659));
#34905=CARTESIAN_POINT('Ctrl Pts',(0.000527368666328687,-0.0241740429148254,
-0.0146195967857361));
#34906=CARTESIAN_POINT('Ctrl Pts',(0.000353569402019352,-0.0241627283616394,
-0.0146571032941968));
#34907=CARTESIAN_POINT('Ctrl Pts',(0.000175914055471926,-0.0241514138084535,
-0.0146759509197155));
#34908=CARTESIAN_POINT('Ctrl Pts',(-1.38208273950699E-6,-0.0241400992552675,
-0.0146758529045275));
#34909=CARTESIAN_POINT('Ctrl Pts',(-0.000478750851133147,-0.0241096348899757,
-0.0146755889992331));
#34910=CARTESIAN_POINT('Ctrl Pts',(-0.000957571928518442,-0.0240791705246838,
-0.0145342776525842));
#34911=CARTESIAN_POINT('Ctrl Pts',(-0.00135929122746163,-0.024048706159392,
-0.0142740256719797));
#34912=CARTESIAN_POINT('Ctrl Pts',(-0.00150701072241057,-0.0240375038580171,
-0.0141783262837863));
#34913=CARTESIAN_POINT('Ctrl Pts',(-0.00164444690479554,-0.0240263015566424,
-0.0140670459612177));
#34914=CARTESIAN_POINT('Ctrl Pts',(-0.00176852156248608,-0.0240150992552675,
-0.0139428653077458));
#34915=CARTESIAN_POINT('Ctrl Pts',(-0.00210587590077154,-0.0239846406182023,
-0.0136052227709083));
#34916=CARTESIAN_POINT('Ctrl Pts',(-0.0023445600348803,-0.0239541819811371,
-0.0131668393892154));
#34917=CARTESIAN_POINT('Ctrl Pts',(-0.00244467776727557,-0.023923723344072,
-0.0126988739498101));
#34918=CARTESIAN_POINT('Ctrl Pts',(-0.00248151863136018,-0.0239125153144705,
-0.0125266741732374));
#34919=CARTESIAN_POINT('Ctrl Pts',(-0.00250005276538172,-0.023901307284869,
-0.0123507233831673));
#34920=CARTESIAN_POINT('Ctrl Pts',(-0.0024999998866792,-0.0238900992552675,
-0.0121751005555373));
#34921=CARTESIAN_POINT('Ctrl Pts',(-0.00249985618495232,-0.0238596406182022,
-0.0116978327254759));
#34922=CARTESIAN_POINT('Ctrl Pts',(-0.00235872289837664,-0.0238291819811368,
-0.0112190599612614));
#34923=CARTESIAN_POINT('Ctrl Pts',(-0.00209866256915363,-0.0237987233440715,
-0.0108173189951861));
#34924=CARTESIAN_POINT('Ctrl Pts',(-0.00200296676169467,-0.0237875153144702,
-0.010669488196645));
#34925=CARTESIAN_POINT('Ctrl Pts',(-0.00189167007198695,-0.0237763072848689,
-0.0105319459848342));
#34926=CARTESIAN_POINT('Ctrl Pts',(-0.00176745717406797,-0.0237650992552675,
-0.0104077766089687));
#34927=CARTESIAN_POINT('Ctrl Pts',(-0.00142983609072378,-0.0237346348899757,
-0.0100702738222191));
#34928=CARTESIAN_POINT('Ctrl Pts',(-0.000991418463670934,-0.0237041705246839,
-0.00983145743438289));
#34929=CARTESIAN_POINT('Ctrl Pts',(-0.000523378534922975,-0.023673706159392,
-0.00973125211066419));
#34930=CARTESIAN_POINT('Ctrl Pts',(-0.000351271737782169,-0.0236625038580172,
-0.00969440479003534));
#34931=CARTESIAN_POINT('Ctrl Pts',(-0.000175413828559905,-0.0236513015566424,
-0.00967584462654266));
#34932=CARTESIAN_POINT('Ctrl Pts',(1.23379254317394E-7,-0.0236400992552675,
-0.00967585328960259));
#34933=CARTESIAN_POINT('Ctrl Pts',(0.000475733262739959,-0.0236097471417868,
-0.00967587676175972));
#34934=CARTESIAN_POINT('Ctrl Pts',(0.000953014801081544,-0.0235793950283061,
-0.00981594521882193));
#34935=CARTESIAN_POINT('Ctrl Pts',(0.0013538998578098,-0.0235490429148253,
-0.0100741979449232));
#34936=CARTESIAN_POINT('Ctrl Pts',(0.00150334036707393,-0.0235377283616394,
-0.0101704684799798));
#34937=CARTESIAN_POINT('Ctrl Pts',(0.00164230892020507,-0.0235264138084535,
-0.0102826474887713));
#34938=CARTESIAN_POINT('Ctrl Pts',(0.0017676316806438,-0.0235150992552675,
-0.0104079510716196));
#34939=CARTESIAN_POINT('Ctrl Pts',(0.00211012846753573,-0.0234841775128981,
-0.0107503954477357));
#34940=CARTESIAN_POINT('Ctrl Pts',(0.00235085694096267,-0.0234532557705288,
-0.0111961996941204));
#34941=CARTESIAN_POINT('Ctrl Pts',(0.00244876022617186,-0.0234223340281594,
-0.0116722926102551));
#34942=CARTESIAN_POINT('Ctrl Pts',(0.00248278041091645,-0.0234115891038621,
-0.0118377290297571));
#34943=CARTESIAN_POINT('Ctrl Pts',(0.00249996579487876,-0.0234008441795648,
-0.0120065934906643));
#34944=CARTESIAN_POINT('Ctrl Pts',(0.00249999994879836,-0.0233900992552675,
-0.0121753473140382));
#34945=CARTESIAN_POINT('',(0.00249999978282922,-0.0223900527209141,-0.0121751135025362));
#34946=CARTESIAN_POINT('Ctrl Pts',(0.00249999999998192,-0.0233900662468386,
-0.0121758627953746));
#34947=CARTESIAN_POINT('Ctrl Pts',(0.00249999815284274,-0.0233591476370275,
-0.0126615013552356));
#34948=CARTESIAN_POINT('Ctrl Pts',(0.00235420495401003,-0.0233282290272166,
-0.01314711521106));
#34949=CARTESIAN_POINT('Ctrl Pts',(0.00208693825047046,-0.0232973104174055,
-0.0135523302165222));
#34950=CARTESIAN_POINT('Ctrl Pts',(0.00199404176653275,-0.0232865637359011,
-0.0136931747315616));
#34951=CARTESIAN_POINT('Ctrl Pts',(0.00188691839382461,-0.0232758170543966,
-0.0138244520404621));
#34952=CARTESIAN_POINT('Ctrl Pts',(0.00176789131965712,-0.0232650703728922,
-0.0139434958640836));
#34953=CARTESIAN_POINT('Ctrl Pts',(0.0014317551106563,-0.0232347214056046,
-0.0142796793740706));
#34954=CARTESIAN_POINT('Ctrl Pts',(0.000995357070768357,-0.0232043724383171,
-0.0145182356543401));
#34955=CARTESIAN_POINT('Ctrl Pts',(0.000529205667740109,-0.0231740234710294,
-0.0146191996314777));
#34956=CARTESIAN_POINT('Ctrl Pts',(0.0003553901875384,-0.0231627071470016,
-0.0146568464175974));
#34957=CARTESIAN_POINT('Ctrl Pts',(0.000177702613060415,-0.0231513908229737,
-0.0146758276322675));
#34958=CARTESIAN_POINT('Ctrl Pts',(3.61283311594722E-7,-0.0231400744989458,
-0.014675853260453));
#34959=CARTESIAN_POINT('Ctrl Pts',(-0.000477005090471533,-0.0231096132828639,
-0.0146759222462554));
#34960=CARTESIAN_POINT('Ctrl Pts',(-0.00095592265976367,-0.0230791520667819,
-0.014534946223913));
#34961=CARTESIAN_POINT('Ctrl Pts',(-0.00135782237193734,-0.0230486908507,
-0.0142749765335987));
#34962=CARTESIAN_POINT('Ctrl Pts',(-0.00150564689080733,-0.0230374867754665,
-0.0141793559266975));
#34963=CARTESIAN_POINT('Ctrl Pts',(-0.00164319368247117,-0.023026282700233,
-0.0140681391251308));
#34964=CARTESIAN_POINT('Ctrl Pts',(-0.00176738035000952,-0.0230150786249995,
-0.0139440067579514));
#34965=CARTESIAN_POINT('Ctrl Pts',(-0.00210495091791582,-0.0229846231331628,
-0.0136065837920654));
#34966=CARTESIAN_POINT('Ctrl Pts',(-0.0023439176592855,-0.0229541676413262,
-0.0131683568875582));
#34967=CARTESIAN_POINT('Ctrl Pts',(-0.00244433827125326,-0.0229237121494896,
-0.0127004582957666));
#34968=CARTESIAN_POINT('Ctrl Pts',(-0.00248130023954904,-0.0229125023500108,
-0.0125282381451764));
#34969=CARTESIAN_POINT('Ctrl Pts',(-0.002499948451974,-0.0229012925505319,
-0.0123522531780084));
#34970=CARTESIAN_POINT('Ctrl Pts',(-0.00249999989281311,-0.0228900827510531,
-0.0121765853619898));
#34971=CARTESIAN_POINT('Ctrl Pts',(-0.00250013965053656,-0.0228596272592165,
-0.0116993199348243));
#34972=CARTESIAN_POINT('Ctrl Pts',(-0.00235929209470182,-0.02282917176738,
-0.0112204653179175));
#34973=CARTESIAN_POINT('Ctrl Pts',(-0.00209947244932243,-0.0227987162755435,
-0.0108185709155917));
#34974=CARTESIAN_POINT('Ctrl Pts',(-0.00200384023490871,-0.0227875064760646,
-0.0106706450280063));
#34975=CARTESIAN_POINT('Ctrl Pts',(-0.00189259294181167,-0.0227762966765856,
-0.0105330037373359));
#34976=CARTESIAN_POINT('Ctrl Pts',(-0.0017684155842339,-0.0227650868771067,
-0.0104087352029432));
#34977=CARTESIAN_POINT('Ctrl Pts',(-0.00143097927872439,-0.0227346256610247,
-0.0100710511359404));
#34978=CARTESIAN_POINT('Ctrl Pts',(-0.000992693544891953,-0.0227041644449427,
-0.00983199746057321));
#34979=CARTESIAN_POINT('Ctrl Pts',(-0.000524710188623356,-0.0226737032288607,
-0.00973153759132664));
#34980=CARTESIAN_POINT('Ctrl Pts',(-0.000352579150994395,-0.0226624991536272,
-0.0096945870004523));
#34981=CARTESIAN_POINT('Ctrl Pts',(-0.000176685099276302,-0.0226512950783938,
-0.00967593098740631));
#34982=CARTESIAN_POINT('Ctrl Pts',(-1.10286753579808E-6,-0.0226400910031603,
-0.00967585352982147));
#34983=CARTESIAN_POINT('Ctrl Pts',(0.000474504382178306,-0.0226097420358727,
-0.00967564371708286));
#34984=CARTESIAN_POINT('Ctrl Pts',(0.000951852528106953,-0.0225793930685852,
-0.00981547660079706));
#34985=CARTESIAN_POINT('Ctrl Pts',(0.00135286317164378,-0.0225490441012976,
-0.0100735304667205));
#34986=CARTESIAN_POINT('Ctrl Pts',(0.00150238939235155,-0.0225377277772697,
-0.0101697519010701));
#34987=CARTESIAN_POINT('Ctrl Pts',(0.0016414461183173,-0.0225264114532418,
-0.0102818951503619));
#34988=CARTESIAN_POINT('Ctrl Pts',(0.00176685577834738,-0.0225150951292139,
-0.0104071756283851));
#34989=CARTESIAN_POINT('Ctrl Pts',(0.00210950170607601,-0.0224841765194028,
-0.0107494686033299));
#34990=CARTESIAN_POINT('Ctrl Pts',(0.00235042559911038,-0.0224532579095917,
-0.0111951657732823));
#34991=CARTESIAN_POINT('Ctrl Pts',(0.00244853827886408,-0.0224223392997806,
-0.0116712145078883));
#34992=CARTESIAN_POINT('Ctrl Pts',(0.0024826402558706,-0.0224115926182762,
-0.0118366793901265));
#34993=CARTESIAN_POINT('Ctrl Pts',(0.00249990006528172,-0.0224008459367719,
-0.0120055815453249));
#34994=CARTESIAN_POINT('Ctrl Pts',(0.00249999956566543,-0.0223900992552675,
-0.0121743796269425));
#34995=CARTESIAN_POINT('',(0.00249999946670881,-0.0213901564165093,-0.012177099742631));
#34996=CARTESIAN_POINT('Ctrl Pts',(0.00249999999999302,-0.0223900061865608,
-0.0121758473781298));
#34997=CARTESIAN_POINT('Ctrl Pts',(0.00250000114022626,-0.0223593773858453,
-0.0126583078509963));
#34998=CARTESIAN_POINT('Ctrl Pts',(0.00235604930438737,-0.0223287344743284,
-0.0131410200720147));
#34999=CARTESIAN_POINT('Ctrl Pts',(0.00209205887758274,-0.0222980771500896,
-0.0135445350073125));
#35000=CARTESIAN_POINT('Ctrl Pts',(0.00199792613435286,-0.0222871454732647,
-0.0136884188907304));
#35001=CARTESIAN_POINT('Ctrl Pts',(0.00188900128248741,-0.0222762119639099,
-0.0138223841604978));
#35002=CARTESIAN_POINT('Ctrl Pts',(0.0017677797086252,-0.0222652766083368,
-0.0139436074837736));
#35003=CARTESIAN_POINT('Ctrl Pts',(0.00143008399010385,-0.0222348131962569,
-0.0142813080757631));
#35004=CARTESIAN_POINT('Ctrl Pts',(0.000991179767819557,-0.0222043354565482,
-0.0145205707095847));
#35005=CARTESIAN_POINT('Ctrl Pts',(0.000522028801479781,-0.0221738442769973,
-0.014620743044896));
#35006=CARTESIAN_POINT('Ctrl Pts',(0.000350468005067636,-0.0221626941538544,
-0.0146573744212706));
#35007=CARTESIAN_POINT('Ctrl Pts',(0.000175121182212468,-0.0221515422334758,
-0.0146758524441749));
#35008=CARTESIAN_POINT('Ctrl Pts',(1.20261312456349E-8,-0.0221403885592749,
-0.0146758532865292));
#35009=CARTESIAN_POINT('Ctrl Pts',(-0.000326969715656887,-0.0221195612770291,
-0.0146758548594593));
#35010=CARTESIAN_POINT('Ctrl Pts',(-0.000654265414087993,-0.0220987278795242,
-0.0146108269010241));
#35011=CARTESIAN_POINT('Ctrl Pts',(-0.000956700247905833,-0.0220778855401309,
-0.0144855555694632));
#35012=CARTESIAN_POINT('Ctrl Pts',(-0.00125913508172367,-0.0220570432007376,
-0.0143602842379022));
#35013=CARTESIAN_POINT('Ctrl Pts',(-0.00153644332769053,-0.0220361919194559,
-0.0141749427520477));
#35014=CARTESIAN_POINT('Ctrl Pts',(-0.00176776270110393,-0.0220153431912449,
-0.0139436244913767));
#35015=CARTESIAN_POINT('Ctrl Pts',(-0.00188342238781062,-0.0220049188271394,
-0.0138279653610412));
#35016=CARTESIAN_POINT('Ctrl Pts',(-0.00198770652448018,-0.0219944951013015,
-0.0137009208315779));
#35017=CARTESIAN_POINT('Ctrl Pts',(-0.00207867152525912,-0.0219840572681485,
-0.0135647826188414));
#35018=CARTESIAN_POINT('Ctrl Pts',(-0.00216963652603806,-0.0219736194349956,
-0.0134286444061049));
#35019=CARTESIAN_POINT('Ctrl Pts',(-0.00224723455883184,-0.0219631674945277,
-0.013283363448231));
#35020=CARTESIAN_POINT('Ctrl Pts',(-0.00230969768073528,-0.0219527615126167,
-0.0131325646451225));
#35021=CARTESIAN_POINT('Ctrl Pts',(-0.00237216080263872,-0.0219423555307058,
-0.0129817658420139));
#35022=CARTESIAN_POINT('Ctrl Pts',(-0.00241973422772398,-0.0219319955073519,
-0.0128256045726092));
#35023=CARTESIAN_POINT('Ctrl Pts',(-0.0024519629077376,-0.0219214559246494,
-0.0126635805659663));
#35024=CARTESIAN_POINT('Ctrl Pts',(-0.00246807724774441,-0.0219161861332981,
-0.0125825685626449));
#35025=CARTESIAN_POINT('Ctrl Pts',(-0.00248016729986118,-0.0219108714521097,
-0.0125000349508198));
#35026=CARTESIAN_POINT('Ctrl Pts',(-0.00248796174300818,-0.0219057994435024,
-0.0124208968853884));
#35027=CARTESIAN_POINT('Ctrl Pts',(-0.00249185896458168,-0.0219032634391987,
-0.0123813278526727));
#35028=CARTESIAN_POINT('Ctrl Pts',(-0.00249482184802687,-0.0219007881030403,
-0.0123426284113902));
#35029=CARTESIAN_POINT('Ctrl Pts',(-0.00249698862207265,-0.021897970281138,
-0.0122985228477366));
#35030=CARTESIAN_POINT('Ctrl Pts',(-0.00249915539611843,-0.0218951524592358,
-0.012254417284083));
#35031=CARTESIAN_POINT('Ctrl Pts',(-0.0025,-0.0218919921515896,-0.0122048746012686));
#35032=CARTESIAN_POINT('Ctrl Pts',(-0.0025,-0.0218901405042465,-0.012175853286558));
#35033=CARTESIAN_POINT('Ctrl Pts',(-0.0025,-0.0218882888569033,-0.0121468319718473));
#35034=CARTESIAN_POINT('Ctrl Pts',(-0.00249975948868643,-0.0218877458698631,
-0.0121383237374989));
#35035=CARTESIAN_POINT('Ctrl Pts',(-0.00249946167551239,-0.0218868304812657,
-0.0121239752310355));
#35036=CARTESIAN_POINT('Ctrl Pts',(-0.00249916386233835,-0.0218859150926683,
-0.0121096267245721));
#35037=CARTESIAN_POINT('Ctrl Pts',(-0.00249858311755661,-0.0218846273025136,
-0.0120894460511038));
#35038=CARTESIAN_POINT('Ctrl Pts',(-0.0024977526130494,-0.0218833775691218,
-0.0120698727034076));
#35039=CARTESIAN_POINT('Ctrl Pts',(-0.00249609160403497,-0.0218808781023383,
-0.0120307260080153));
#35040=CARTESIAN_POINT('Ctrl Pts',(-0.0024936817236808,-0.0218785308626062,
-0.0119939903198025));
#35041=CARTESIAN_POINT('Ctrl Pts',(-0.00249023640476994,-0.0218760430773448,
-0.0119551212128613));
#35042=CARTESIAN_POINT('Ctrl Pts',(-0.00248334576694822,-0.0218710675068219,
-0.011877382998979));
#35043=CARTESIAN_POINT('Ctrl Pts',(-0.00247194153334508,-0.0218655297541816,
-0.0117911618818107));
#35044=CARTESIAN_POINT('Ctrl Pts',(-0.00245443835988697,-0.0218596594238335,
-0.0117007403131346));
#35045=CARTESIAN_POINT('Ctrl Pts',(-0.00243693518642886,-0.0218537890934854,
-0.0116103187444584));
#35046=CARTESIAN_POINT('Ctrl Pts',(-0.00241347394517101,-0.0218475861854294,
-0.0115156557012848));
#35047=CARTESIAN_POINT('Ctrl Pts',(-0.00238205060024122,-0.0218409895437126,
-0.0114170154001222));
#35048=CARTESIAN_POINT('Ctrl Pts',(-0.00235062725531143,-0.0218343929019958,
-0.0113183750989597));
#35049=CARTESIAN_POINT('Ctrl Pts',(-0.00231120270368248,-0.0218274025266182,
-0.0112157783033761));
#35050=CARTESIAN_POINT('Ctrl Pts',(-0.00226189465481612,-0.0218200334369823,
-0.0111110375416922));
#35051=CARTESIAN_POINT('Ctrl Pts',(-0.0021632785570834,-0.0218052952577104,
-0.0109015560183245));
#35052=CARTESIAN_POINT('Ctrl Pts',(-0.00202509411853232,-0.0217890422214056,
-0.0106835381773548));
#35053=CARTESIAN_POINT('Ctrl Pts',(-0.001835460791482,-0.0217712625436928,
-0.0104784777585937));
#35054=CARTESIAN_POINT('Ctrl Pts',(-0.00164582746443168,-0.02175348286598,
-0.0102734173398327));
#35055=CARTESIAN_POINT('Ctrl Pts',(-0.00140431280704041,-0.0217341765468593,
-0.0100818042152198));
#35056=CARTESIAN_POINT('Ctrl Pts',(-0.00111110002761456,-0.0217133467439652,
-0.00993633174644402));
#35057=CARTESIAN_POINT('Ctrl Pts',(-0.00081788724818871,-0.021692516941071,
-0.00979085927766821));
#35058=CARTESIAN_POINT('Ctrl Pts',(-0.000472595108618116,-0.0216701636544036,
-0.0096924156088888));
#35059=CARTESIAN_POINT('Ctrl Pts',(-9.76363564151474E-5,-0.0216462860377993,
-0.00967776058573494));
#35060=CARTESIAN_POINT('Ctrl Pts',(0.000277322395787821,-0.0216224084211949,
-0.00966310556258107));
#35061=CARTESIAN_POINT('Ctrl Pts',(0.000681901047087343,-0.0215970064746537,
-0.00973369490722545));
#35062=CARTESIAN_POINT('Ctrl Pts',(0.00106482420138709,-0.0215700804251951,
-0.00991396261277646));
#35063=CARTESIAN_POINT('Ctrl Pts',(0.00144774735568684,-0.0215431543757365,
-0.0100942303183275));
#35064=CARTESIAN_POINT('Ctrl Pts',(0.00180788869735316,-0.0215147042233605,
-0.0103860811844988));
#35065=CARTESIAN_POINT('Ctrl Pts',(0.00207151346256511,-0.0214847299061527,
-0.010776270500721));
#35066=CARTESIAN_POINT('Ctrl Pts',(0.00231596365811457,-0.0214569357507098,
-0.0111380796599445));
#35067=CARTESIAN_POINT('Ctrl Pts',(0.00247586744117682,-0.0214278310853771,
-0.0115853104295833));
#35068=CARTESIAN_POINT('Ctrl Pts',(0.00249745187057231,-0.0213974159266089,
-0.0120630075769592));
#35069=CARTESIAN_POINT('Ctrl Pts',(0.00249914479383464,-0.0213950303861407,
-0.0121004746138832));
#35070=CARTESIAN_POINT('Ctrl Pts',(0.00250000013050565,-0.0213926367839425,
-0.0121381054938293));
#35071=CARTESIAN_POINT('Ctrl Pts',(0.00249999999998506,-0.0213902351200221,
-0.0121758619288322));
#35072=CARTESIAN_POINT('',(0.00249990205332692,-0.0203902475809712,-0.012175258225647));
#35073=CARTESIAN_POINT('Ctrl Pts',(0.00249999907939785,-0.0213900992552675,
-0.0121779987491857));
#35074=CARTESIAN_POINT('Ctrl Pts',(0.00249958231006304,-0.0213591763542908,
-0.0126636389742638));
#35075=CARTESIAN_POINT('Ctrl Pts',(0.00235337321701218,-0.021328253453314,
-0.0131491296217983));
#35076=CARTESIAN_POINT('Ctrl Pts',(0.00208575865386121,-0.0212973305523372,
-0.0135541169905869));
#35077=CARTESIAN_POINT('Ctrl Pts',(0.00199277940318017,-0.0212865867866473,
-0.0136948246622542));
#35078=CARTESIAN_POINT('Ctrl Pts',(0.00188559305150799,-0.0212758430209575,
-0.0138259607867651));
#35079=CARTESIAN_POINT('Ctrl Pts',(0.00176652209780973,-0.0212650992552675,
-0.0139448642186752));
#35080=CARTESIAN_POINT('Ctrl Pts',(0.00143012280556268,-0.0212347459653853,
-0.0142807902283188));
#35081=CARTESIAN_POINT('Ctrl Pts',(0.000993536318349333,-0.0212043926755031,
-0.0145190091690837));
#35082=CARTESIAN_POINT('Ctrl Pts',(0.000527303328876991,-0.0211740393856209,
-0.0146196108848798));
#35083=CARTESIAN_POINT('Ctrl Pts',(0.000353527454837905,-0.0211627260088364,
-0.0146571074831195));
#35084=CARTESIAN_POINT('Ctrl Pts',(0.000175897082413975,-0.021151412632052,
-0.0146759503570788));
#35085=CARTESIAN_POINT('Ctrl Pts',(-1.37428056251401E-6,-0.0211400992552675,
-0.0146758529088287));
#35086=CARTESIAN_POINT('Ctrl Pts',(-0.000478744400520623,-0.0211096337139525,
-0.0146755904925982));
#35087=CARTESIAN_POINT('Ctrl Pts',(-0.000957566979565421,-0.0210791681726375,
-0.0145342798794274));
#35088=CARTESIAN_POINT('Ctrl Pts',(-0.00135928762466615,-0.0210487026313225,
-0.0142740280060296));
#35089=CARTESIAN_POINT('Ctrl Pts',(-0.00150698640525244,-0.0210375015059708,
-0.0141783423975977));
#35090=CARTESIAN_POINT('Ctrl Pts',(-0.00164440482203652,-0.0210263003806192,
-0.0140670802591278));
#35091=CARTESIAN_POINT('Ctrl Pts',(-0.00176846592375923,-0.0210150992552675,
-0.0139429209922509));
#35092=CARTESIAN_POINT('Ctrl Pts',(-0.00210583182168066,-0.0209846394442589,
-0.0136052881486477));
#35093=CARTESIAN_POINT('Ctrl Pts',(-0.00234452996584051,-0.0209541796332503,
-0.0131669110301521));
#35094=CARTESIAN_POINT('Ctrl Pts',(-0.00244466201221942,-0.0209237198222416,
-0.012698947585907));
#35095=CARTESIAN_POINT('Ctrl Pts',(-0.00248150286425866,-0.0209125129665836,
-0.012526773215836));
#35096=CARTESIAN_POINT('Ctrl Pts',(-0.00250004228843935,-0.0209013061109256,
-0.0123508483409523));
#35097=CARTESIAN_POINT('Ctrl Pts',(-0.00249999992725447,-0.0208900992552675,
-0.0121752501881915));
#35098=CARTESIAN_POINT('Ctrl Pts',(-0.00249988479115165,-0.0208596394442589,
-0.0116979810317242));
#35099=CARTESIAN_POINT('Ctrl Pts',(-0.00235877941875351,-0.0208291796332502,
-0.0112191987874848));
#35100=CARTESIAN_POINT('Ctrl Pts',(-0.00209874201892454,-0.0207987198222416,
-0.0108174417369898));
#35101=CARTESIAN_POINT('Ctrl Pts',(-0.00200306835881087,-0.0207875129665835,
-0.0106696262015222));
#35102=CARTESIAN_POINT('Ctrl Pts',(-0.00189179763511228,-0.0207763061109256,
-0.0105320954221778));
#35103=CARTESIAN_POINT('Ctrl Pts',(-0.00176761314542966,-0.0207650992552675,
-0.0104079325394361));
#35104=CARTESIAN_POINT('Ctrl Pts',(-0.001430020887926,-0.0207346337139525,
-0.0100703990198312));
#35105=CARTESIAN_POINT('Ctrl Pts',(-0.000991623047142472,-0.0207041681726375,
-0.00983154374161374));
#35106=CARTESIAN_POINT('Ctrl Pts',(-0.000523590769440504,-0.0206737026313225,
-0.00973129755879146));
#35107=CARTESIAN_POINT('Ctrl Pts',(-0.000351511496107748,-0.0206625015059708,
-0.00969444050615581));
#35108=CARTESIAN_POINT('Ctrl Pts',(-0.00017568058482422,-0.0206513003806192,
-0.00967586509253789));
#35109=CARTESIAN_POINT('Ctrl Pts',(-1.68083886645815E-7,-0.0206400992552675,
-0.00967585329220854));
#35110=CARTESIAN_POINT('Ctrl Pts',(0.000475443218696623,-0.0206097459653853,
-0.00967582131516996));
#35111=CARTESIAN_POINT('Ctrl Pts',(0.000952742201519874,-0.0205793926755031,
-0.0098158349233419));
#35112=CARTESIAN_POINT('Ctrl Pts',(0.00135365793268781,-0.0205490393856208,
-0.0100740421149084));
#35113=CARTESIAN_POINT('Ctrl Pts',(0.00150308854607822,-0.0205377260088364,
-0.0101702819379386));
#35114=CARTESIAN_POINT('Ctrl Pts',(0.00164205199002488,-0.020526412632052,
-0.0102824269558209));
#35115=CARTESIAN_POINT('Ctrl Pts',(0.00176737540225734,-0.0205150992552675,
-0.0104076948695898));
#35116=CARTESIAN_POINT('Ctrl Pts',(0.00210992241897826,-0.0204841763542906,
-0.0107500901921239));
#35117=CARTESIAN_POINT('Ctrl Pts',(0.0023507156029587,-0.0204532534533137,
-0.0111958603106268));
#35118=CARTESIAN_POINT('Ctrl Pts',(0.00244868762262492,-0.0204223305523368,
-0.0116719396761014));
#35119=CARTESIAN_POINT('Ctrl Pts',(0.00248272674541716,-0.020411586786647,
-0.0118373473510217));
#35120=CARTESIAN_POINT('Ctrl Pts',(0.00249993643078121,-0.0204008430209573,
-0.0120061844971346));
#35121=CARTESIAN_POINT('Ctrl Pts',(0.00249999982355582,-0.0203900992552675,
-0.0121749140204342));
#35122=CARTESIAN_POINT('',(0.00249999986986764,-0.0193900632541159,-0.0121752806287112));
#35123=CARTESIAN_POINT('Ctrl Pts',(0.00249999999995715,-0.0203900382015828,
-0.0121758679244561));
#35124=CARTESIAN_POINT('Ctrl Pts',(0.00249999715646827,-0.0203591211281684,
-0.012661506106886));
#35125=CARTESIAN_POINT('Ctrl Pts',(0.00235420317554791,-0.0203282040547541,
-0.0131471193498656));
#35126=CARTESIAN_POINT('Ctrl Pts',(0.00208693599846101,-0.0202972869813398,
-0.0135523336308884));
#35127=CARTESIAN_POINT('Ctrl Pts',(0.00199403155362639,-0.020286539931991,
-0.0136931897144067));
#35128=CARTESIAN_POINT('Ctrl Pts',(0.00188689786182557,-0.0202757928826422,
-0.013824476965648));
#35129=CARTESIAN_POINT('Ctrl Pts',(0.00176785872255326,-0.0202650458332934,
-0.0139435284651733));
#35130=CARTESIAN_POINT('Ctrl Pts',(0.00143171690229952,-0.0202346983967062,
-0.0142797051882159));
#35131=CARTESIAN_POINT('Ctrl Pts',(0.000995315253905716,-0.0202043509601189,
-0.0145182532900219));
#35132=CARTESIAN_POINT('Ctrl Pts',(0.000529162715761184,-0.0201740035235317,
-0.0146192089340741));
#35133=CARTESIAN_POINT('Ctrl Pts',(0.000355332482386485,-0.0201626868373558,
-0.0146568557164684));
#35134=CARTESIAN_POINT('Ctrl Pts',(0.000177629853437843,-0.0201513701511799,
-0.0146758338185694));
#35135=CARTESIAN_POINT('Ctrl Pts',(2.74208224093162E-7,-0.020140053465004,
-0.0146758532715201));
#35136=CARTESIAN_POINT('Ctrl Pts',(-0.000477091387164691,-0.0201095937825525,
-0.0146759056305492));
#35137=CARTESIAN_POINT('Ctrl Pts',(-0.000956003432813248,-0.020079134100101,
-0.0145349133668213));
#35138=CARTESIAN_POINT('Ctrl Pts',(-0.0013578937810368,-0.0200486744176495,
-0.0142749303407468));
#35139=CARTESIAN_POINT('Ctrl Pts',(-0.00150572711533615,-0.0200374699773378,
-0.0141792968980038));
#35140=CARTESIAN_POINT('Ctrl Pts',(-0.00164328050466185,-0.0200262655370262,
-0.0140680650532317));
#35141=CARTESIAN_POINT('Ctrl Pts',(-0.00176747091116223,-0.0200150610967145,
-0.0139439162317598));
#35142=CARTESIAN_POINT('Ctrl Pts',(-0.00210502365928357,-0.019984607137146,
-0.0136064765128253));
#35143=CARTESIAN_POINT('Ctrl Pts',(-0.00234396783479502,-0.0199541531775775,
-0.0131682380928252));
#35144=CARTESIAN_POINT('Ctrl Pts',(-0.00244436472397797,-0.019923699218009,
-0.0127003350271098));
#35145=CARTESIAN_POINT('Ctrl Pts',(-0.00248132101892018,-0.0199124890548144,
-0.0125280989763549));
#35146=CARTESIAN_POINT('Ctrl Pts',(-0.00249996036917035,-0.0199012788916198,
-0.0123520984181568));
#35147=CARTESIAN_POINT('Ctrl Pts',(-0.00249999993659396,-0.0198900687284252,
-0.0121764163409007));
#35148=CARTESIAN_POINT('Ctrl Pts',(-0.00250010742697549,-0.0198596147688566,
-0.0116991516673366));
#35149=CARTESIAN_POINT('Ctrl Pts',(-0.00235922792536984,-0.0198291608092881,
-0.0112203071714482));
#35150=CARTESIAN_POINT('Ctrl Pts',(-0.00209938175411062,-0.0197987068497195,
-0.0108184306366412));
#35151=CARTESIAN_POINT('Ctrl Pts',(-0.00200373186074464,-0.0197874966865249,
-0.0106704990834677));
#35152=CARTESIAN_POINT('Ctrl Pts',(-0.00189246502018833,-0.0197762865233303,
-0.0105328548560365));
#35153=CARTESIAN_POINT('Ctrl Pts',(-0.0017682671442481,-0.0197650763601357,
-0.0104085866664431));
#35154=CARTESIAN_POINT('Ctrl Pts',(-0.00143080302382207,-0.0197346166776842,
-0.0100709314933526));
#35155=CARTESIAN_POINT('Ctrl Pts',(-0.000992497953249737,-0.0197041569952327,
-0.00983191475799308));
#35156=CARTESIAN_POINT('Ctrl Pts',(-0.000524506848390027,-0.0196736973127811,
-0.00973149395004639));
#35157=CARTESIAN_POINT('Ctrl Pts',(-0.000352358684694864,-0.0196624928724695,
-0.00969455466315548));
#35158=CARTESIAN_POINT('Ctrl Pts',(-0.000176448413992738,-0.0196512884321579,
-0.00967591326800827));
#35159=CARTESIAN_POINT('Ctrl Pts',(-8.51900453529701E-7,-0.0196400839918463,
-0.00967585343170498));
#35160=CARTESIAN_POINT('Ctrl Pts',(0.000474754547648577,-0.019609736555259,
-0.00967569136395604));
#35161=CARTESIAN_POINT('Ctrl Pts',(0.000952088007784488,-0.0195793891186717,
-0.00981557170663914));
#35162=CARTESIAN_POINT('Ctrl Pts',(0.00135307241530568,-0.0195490416820845,
-0.0100736651315779));
#35163=CARTESIAN_POINT('Ctrl Pts',(0.00150260117989429,-0.0195377249959086,
-0.0101699092504406));
#35164=CARTESIAN_POINT('Ctrl Pts',(0.00164165715754688,-0.0195264083097328,
-0.010282076734405));
#35165=CARTESIAN_POINT('Ctrl Pts',(0.00176706230547633,-0.0195150916235569,
-0.0104073819668685));
#35166=CARTESIAN_POINT('Ctrl Pts',(0.00210966791500204,-0.0194841745501424,
-0.010749714608341));
#35167=CARTESIAN_POINT('Ctrl Pts',(0.00235053970574287,-0.019453257476728,
-0.0111954394640646));
#35168=CARTESIAN_POINT('Ctrl Pts',(0.00244859695247532,-0.0194223404033135,
-0.011671499279606));
#35169=CARTESIAN_POINT('Ctrl Pts',(0.00248268252246114,-0.0194115933539649,
-0.0118369819002261));
#35170=CARTESIAN_POINT('Ctrl Pts',(0.00249992271098996,-0.0194008463046161,
-0.0120059004115422));
#35171=CARTESIAN_POINT('Ctrl Pts',(0.00249999973973945,-0.0193900992552675,
-0.012174712540005));
#35172=CARTESIAN_POINT('',(0.00249999952946043,-0.0183901705276876,-0.012176929269498));
#35173=CARTESIAN_POINT('Ctrl Pts',(0.00249999999999582,-0.0193900272529644,
-0.0121758487174173));
#35174=CARTESIAN_POINT('Ctrl Pts',(0.00250000088756219,-0.0193592099655948,
-0.012661479609892));
#35175=CARTESIAN_POINT('Ctrl Pts',(0.00235421483873487,-0.0193283761000651,
-0.0131470874883483));
#35176=CARTESIAN_POINT('Ctrl Pts',(0.0020869581343954,-0.0192975252233586,
-0.0135523000691403));
#35177=CARTESIAN_POINT('Ctrl Pts',(0.001994005391597,-0.0192867951890469,
-0.0136932343102256));
#35178=CARTESIAN_POINT('Ctrl Pts',(0.00188680774892241,-0.0192760630969427,
-0.0138245894057865));
#35179=CARTESIAN_POINT('Ctrl Pts',(0.00176769300135974,-0.0192653289288279,
-0.0139436941880376));
#35180=CARTESIAN_POINT('Ctrl Pts',(0.00143152114808729,-0.0192350343997095,
-0.0142798379166879));
#35181=CARTESIAN_POINT('Ctrl Pts',(0.000995098492753798,-0.019204723334944,
-0.0145183453699338));
#35182=CARTESIAN_POINT('Ctrl Pts',(0.000528936678592756,-0.0191743969631418,
-0.0146192578764775));
#35183=CARTESIAN_POINT('Ctrl Pts',(0.000355014062610838,-0.0191630823471504,
-0.0146569078224624));
#35184=CARTESIAN_POINT('Ctrl Pts',(0.000177216695672668,-0.0191517656004221,
-0.0146758695670535));
#35185=CARTESIAN_POINT('Ctrl Pts',(-2.29520690578055E-7,-0.0191404467867643,
-0.0146758532760222));
#35186=CARTESIAN_POINT('Ctrl Pts',(-0.000477621111070754,-0.0191099952698817,
-0.014675809447523));
#35187=CARTESIAN_POINT('Ctrl Pts',(-0.000956528405034772,-0.0190795287926513,
-0.0145347058285624));
#35188=CARTESIAN_POINT('Ctrl Pts',(-0.00135838029685896,-0.0190490427992403,
-0.0142746155334802));
#35189=CARTESIAN_POINT('Ctrl Pts',(-0.00150624544658671,-0.0190378251937692,
-0.0141789128847991));
#35190=CARTESIAN_POINT('Ctrl Pts',(-0.00164381976427042,-0.0190266049459231,
-0.0140676026162161));
#35191=CARTESIAN_POINT('Ctrl Pts',(-0.00176801757635966,-0.0190153818287327,
-0.0139433695805943));
#35192=CARTESIAN_POINT('Ctrl Pts',(-0.00210531564910551,-0.0189849019375425,
-0.0136059758473093));
#35193=CARTESIAN_POINT('Ctrl Pts',(-0.00234407137079544,-0.018954400883096,
-0.0131678879829634));
#35194=CARTESIAN_POINT('Ctrl Pts',(-0.00244439518612312,-0.0189238956125108,
-0.012700193037157));
#35195=CARTESIAN_POINT('Ctrl Pts',(-0.00248140519030315,-0.0189126420513481,
-0.0125276578136636));
#35196=CARTESIAN_POINT('Ctrl Pts',(-0.00250003369489785,-0.0189013879164058,
-0.0123513493333056));
#35197=CARTESIAN_POINT('Ctrl Pts',(-0.00249999995404654,-0.0188901340585108,
-0.0121753739460773));
#35198=CARTESIAN_POINT('Ctrl Pts',(-0.00249990839921447,-0.0188595970379636,
-0.0116978697812211));
#35199=CARTESIAN_POINT('Ctrl Pts',(-0.00235869288269855,-0.0188290620572946,
-0.0112188869879149));
#35200=CARTESIAN_POINT('Ctrl Pts',(-0.00209846725181672,-0.0187985416747736,
-0.0108170173166733));
#35201=CARTESIAN_POINT('Ctrl Pts',(-0.00200282958386128,-0.0187873248772602,
-0.0106693228791603));
#35202=CARTESIAN_POINT('Ctrl Pts',(-0.00189161856248915,-0.0187761100515137,
-0.0105319019889743));
#35203=CARTESIAN_POINT('Ctrl Pts',(-0.00176751057099405,-0.0187648978209337,
-0.0104078299887975));
#35204=CARTESIAN_POINT('Ctrl Pts',(-0.00142992556062184,-0.0187343995352791,
-0.0100703428780802));
#35205=CARTESIAN_POINT('Ctrl Pts',(-0.000991551759118442,-0.0187039204509871,
-0.009831520411939));
#35206=CARTESIAN_POINT('Ctrl Pts',(-0.000523550509890121,-0.0186734572019689,
-0.00973128893608708));
#35207=CARTESIAN_POINT('Ctrl Pts',(-0.00035134857821876,-0.018662248192731,
-0.00969440857778797));
#35208=CARTESIAN_POINT('Ctrl Pts',(-0.000175390128030396,-0.0186510413274082,
-0.00967583603259462));
#35209=CARTESIAN_POINT('Ctrl Pts',(2.45764735002735E-7,-0.0186398364383139,
-0.00967585329863816));
#35210=CARTESIAN_POINT('Ctrl Pts',(0.000475846715698093,-0.0186094949413409,
-0.00967590005301506));
#35211=CARTESIAN_POINT('Ctrl Pts',(0.000953114529689402,-0.01857916793529,
-0.00981598683912423));
#35212=CARTESIAN_POINT('Ctrl Pts',(0.00135398369347432,-0.0185488563282234,
-0.0100742519547624));
#35213=CARTESIAN_POINT('Ctrl Pts',(0.0015034823299754,-0.0185375520316199,
-0.0101705683745117));
#35214=CARTESIAN_POINT('Ctrl Pts',(0.00164249968130742,-0.0185262498767293,
-0.0102828061312865));
#35215=CARTESIAN_POINT('Ctrl Pts',(0.0017678581511007,-0.0185149499106513,
-0.0104081775364312));
#35216=CARTESIAN_POINT('Ctrl Pts',(0.00211031317621986,-0.018484080595052,
-0.0107506678984214));
#35217=CARTESIAN_POINT('Ctrl Pts',(0.00235098525044874,-0.0184532276140454,
-0.0111965061642443));
#35218=CARTESIAN_POINT('Ctrl Pts',(0.00244882647930589,-0.0184223906475597,
-0.0116726148994588));
#35219=CARTESIAN_POINT('Ctrl Pts',(0.00248283735956045,-0.0184116713180213,
-0.0118381164714512));
#35220=CARTESIAN_POINT('Ctrl Pts',(0.00250000059660287,-0.0184009539235939,
-0.0120070464132494));
#35221=CARTESIAN_POINT('Ctrl Pts',(0.00249999999998439,-0.0183902384508335,
-0.0121758621219101));
#35222=CARTESIAN_POINT('',(0.00249999959063015,-0.0173900991833072,-0.0121744179063317));
#35223=CARTESIAN_POINT('Ctrl Pts',(0.00249999903573504,-0.0183900992552675,
-0.0121780490378796));
#35224=CARTESIAN_POINT('Ctrl Pts',(0.00249957249695903,-0.0183591752383259,
-0.0126636898835828));
#35225=CARTESIAN_POINT('Ctrl Pts',(0.00235335328054027,-0.0183282512213843,
-0.0131491781125948));
#35226=CARTESIAN_POINT('Ctrl Pts',(0.00208572997424369,-0.0182973272044428,
-0.0135541603911402));
#35227=CARTESIAN_POINT('Ctrl Pts',(0.00199276069915751,-0.0182865845547177,
-0.0136948466018448));
#35228=CARTESIAN_POINT('Ctrl Pts',(0.00188558847493998,-0.0182758419049926,
-0.0138259636437154));
#35229=CARTESIAN_POINT('Ctrl Pts',(0.0017665348429219,-0.0182650992552675,
-0.0139448514914026));
#35230=CARTESIAN_POINT('Ctrl Pts',(0.00143013698981292,-0.0182347448322822,
-0.0142807809044306));
#35231=CARTESIAN_POINT('Ctrl Pts',(0.000993550900972938,-0.0182043904092969,
-0.0145190032078329));
#35232=CARTESIAN_POINT('Ctrl Pts',(0.00052731742539814,-0.0181740359863115,
-0.0146196078431516));
#35233=CARTESIAN_POINT('Ctrl Pts',(0.00035356526115382,-0.0181627237426302,
-0.0146571003743305));
#35234=CARTESIAN_POINT('Ctrl Pts',(0.000175959535775875,-0.0181514114989488,
-0.0146759442704757));
#35235=CARTESIAN_POINT('Ctrl Pts',(-1.28796846103748E-6,-0.0181400992552675,
-0.0146758529547855));
#35236=CARTESIAN_POINT('Ctrl Pts',(-0.000478659398081885,-0.0181096325812141,
-0.0146756070190147));
#35237=CARTESIAN_POINT('Ctrl Pts',(-0.000957487877102955,-0.0180791659071606,
-0.0145343122044584));
#35238=CARTESIAN_POINT('Ctrl Pts',(-0.00135921802140773,-0.0180486992331071,
-0.0142740730963684));
#35239=CARTESIAN_POINT('Ctrl Pts',(-0.0015068998668508,-0.0180374992404939,
-0.0141784054142588));
#35240=CARTESIAN_POINT('Ctrl Pts',(-0.00164430467893622,-0.0180262992478808,
-0.0140671651195189));
#35241=CARTESIAN_POINT('Ctrl Pts',(-0.0017683566360559,-0.0180150992552675,
-0.0139430303596657));
#35242=CARTESIAN_POINT('Ctrl Pts',(-0.0021057443084893,-0.0179846383135236,
-0.0136054174862585));
#35243=CARTESIAN_POINT('Ctrl Pts',(-0.00234446976288325,-0.0179541773717796,
-0.0131670539246621));
#35244=CARTESIAN_POINT('Ctrl Pts',(-0.00244463034509106,-0.0179237164300356,
-0.0126990955591814));
#35245=CARTESIAN_POINT('Ctrl Pts',(-0.00248147661011304,-0.0179125107051129,
-0.0125269468198901));
#35246=CARTESIAN_POINT('Ctrl Pts',(-0.00250002667142186,-0.0179013049801901,
-0.0123510474891866));
#35247=CARTESIAN_POINT('Ctrl Pts',(-0.00249999997109181,-0.0178900992552675,
-0.0121754731011273));
#35248=CARTESIAN_POINT('Ctrl Pts',(-0.00249992739058463,-0.0178596383135234,
-0.0116982026662986));
#35249=CARTESIAN_POINT('Ctrl Pts',(-0.00235886399483292,-0.0178291773717794,
-0.0112194068467278));
#35250=CARTESIAN_POINT('Ctrl Pts',(-0.0020988613435106,-0.0177987164300353,
-0.0108176261108924));
#35251=CARTESIAN_POINT('Ctrl Pts',(-0.0020032136706863,-0.0177875107051127,
-0.0106698222628437));
#35252=CARTESIAN_POINT('Ctrl Pts',(-0.00189197228786045,-0.01777630498019,
-0.0105322989909189));
#35253=CARTESIAN_POINT('Ctrl Pts',(-0.00176781907028875,-0.0177650992552675,
-0.0104081384524507));
#35254=CARTESIAN_POINT('Ctrl Pts',(-0.00143026521825581,-0.0177346325812141,
-0.0100705646960056));
#35255=CARTESIAN_POINT('Ctrl Pts',(-0.000991893967360312,-0.0177041659071607,
-0.00983165814577795));
#35256=CARTESIAN_POINT('Ctrl Pts',(-0.000523872223124607,-0.0176736992331073,
-0.00973135785930967));
#35257=CARTESIAN_POINT('Ctrl Pts',(-0.0003518206211315,-0.0176624992404941,
-0.00969448601482857));
#35258=CARTESIAN_POINT('Ctrl Pts',(-0.000176016299390968,-0.0176512992478808,
-0.00967589037720141));
#35259=CARTESIAN_POINT('Ctrl Pts',(-5.27597649642248E-7,-0.0176400992552675,
-0.00967585334222996));
#35260=CARTESIAN_POINT('Ctrl Pts',(0.000475085062621117,-0.0176097448322822,
-0.00967575296937904));
#35261=CARTESIAN_POINT('Ctrl Pts',(0.000952405251914807,-0.0175793904092968,
-0.00981569870440331));
#35262=CARTESIAN_POINT('Ctrl Pts',(0.00135335865844833,-0.0175490359863114,
-0.0100738493994059));
#35263=CARTESIAN_POINT('Ctrl Pts',(0.00150278276846154,-0.0175377237426301,
-0.0101700549365618));
#35264=CARTESIAN_POINT('Ctrl Pts',(0.00164174481919509,-0.0175264114989488,
-0.0102821628401217));
#35265=CARTESIAN_POINT('Ctrl Pts',(0.00176707279908354,-0.0175150992552675,
-0.0104073924521772));
#35266=CARTESIAN_POINT('Ctrl Pts',(0.00210967897717657,-0.017484175238326,
-0.0107497297244178));
#35267=CARTESIAN_POINT('Ctrl Pts',(0.00235054853018672,-0.0174532512213847,
-0.0111954593727511));
#35268=CARTESIAN_POINT('Ctrl Pts',(0.0024486017532444,-0.0174223272044432,
-0.0116715225875039));
#35269=CARTESIAN_POINT('Ctrl Pts',(0.00248266432123916,-0.017411584554718,
-0.0118369015023081));
#35270=CARTESIAN_POINT('Ctrl Pts',(0.00249990272492457,-0.0174008419049927,
-0.0120057117944032));
#35271=CARTESIAN_POINT('Ctrl Pts',(0.00249999958793644,-0.0173900992552675,
-0.0121744179058976));
#35272=CARTESIAN_POINT('',(0.00249381958246776,-0.0173787744554382,-0.0123515850776938));
#35273=CARTESIAN_POINT('Origin',(-1.04514259548572E-5,-0.0173843902893253,
-0.0121754854583606));
#35274=CARTESIAN_POINT('',(-0.0005656487160527,-0.0173787743898723,-0.00974068562702664));
#35275=CARTESIAN_POINT('Origin',(0.,-0.0173787743898623,-0.0121758532865581));
#35276=CARTESIAN_POINT('',(0.00249999999193524,-0.0180924405687266,-0.0121757107249461));
#35277=CARTESIAN_POINT('Ctrl Pts',(-0.000565648716059983,-0.0173787743898623,
-0.00974068562702833));
#35278=CARTESIAN_POINT('Ctrl Pts',(-0.00102063502873678,-0.0174085101231125,
-0.00984637133724353));
#35279=CARTESIAN_POINT('Ctrl Pts',(-0.00144474304188495,-0.0174382458563627,
-0.0100828662127555));
#35280=CARTESIAN_POINT('Ctrl Pts',(-0.00177369170692559,-0.0174679815896129,
-0.0104140310115305));
#35281=CARTESIAN_POINT('Ctrl Pts',(-0.00210264037196623,-0.017497717322863,
-0.0107451958103055));
#35282=CARTESIAN_POINT('Ctrl Pts',(-0.00233633893814873,-0.0175274530561132,
-0.0111711335748698));
#35283=CARTESIAN_POINT('Ctrl Pts',(-0.00243891071790016,-0.0175571887893634,
-0.0116265678324346));
#35284=CARTESIAN_POINT('Ctrl Pts',(-0.0025414824976516,-0.0175869245226136,
-0.0120820020899993));
#35285=CARTESIAN_POINT('Ctrl Pts',(-0.00251296309993666,-0.0176166602558637,
-0.0125669427677188));
#35286=CARTESIAN_POINT('Ctrl Pts',(-0.00235772085899037,-0.0176463959891139,
-0.0130072090173266));
#35287=CARTESIAN_POINT('Ctrl Pts',(-0.00220247861804409,-0.0176761317223641,
-0.0134474752669345));
#35288=CARTESIAN_POINT('Ctrl Pts',(-0.00192051160882463,-0.0177058674556142,
-0.0138430567057876));
#35289=CARTESIAN_POINT('Ctrl Pts',(-0.00155496962887267,-0.0177356031888644,
-0.0141334205148503));
#35290=CARTESIAN_POINT('Ctrl Pts',(-0.00118942764892072,-0.0177653389221146,
-0.014423784323913));
#35291=CARTESIAN_POINT('Ctrl Pts',(-0.000740306567027435,-0.0177950746553647,
-0.0146089337847607));
#35292=CARTESIAN_POINT('Ctrl Pts',(-0.000276332539189543,-0.0178248103886149,
-0.0146605344185718));
#35293=CARTESIAN_POINT('Ctrl Pts',(0.000187641488648348,-0.0178545461218651,
-0.014712135052383));
#35294=CARTESIAN_POINT('Ctrl Pts',(0.000666458784610825,-0.0178842818551152,
-0.014630191083476));
#35295=CARTESIAN_POINT('Ctrl Pts',(0.00108687388580177,-0.0179140175883654,
-0.0144272317879128));
#35296=CARTESIAN_POINT('Ctrl Pts',(0.00150728898699271,-0.0179437533216156,
-0.0142242724923496));
#35297=CARTESIAN_POINT('Ctrl Pts',(0.00186930350615625,-0.0179734890548657,
-0.013900260938493));
#35298=CARTESIAN_POINT('Ctrl Pts',(0.00211745136178973,-0.0180032247881159,
-0.0135049130032205));
#35299=CARTESIAN_POINT('Ctrl Pts',(0.00236559817464578,-0.0180329603964093,
-0.0131095667292959));
#35300=CARTESIAN_POINT('Ctrl Pts',(0.00250000021304311,-0.0180626960047028,
-0.0126429497555809));
#35301=CARTESIAN_POINT('Ctrl Pts',(0.00249999999999974,-0.0180924316129961,
-0.0121758521463073));
#35302=CARTESIAN_POINT('',(0.00249999972323816,-0.0190923959387205,-0.0121750282773563));
#35303=CARTESIAN_POINT('Ctrl Pts',(0.00249999998387073,-0.0180924495244571,
-0.012175569303585));
#35304=CARTESIAN_POINT('Ctrl Pts',(0.00249994481879298,-0.0181233634206488,
-0.0116899321120859));
#35305=CARTESIAN_POINT('Ctrl Pts',(0.00235409908043358,-0.0181542773168405,
-0.0112043354005097));
#35306=CARTESIAN_POINT('Ctrl Pts',(0.00208678918439825,-0.0181851912130322,
-0.0107991503774748));
#35307=CARTESIAN_POINT('Ctrl Pts',(0.00199384948267087,-0.0181959395180291,
-0.0106582735309988));
#35308=CARTESIAN_POINT('Ctrl Pts',(0.00188667534136289,-0.018206687823026,
-0.0105269712305407));
#35309=CARTESIAN_POINT('Ctrl Pts',(0.00176759243584567,-0.018217436128023,
-0.010407911833698));
#35310=CARTESIAN_POINT('Ctrl Pts',(0.00143140152045128,-0.0182477803867574,
-0.0100717872872149));
#35311=CARTESIAN_POINT('Ctrl Pts',(0.000994966013488791,-0.0182781246454917,
-0.0098333052659455));
#35312=CARTESIAN_POINT('Ctrl Pts',(0.00052880017530072,-0.0183084689042261,
-0.00973241915104269));
#35313=CARTESIAN_POINT('Ctrl Pts',(0.00035492747743972,-0.0183197868466803,
-0.00969479017968124));
#35314=CARTESIAN_POINT('Ctrl Pts',(0.000177183507666847,-0.0183311047891346,
-0.00967583842259123));
#35315=CARTESIAN_POINT('Ctrl Pts',(-2.0960162221961E-7,-0.0183424227315888,
-0.00967585329534467));
#35316=CARTESIAN_POINT('Ctrl Pts',(-0.00047757315541562,-0.0183728792315804,
-0.00967589331781491));
#35317=CARTESIAN_POINT('Ctrl Pts',(-0.000956456302177873,-0.0184033357315721,
-0.00981697710992422));
#35318=CARTESIAN_POINT('Ctrl Pts',(-0.00135829552168139,-0.0184337922315637,
-0.0100770361730915));
#35319=CARTESIAN_POINT('Ctrl Pts',(-0.00150614212993305,-0.0184449979327607,
-0.0101727183478725));
#35320=CARTESIAN_POINT('Ctrl Pts',(-0.00164370139022194,-0.0184562036339577,
-0.0102840036490499));
#35321=CARTESIAN_POINT('Ctrl Pts',(-0.00176788886171212,-0.0184674093351546,
-0.0104082082507451));
#35322=CARTESIAN_POINT('Ctrl Pts',(-0.00210536041935918,-0.0184978601156729,
-0.0107457263586352));
#35323=CARTESIAN_POINT('Ctrl Pts',(-0.00234420066788555,-0.0185283108961913,
-0.0111840193628629));
#35324=CARTESIAN_POINT('Ctrl Pts',(-0.00244448756983183,-0.0185587616767095,
-0.0116519444004551));
#35325=CARTESIAN_POINT('Ctrl Pts',(-0.00248141137363274,-0.0185699730973799,
-0.0118242258444551));
#35326=CARTESIAN_POINT('Ctrl Pts',(-0.00250000950067293,-0.0185811845180502,
-0.0120002691096592));
#35327=CARTESIAN_POINT('Ctrl Pts',(-0.0024999999963431,-0.0185923959387205,
-0.0121759885068293));
#35328=CARTESIAN_POINT('Ctrl Pts',(-0.00249997418210687,-0.0186228467192388,
-0.0126532511975605));
#35329=CARTESIAN_POINT('Ctrl Pts',(-0.00235896206199205,-0.018653297499757,
-0.0131320547624161));
#35330=CARTESIAN_POINT('Ctrl Pts',(-0.00209900534106159,-0.0186837482802753,
-0.0135338579176971));
#35331=CARTESIAN_POINT('Ctrl Pts',(-0.00200329402907474,-0.0186949597009456,
-0.0136817944935038));
#35332=CARTESIAN_POINT('Ctrl Pts',(-0.00189196193403086,-0.018706171121616,
-0.0138194350006231));
#35333=CARTESIAN_POINT('Ctrl Pts',(-0.00176769763421554,-0.0187173825422863,
-0.0139436895555572));
#35334=CARTESIAN_POINT('Ctrl Pts',(-0.00143012617404289,-0.018747839042278,
-0.0142812345431729));
#35335=CARTESIAN_POINT('Ctrl Pts',(-0.000991746055560251,-0.0187782955422696,
-0.0145201097185846));
#35336=CARTESIAN_POINT('Ctrl Pts',(-0.000523724419950059,-0.0188087520422614,
-0.0146203803843723));
#35337=CARTESIAN_POINT('Ctrl Pts',(-0.000351527660513317,-0.0188199577434583,
-0.0146572724474768));
#35338=CARTESIAN_POINT('Ctrl Pts',(-0.000175573044316863,-0.0188311634446552,
-0.0146758575599681));
#35339=CARTESIAN_POINT('Ctrl Pts',(6.08389199934128E-8,-0.0188423691458522,
-0.0146758532858178));
#35340=CARTESIAN_POINT('Ctrl Pts',(0.00047566516762695,-0.0188727134045866,
-0.0146758417117163));
#35341=CARTESIAN_POINT('Ctrl Pts',(0.000952945835934379,-0.0189030576633209,
-0.0145357883099573));
#35342=CARTESIAN_POINT('Ctrl Pts',(0.0013538351280994,-0.0189334019220553,
-0.0142775503260774));
#35343=CARTESIAN_POINT('Ctrl Pts',(0.00150336067686838,-0.0189447198645095,
-0.0141812315243351));
#35344=CARTESIAN_POINT('Ctrl Pts',(0.00164240318950303,-0.0189560378069638,
-0.0140689863748748));
#35345=CARTESIAN_POINT('Ctrl Pts',(0.00176778367472126,-0.018967355749418,
-0.0139436035176114));
#35346=CARTESIAN_POINT('Ctrl Pts',(0.00211024868725995,-0.0189982696456097,
-0.0136011320260544));
#35347=CARTESIAN_POINT('Ctrl Pts',(0.00235093846666087,-0.0190291835418014,
-0.0131553101000555));
#35348=CARTESIAN_POINT('Ctrl Pts',(0.00244880189405485,-0.0190600974379931,
-0.0126792112940174));
#35349=CARTESIAN_POINT('Ctrl Pts',(0.00248282756196641,-0.01907084574299,
-0.0125136787728425));
#35350=CARTESIAN_POINT('Ctrl Pts',(0.0024999990853136,-0.0190815940479869,
-0.01234471570696));
#35351=CARTESIAN_POINT('Ctrl Pts',(0.00249999999996332,-0.0190923423529838,
-0.0121758668289893));
#35352=CARTESIAN_POINT('',(0.00249999972741721,-0.0200925477005089,-0.0121764841472801));
#35353=CARTESIAN_POINT('Ctrl Pts',(0.00249999944651301,-0.0190924495244571,
-0.0121741897257233));
#35354=CARTESIAN_POINT('Ctrl Pts',(0.00249967628899577,-0.0191233739581301,
-0.0116885485653149));
#35355=CARTESIAN_POINT('Ctrl Pts',(0.00235356029135108,-0.0191542983918031,
-0.0112030290255191));
#35356=CARTESIAN_POINT('Ctrl Pts',(0.00208602297944995,-0.0191852228254761,
-0.0107979896760339));
#35357=CARTESIAN_POINT('Ctrl Pts',(0.00199308843554419,-0.0191959650584697,
-0.010657290993892));
#35358=CARTESIAN_POINT('Ctrl Pts',(0.00188595038429507,-0.0192067072914634,
-0.0105261574625068));
#35359=CARTESIAN_POINT('Ctrl Pts',(0.00176692942331025,-0.0192174495244571,
-0.0104072492005511));
#35360=CARTESIAN_POINT('Ctrl Pts',(0.00143060615072211,-0.0192478043705736,
-0.0100712443870478));
#35361=CARTESIAN_POINT('Ctrl Pts',(0.000994072722768003,-0.0192781592166902,
-0.00983292461567489));
#35362=CARTESIAN_POINT('Ctrl Pts',(0.000527861249261944,-0.0193085140628067,
-0.00973221614051378));
#35363=CARTESIAN_POINT('Ctrl Pts',(0.000354126205227666,-0.0193198258833568,
-0.00969468683812412));
#35364=CARTESIAN_POINT('Ctrl Pts',(0.000176533840600821,-0.019331137703907,
-0.00967580342092681));
#35365=CARTESIAN_POINT('Ctrl Pts',(-7.04769819689285E-7,-0.0193424495244571,
-0.0096758533858982));
#35366=CARTESIAN_POINT('Ctrl Pts',(-0.000478076729573463,-0.0193729166215054,
-0.00967598796084355));
#35367=CARTESIAN_POINT('Ctrl Pts',(-0.000956938538252152,-0.0194033837185538,
-0.00981717134421778));
#35368=CARTESIAN_POINT('Ctrl Pts',(-0.00135872957220158,-0.0194338508156022,
-0.0100773171420934));
#35369=CARTESIAN_POINT('Ctrl Pts',(-0.00150642617255667,-0.0194450503852205,
-0.0101729455824924));
#35370=CARTESIAN_POINT('Ctrl Pts',(-0.00164385041494005,-0.0194562499548387,
-0.0102841474371042));
#35371=CARTESIAN_POINT('Ctrl Pts',(-0.00176792630945377,-0.0194674495244571,
-0.0104082457044457));
#35372=CARTESIAN_POINT('Ctrl Pts',(-0.00210539650822995,-0.0194979108884482,
-0.0107457767543861));
#35373=CARTESIAN_POINT('Ctrl Pts',(-0.00234422876329441,-0.0195283722524392,
-0.0111840826282489));
#35374=CARTESIAN_POINT('Ctrl Pts',(-0.00244450313034634,-0.0195588336164303,
-0.0116520170089608));
#35375=CARTESIAN_POINT('Ctrl Pts',(-0.00248138935230773,-0.0195700389191059,
-0.0118241480523946));
#35376=CARTESIAN_POINT('Ctrl Pts',(-0.00249998214814256,-0.0195812442217815,
-0.0120000337511903));
#35377=CARTESIAN_POINT('Ctrl Pts',(-0.00249999998709464,-0.0195924495244571,
-0.012175599265259));
#35378=CARTESIAN_POINT('Ctrl Pts',(-0.00250004848188573,-0.0196229108884482,
-0.0126528701773575));
#35379=CARTESIAN_POINT('Ctrl Pts',(-0.0023591062861405,-0.0196533722524392,
-0.0131317021386709));
#35380=CARTESIAN_POINT('Ctrl Pts',(-0.00209920516654239,-0.0196838336164303,
-0.0135335490067995));
#35381=CARTESIAN_POINT('Ctrl Pts',(-0.0020035997723886,-0.0196950389191059,
-0.0136813695636186));
#35382=CARTESIAN_POINT('Ctrl Pts',(-0.00189239965550865,-0.0197062442217815,
-0.0138189145415262));
#35383=CARTESIAN_POINT('Ctrl Pts',(-0.00176828548092616,-0.0197174495244571,
-0.0139431015594235));
#35384=CARTESIAN_POINT('Ctrl Pts',(-0.00143082037966594,-0.0197479166215054,
-0.0142807647208706));
#35385=CARTESIAN_POINT('Ctrl Pts',(-0.000992511726133087,-0.0197783837185537,
-0.0145197870193782));
#35386=CARTESIAN_POINT('Ctrl Pts',(-0.000524516037558449,-0.0198088508156021,
-0.0146202106512542));
#35387=CARTESIAN_POINT('Ctrl Pts',(-0.000352482900073631,-0.0198200503852204,
-0.0146571259325079));
#35388=CARTESIAN_POINT('Ctrl Pts',(-0.000176692611848837,-0.0198312499548388,
-0.014675767862736));
#35389=CARTESIAN_POINT('Ctrl Pts',(-1.21281238046647E-6,-0.0198424495244571,
-0.0146758529923753));
#35390=CARTESIAN_POINT('Ctrl Pts',(0.000474400313029194,-0.0198728043705736,
-0.0146760837241972));
#35391=CARTESIAN_POINT('Ctrl Pts',(0.000951759243660809,-0.0199031592166902,
-0.0145362685350562));
#35392=CARTESIAN_POINT('Ctrl Pts',(0.00135278359530711,-0.0199335140628067,
-0.0142782273123366));
#35393=CARTESIAN_POINT('Ctrl Pts',(0.00150222647123657,-0.0199448258833568,
-0.0141820675098875));
#35394=CARTESIAN_POINT('Ctrl Pts',(0.00164121270041218,-0.019956137703907,
-0.0140700040924385));
#35395=CARTESIAN_POINT('Ctrl Pts',(0.00176656997634155,-0.0199674495244571,
-0.01394481640621));
#35396=CARTESIAN_POINT('Ctrl Pts',(0.00210927367710781,-0.0199983739581303,
-0.0136025763324464));
#35397=CARTESIAN_POINT('Ctrl Pts',(0.00235026996938759,-0.0200292983918035,
-0.0131569149011769));
#35398=CARTESIAN_POINT('Ctrl Pts',(0.00244845842858246,-0.0200602228254768,
-0.0126808793487603));
#35399=CARTESIAN_POINT('Ctrl Pts',(0.00248256619324154,-0.0200709650584702,
-0.0125155186869849));
#35400=CARTESIAN_POINT('Ctrl Pts',(0.00249985251929391,-0.0200817072914636,
-0.0123467222292437));
#35401=CARTESIAN_POINT('Ctrl Pts',(0.00249999905682766,-0.0200924495244571,
-0.0121780248898416));
#35402=CARTESIAN_POINT('',(0.00249999999999813,-0.0210924016317463,-0.0121758502265542));
#35403=CARTESIAN_POINT('Ctrl Pts',(0.00249999999999579,-0.0200925876067202,
-0.0121758578723672));
#35404=CARTESIAN_POINT('Ctrl Pts',(0.00250000088291571,-0.0201232524092462,
-0.0116945251893599));
#35405=CARTESIAN_POINT('Ctrl Pts',(0.00235859969628574,-0.0201525642010006,
-0.0112380345259211));
#35406=CARTESIAN_POINT('Ctrl Pts',(0.00209855644319116,-0.0201841557313721,
-0.0108159596537342));
#35407=CARTESIAN_POINT('Ctrl Pts',(0.00206718492720256,-0.0201877656541674,
-0.0107687593266094));
#35408=CARTESIAN_POINT('Ctrl Pts',(0.00175006943670304,-0.0202225469736906,
-0.0103247030656945));
#35409=CARTESIAN_POINT('Ctrl Pts',(0.0013651500455325,-0.0202520137354763,
-0.010036664202749));
#35410=CARTESIAN_POINT('Ctrl Pts',(0.000561164206619752,-0.0203074924422943,
-0.00970100797496499));
#35411=CARTESIAN_POINT('Ctrl Pts',(0.000143409931365646,-0.0203335043873267,
-0.00965099224594665));
#35412=CARTESIAN_POINT('Ctrl Pts',(-0.000616036517871959,-0.0203820729533282,
-0.00972310203715264));
#35413=CARTESIAN_POINT('Ctrl Pts',(-0.000957753383009871,-0.0204046295742975,
-0.0098435059109142));
#35414=CARTESIAN_POINT('Ctrl Pts',(-0.0015259109359658,-0.0204462893830545,
-0.0101686832292785));
#35415=CARTESIAN_POINT('Ctrl Pts',(-0.00175283236942671,-0.0204653925708423,
-0.0103724766563074));
#35416=CARTESIAN_POINT('Ctrl Pts',(-0.00210085664408624,-0.0205001384570194,
-0.0107934676866464));
#35417=CARTESIAN_POINT('Ctrl Pts',(-0.00222243362220393,-0.0205157811554087,
-0.0110101717401975));
#35418=CARTESIAN_POINT('Ctrl Pts',(-0.00234911679547337,-0.0205366695864338,
-0.0113134981106694));
#35419=CARTESIAN_POINT('Ctrl Pts',(-0.00238204707436731,-0.0205432031273489,
-0.0114109864453164));
#35420=CARTESIAN_POINT('Ctrl Pts',(-0.00243357549085177,-0.0205553781071763,
-0.0115954397446258));
#35421=CARTESIAN_POINT('Ctrl Pts',(-0.0024522147205405,-0.0205610195460884,
-0.011682387300099));
#35422=CARTESIAN_POINT('Ctrl Pts',(-0.00247950787235856,-0.020571546984231,
-0.0118458435498237));
#35423=CARTESIAN_POINT('Ctrl Pts',(-0.00248801985791747,-0.0205764329834614,
-0.0119223870026145));
#35424=CARTESIAN_POINT('Ctrl Pts',(-0.00249552276806611,-0.0205828105879445,
-0.0120225949860141));
#35425=CARTESIAN_POINT('Ctrl Pts',(-0.00249723367102841,-0.0205847778903784,
-0.0120535529673888));
#35426=CARTESIAN_POINT('Ctrl Pts',(-0.00249902446490594,-0.0205879816792375,
-0.012104019675008));
#35427=CARTESIAN_POINT('Ctrl Pts',(-0.00249943337907817,-0.0205890917480586,
-0.0121215172175532));
#35428=CARTESIAN_POINT('Ctrl Pts',(-0.00249981312615746,-0.0205904789322726,
-0.0121433885497522));
#35429=CARTESIAN_POINT('Ctrl Pts',(-0.00249999256379323,-0.0205907560476657,
-0.0121477556401092));
#35430=CARTESIAN_POINT('Ctrl Pts',(-0.00250000725685106,-0.0205942339146019,
-0.012202611695506));
#35431=CARTESIAN_POINT('Ctrl Pts',(-0.00249920257363735,-0.0205974346661451,
-0.0122531107066766));
#35432=CARTESIAN_POINT('Ctrl Pts',(-0.0024948669570304,-0.0206030813157931,
-0.01234204919432));
#35433=CARTESIAN_POINT('Ctrl Pts',(-0.00249192331425481,-0.020605527213898,
-0.0123805224298522));
#35434=CARTESIAN_POINT('Ctrl Pts',(-0.00248031131675541,-0.0206130664403408,
-0.0124988715853413));
#35435=CARTESIAN_POINT('Ctrl Pts',(-0.00246824224566287,-0.020618361300807,
-0.01258158571656));
#35436=CARTESIAN_POINT('Ctrl Pts',(-0.00241993022737028,-0.0206341006264045,
-0.0128249234266664));
#35437=CARTESIAN_POINT('Ctrl Pts',(-0.00237242236421832,-0.0206443998357345,
-0.0129809906837992));
#35438=CARTESIAN_POINT('Ctrl Pts',(-0.00224761580526192,-0.0206651083145812,
-0.0132825859980184));
#35439=CARTESIAN_POINT('Ctrl Pts',(-0.00217004468113035,-0.020675517584098,
-0.0134279412711221));
#35440=CARTESIAN_POINT('Ctrl Pts',(-0.00198816583959298,-0.0206963137002469,
-0.013700325271695));
#35441=CARTESIAN_POINT('Ctrl Pts',(-0.00188391087056668,-0.020706700546879,
-0.0138274099627527));
#35442=CARTESIAN_POINT('Ctrl Pts',(-0.00153699680145617,-0.0207378762373913,
-0.0141745226749268));
#35443=CARTESIAN_POINT('Ctrl Pts',(-0.00125969929053859,-0.0207586802318874,
-0.0143599649981351));
#35444=CARTESIAN_POINT('Ctrl Pts',(-0.000654815182332665,-0.0208003032688987,
-0.0146106845637142));
#35445=CARTESIAN_POINT('Ctrl Pts',(-0.000327493358863664,-0.0208211223114141,
-0.0146757914697553));
#35446=CARTESIAN_POINT('Ctrl Pts',(0.000478376746627,-0.0208724523882349,
-0.0146759436934712));
#35447=CARTESIAN_POINT('Ctrl Pts',(0.000958122796932754,-0.0209029755972295,
-0.0145341502276829));
#35448=CARTESIAN_POINT('Ctrl Pts',(0.0015072169308343,-0.0209446959549672,
-0.0141781084150004));
#35449=CARTESIAN_POINT('Ctrl Pts',(0.00164404399136796,-0.0209558741894894,
-0.0140673205596144));
#35450=CARTESIAN_POINT('Ctrl Pts',(0.00210759434674393,-0.0209978211139755,
-0.0136038550902574));
#35451=CARTESIAN_POINT('Ctrl Pts',(0.00234767621310324,-0.0210286086970427,
-0.0131616003846502));
#35452=CARTESIAN_POINT('Ctrl Pts',(0.00248215348338499,-0.0210704099800494,
-0.0125202443438541));
#35453=CARTESIAN_POINT('Ctrl Pts',(0.00250000021067322,-0.0210814043918721,
-0.012347970180121));
#35454=CARTESIAN_POINT('Ctrl Pts',(0.00249999999999813,-0.0210924016317463,
-0.0121758502265542));
#35455=CARTESIAN_POINT('',(0.0024999998213867,-0.022092406279442,-0.012175193061947));
#35456=CARTESIAN_POINT('Ctrl Pts',(0.00249999988477308,-0.0210924495244571,
-0.0121750942512416));
#35457=CARTESIAN_POINT('Ctrl Pts',(0.00249985243829347,-0.0211233650347228,
-0.0116894565292411));
#35458=CARTESIAN_POINT('Ctrl Pts',(0.00235391411686965,-0.0211542805449884,
-0.0112038870833032));
#35459=CARTESIAN_POINT('Ctrl Pts',(0.00208652671078272,-0.0211851960552541,
-0.0107987526057108));
#35460=CARTESIAN_POINT('Ctrl Pts',(0.00199357142069997,-0.0211959436079039,
-0.0106579105464745));
#35461=CARTESIAN_POINT('Ctrl Pts',(0.00188638697405189,-0.0212066911605536,
-0.0105266434104093));
#35462=CARTESIAN_POINT('Ctrl Pts',(0.00176729866884987,-0.0212174387132034,
-0.0104076181734915));
#35463=CARTESIAN_POINT('Ctrl Pts',(0.0014310510541324,-0.0212477845892019,
-0.0100715486330199));
#35464=CARTESIAN_POINT('Ctrl Pts',(0.000994574777890654,-0.0212781304652003,
-0.00983313893831883));
#35465=CARTESIAN_POINT('Ctrl Pts',(0.00052839112564458,-0.0213084763411988,
-0.00973233066167));
#35466=CARTESIAN_POINT('Ctrl Pts',(0.000354532657022751,-0.0213197935281157,
-0.00969473523652343));
#35467=CARTESIAN_POINT('Ctrl Pts',(0.0001768069587554,-0.0213311107150327,
-0.0096758132432822));
#35468=CARTESIAN_POINT('Ctrl Pts',(-5.65296794099548E-7,-0.0213424279019496,
-0.00967585335047019));
#35469=CARTESIAN_POINT('Ctrl Pts',(-0.000477929976962419,-0.02137288602121,
-0.00967596129156228));
#35470=CARTESIAN_POINT('Ctrl Pts',(-0.000956793938650606,-0.0214033441404702,
-0.00981711385692225));
#35471=CARTESIAN_POINT('Ctrl Pts',(-0.00135859660307426,-0.0214338022597306,
-0.0100772310551608));
#35472=CARTESIAN_POINT('Ctrl Pts',(-0.00150641190896486,-0.0214450072033856,
-0.0101729230617834));
#35473=CARTESIAN_POINT('Ctrl Pts',(-0.0016439400878006,-0.0214562121470408,
-0.0102842129945245));
#35474=CARTESIAN_POINT('Ctrl Pts',(-0.00176809815021911,-0.0214674170906958,
-0.0104084175929071));
#35475=CARTESIAN_POINT('Ctrl Pts',(-0.00210553052273885,-0.0214978694886136,
-0.0107459764392172));
#35476=CARTESIAN_POINT('Ctrl Pts',(-0.00234431904705325,-0.0215283218865315,
-0.0111842987747312));
#35477=CARTESIAN_POINT('Ctrl Pts',(-0.00244455018892782,-0.0215587742844493,
-0.0116522366578946));
#35478=CARTESIAN_POINT('Ctrl Pts',(-0.00248144901564452,-0.0215699849494469,
-0.0118245020690442));
#35479=CARTESIAN_POINT('Ctrl Pts',(-0.00250002608530036,-0.0215811956144444,
-0.0120005262168479));
#35480=CARTESIAN_POINT('Ctrl Pts',(-0.00249999997238889,-0.021592406279442,
-0.0121762248448264));
#35481=CARTESIAN_POINT('Ctrl Pts',(-0.00249992903986427,-0.0216228586773597,
-0.0126534886408611));
#35482=CARTESIAN_POINT('Ctrl Pts',(-0.00235887103208122,-0.0216533110752775,
-0.0131322797429597));
#35483=CARTESIAN_POINT('Ctrl Pts',(-0.00209887538814559,-0.0216837634731953,
-0.0135340587588769));
#35484=CARTESIAN_POINT('Ctrl Pts',(-0.00200316128139836,-0.0216949741381929,
-0.0136819686201198));
#35485=CARTESIAN_POINT('Ctrl Pts',(-0.00189183109921226,-0.0217061848031906,
-0.0138195833748683));
#35486=CARTESIAN_POINT('Ctrl Pts',(-0.00176757270783774,-0.0217173954681882,
-0.0139438144633115));
#35487=CARTESIAN_POINT('Ctrl Pts',(-0.00142997659695858,-0.0217478535874485,
-0.0142813363951889));
#35488=CARTESIAN_POINT('Ctrl Pts',(-0.000991578519381806,-0.0217783117067088,
-0.0145201807728917));
#35489=CARTESIAN_POINT('Ctrl Pts',(-0.000523548797234617,-0.0218087698259691,
-0.0146204180038266));
#35490=CARTESIAN_POINT('Ctrl Pts',(-0.000351369857991001,-0.0218199747696242,
-0.0146572933116937));
#35491=CARTESIAN_POINT('Ctrl Pts',(-0.000175435271197161,-0.0218311797132794,
-0.0146758657712238));
#35492=CARTESIAN_POINT('Ctrl Pts',(1.77819740284356E-7,-0.0218423846569345,
-0.0146758532802341));
#35493=CARTESIAN_POINT('Ctrl Pts',(0.00047578334220584,-0.021872730532933,
-0.0146758194514139));
#35494=CARTESIAN_POINT('Ctrl Pts',(0.000953058397251753,-0.0219030764089314,
-0.0145357430466052));
#35495=CARTESIAN_POINT('Ctrl Pts',(0.00135393608389562,-0.0219334222849299,
-0.0142774852906743));
#35496=CARTESIAN_POINT('Ctrl Pts',(0.00150343935448162,-0.0219447394718468,
-0.0141811706778827));
#35497=CARTESIAN_POINT('Ctrl Pts',(0.00164246131298928,-0.0219560566587638,
-0.0140689339964588));
#35498=CARTESIAN_POINT('Ctrl Pts',(0.00176782419267002,-0.0219673738456807,
-0.0139435629979674));
#35499=CARTESIAN_POINT('Ctrl Pts',(0.00211028185658907,-0.0219982893559464,
-0.0136010831556415));
#35500=CARTESIAN_POINT('Ctrl Pts',(0.00235096149551733,-0.022029204866212,
-0.0131552550642329));
#35501=CARTESIAN_POINT('Ctrl Pts',(0.00244881377882811,-0.0220601203764777,
-0.012679153471956));
#35502=CARTESIAN_POINT('Ctrl Pts',(0.00248283141456312,-0.0220708679291274,
-0.0125136402106303));
#35503=CARTESIAN_POINT('Ctrl Pts',(0.00249999892493164,-0.0220816154817772,
-0.0123446976407022));
#35504=CARTESIAN_POINT('Ctrl Pts',(0.00249999999994932,-0.0220923630344269,
-0.0121758692053469));
#35505=CARTESIAN_POINT('',(0.00249999957091393,-0.0230925272726456,-0.0121768329188578));
#35506=CARTESIAN_POINT('Ctrl Pts',(0.00249999964282408,-0.0220924495244571,
-0.0121745169185471));
#35507=CARTESIAN_POINT('Ctrl Pts',(0.00249974004482518,-0.0221233733501191,
-0.0116888760627414));
#35508=CARTESIAN_POINT('Ctrl Pts',(0.00235368778652483,-0.022154297175781,
-0.0112033376886623));
#35509=CARTESIAN_POINT('Ctrl Pts',(0.00208620381233168,-0.022185221001443,
-0.0107982634878833));
#35510=CARTESIAN_POINT('Ctrl Pts',(0.00199328071033653,-0.0221959638424477,
-0.0106575419684423));
#35511=CARTESIAN_POINT('Ctrl Pts',(0.00188615069187808,-0.0222067066834524,
-0.0105263851913197));
#35512=CARTESIAN_POINT('Ctrl Pts',(0.00176713455698379,-0.0222174495244571,
-0.0104074541637598));
#35513=CARTESIAN_POINT('Ctrl Pts',(0.00143085079516353,-0.0222478037532254,
-0.0100714108753393));
#35514=CARTESIAN_POINT('Ctrl Pts',(0.000994345731519502,-0.0222781579819937,
-0.00983304058934352));
#35515=CARTESIAN_POINT('Ctrl Pts',(0.000528146602411794,-0.022308512210762,
-0.00973227779839309));
#35516=CARTESIAN_POINT('Ctrl Pts',(0.000354403143582682,-0.0223198246486604,
-0.00969472544205448));
#35517=CARTESIAN_POINT('Ctrl Pts',(0.000176799616673616,-0.0223311370865588,
-0.00967582128046176));
#35518=CARTESIAN_POINT('Ctrl Pts',(-4.51998086409324E-7,-0.0223424495244571,
-0.00967585332741856));
#35519=CARTESIAN_POINT('Ctrl Pts',(-0.000477823260289689,-0.022372916004356,
-0.00967593963577877));
#35520=CARTESIAN_POINT('Ctrl Pts',(-0.000956698784724591,-0.0224033824842549,
-0.00981707420232769));
#35521=CARTESIAN_POINT('Ctrl Pts',(-0.00135851583923652,-0.0224338489641538,
-0.0100771787728368));
#35522=CARTESIAN_POINT('Ctrl Pts',(-0.00150623313614594,-0.0224450491509216,
-0.0101727992638984));
#35523=CARTESIAN_POINT('Ctrl Pts',(-0.00164367812918537,-0.0224562493376893,
-0.0102839965356232));
#35524=CARTESIAN_POINT('Ctrl Pts',(-0.00176777389185949,-0.0224674495244571,
-0.0104080932725121));
#35525=CARTESIAN_POINT('Ctrl Pts',(-0.00210527270547203,-0.02249791027239,
-0.0107455947356616));
#35526=CARTESIAN_POINT('Ctrl Pts',(-0.00234414264356883,-0.022528371020323,
-0.0111838793575966));
#35527=CARTESIAN_POINT('Ctrl Pts',(-0.00244445757818406,-0.0225588317682559,
-0.0116518044830498));
#35528=CARTESIAN_POINT('Ctrl Pts',(-0.00248136149819129,-0.0225700376869897,
-0.0118239450667558));
#35529=CARTESIAN_POINT('Ctrl Pts',(-0.00249996959653367,-0.0225812436057234,
-0.0119998424534536));
#35530=CARTESIAN_POINT('Ctrl Pts',(-0.00249999996261091,-0.0225924495244571,
-0.0121754209146634));
#35531=CARTESIAN_POINT('Ctrl Pts',(-0.0025000825059031,-0.0226229102723899,
-0.0126526911302003));
#35532=CARTESIAN_POINT('Ctrl Pts',(-0.00235917485964853,-0.0226533710203227,
-0.0131315326026438));
#35533=CARTESIAN_POINT('Ctrl Pts',(-0.00209930299428055,-0.0226838317682555,
-0.0135333977382077));
#35534=CARTESIAN_POINT('Ctrl Pts',(-0.00200370117219264,-0.0226950376869894,
-0.013681236132099));
#35535=CARTESIAN_POINT('Ctrl Pts',(-0.0018925015674253,-0.0227062436057232,
-0.013818798540917));
#35536=CARTESIAN_POINT('Ctrl Pts',(-0.00176838524989491,-0.0227174495244571,
-0.0139430017262638));
#35537=CARTESIAN_POINT('Ctrl Pts',(-0.00143093971035745,-0.022747916004356,
-0.0142806834406874));
#35538=CARTESIAN_POINT('Ctrl Pts',(-0.000992645225224244,-0.0227783824842549,
-0.0145197303711406));
#35539=CARTESIAN_POINT('Ctrl Pts',(-0.000524655831827541,-0.0228088489641538,
-0.0146201806496847));
#35540=CARTESIAN_POINT('Ctrl Pts',(-0.000352612043744256,-0.0228200491509216,
-0.0146571085089024));
#35541=CARTESIAN_POINT('Ctrl Pts',(-0.000176809501660097,-0.0228312493376894,
-0.0146757605083209));
#35542=CARTESIAN_POINT('Ctrl Pts',(-1.31674182171623E-6,-0.0228424495244571,
-0.0146758529397963));
#35543=CARTESIAN_POINT('Ctrl Pts',(0.000474295628738454,-0.0228728037532255,
-0.0146761034433107));
#35544=CARTESIAN_POINT('Ctrl Pts',(0.000951659784619451,-0.0229031579819938,
-0.0145363085163652));
#35545=CARTESIAN_POINT('Ctrl Pts',(0.00135269456445851,-0.0229335122107622,
-0.0142782845970376));
#35546=CARTESIAN_POINT('Ctrl Pts',(0.00150215252224747,-0.0229448246486605,
-0.0141821240394448));
#35547=CARTESIAN_POINT('Ctrl Pts',(0.00164115295742169,-0.0229561370865589,
-0.0140700570709453));
#35548=CARTESIAN_POINT('Ctrl Pts',(0.00176652276641499,-0.0229674495244571,
-0.0139448635510104));
#35549=CARTESIAN_POINT('Ctrl Pts',(0.00210923528792769,-0.022998373350119,
-0.0136026329355339));
#35550=CARTESIAN_POINT('Ctrl Pts',(0.00235024342465923,-0.023029297175781,
-0.013156978340393));
#35551=CARTESIAN_POINT('Ctrl Pts',(0.00244844473207978,-0.0230602210014429,
-0.0126809457473519));
#35552=CARTESIAN_POINT('Ctrl Pts',(0.00248255956132539,-0.0230709638424477,
-0.0125155735027911));
#35553=CARTESIAN_POINT('Ctrl Pts',(0.00249985049107578,-0.0230817066834523,
-0.0123467644820629));
#35554=CARTESIAN_POINT('Ctrl Pts',(0.00249999903102137,-0.0230924495244571,
-0.0121780543981421));
#35555=CARTESIAN_POINT('',(0.00250015411382638,-0.02409267137066,-0.0121754468914277));
#35556=CARTESIAN_POINT('Ctrl Pts',(0.00249999999998422,-0.0230925890616768,
-0.0121758621692742));
#35557=CARTESIAN_POINT('Ctrl Pts',(0.00250000171777091,-0.0231233655601217,
-0.0116923989266971));
#35558=CARTESIAN_POINT('Ctrl Pts',(0.00235737737085954,-0.0231527215417898,
-0.0112349651717997));
#35559=CARTESIAN_POINT('Ctrl Pts',(0.00212674943784686,-0.0231806570105422,
-0.0108617236017027));
#35560=CARTESIAN_POINT('Ctrl Pts',(0.00205135317620363,-0.0231897895986188,
-0.010739704474585));
#35561=CARTESIAN_POINT('Ctrl Pts',(0.00196673295883021,-0.0231987703694879,
-0.0106262870985233));
#35562=CARTESIAN_POINT('Ctrl Pts',(0.0018751024366552,-0.0232075993232843,
-0.0105223748766447));
#35563=CARTESIAN_POINT('Ctrl Pts',(0.00156402163431762,-0.0232375731569542,
-0.0101695983499222));
#35564=CARTESIAN_POINT('Ctrl Pts',(0.00117274164898975,-0.0232657971974777,
-0.00992911309264385));
#35565=CARTESIAN_POINT('Ctrl Pts',(0.000777232675165815,-0.0232922714290193,
-0.00979974104833058));
#35566=CARTESIAN_POINT('Ctrl Pts',(0.000699884479445959,-0.0232974488944583,
-0.00977444024641079));
#35567=CARTESIAN_POINT('Ctrl Pts',(0.000622300010692386,-0.0233025594364456,
-0.00975324549795641));
#35568=CARTESIAN_POINT('Ctrl Pts',(0.000544923280299288,-0.0233076030548627,
-0.00973596422789419));
#35569=CARTESIAN_POINT('Ctrl Pts',(0.000104622388244895,-0.0233363030228884,
-0.00963762770494246));
#35570=CARTESIAN_POINT('Ctrl Pts',(-0.00032401863768543,-0.0233628359980385,
-0.00966754509154558));
#35571=CARTESIAN_POINT('Ctrl Pts',(-0.000691942356854824,-0.0233872020603341,
-0.00977351780316071));
#35572=CARTESIAN_POINT('Ctrl Pts',(-0.000719292763144957,-0.0233890133643321,
-0.00978139551412994));
#35573=CARTESIAN_POINT('Ctrl Pts',(-0.000746330545010817,-0.023390812693939,
-0.0097896890216873));
#35574=CARTESIAN_POINT('Ctrl Pts',(-0.000773046138872332,-0.0233926000491877,
-0.0097983757015587));
#35575=CARTESIAN_POINT('Ctrl Pts',(-0.00115914581460374,-0.0234184313028566,
-0.00992391752177489));
#35576=CARTESIAN_POINT('Ctrl Pts',(-0.00147308347060864,-0.0234417615118279,
-0.0101295750295813));
#35577=CARTESIAN_POINT('Ctrl Pts',(-0.00171174468177345,-0.0234625903062594,
-0.0103537857399451));
#35578=CARTESIAN_POINT('Ctrl Pts',(-0.00195040589293826,-0.0234834191006908,
-0.0105779964503089));
#35579=CARTESIAN_POINT('Ctrl Pts',(-0.00211476129448352,-0.0235017464805822,
-0.0108194934548951));
#35580=CARTESIAN_POINT('Ctrl Pts',(-0.00222770154972694,-0.0235175738260776,
-0.0110412406630851));
#35581=CARTESIAN_POINT('Ctrl Pts',(-0.00234064180497036,-0.0235334011715729,
-0.0112629878712752));
#35582=CARTESIAN_POINT('Ctrl Pts',(-0.00240271876911905,-0.0235467284826722,
-0.011464576329171));
#35583=CARTESIAN_POINT('Ctrl Pts',(-0.00243983608043265,-0.0235575506086425,
-0.0116306928508889));
#35584=CARTESIAN_POINT('Ctrl Pts',(-0.00245839473608945,-0.0235629616716276,
-0.0117137511117478));
#35585=CARTESIAN_POINT('Ctrl Pts',(-0.00247059122038172,-0.0235677464383304,
-0.0117879608720915));
#35586=CARTESIAN_POINT('Ctrl Pts',(-0.00247904539026384,-0.0235719114734548,
-0.0118528456194485));
#35587=CARTESIAN_POINT('Ctrl Pts',(-0.00248749956014596,-0.0235760765085792,
-0.0119177303668055));
#35588=CARTESIAN_POINT('Ctrl Pts',(-0.0024921973665701,-0.0235796218121251,
-0.0119732972404837));
#35589=CARTESIAN_POINT('Ctrl Pts',(-0.00249506056939557,-0.0235825206539539,
-0.0120187776517592));
#35590=CARTESIAN_POINT('Ctrl Pts',(-0.0024964921708083,-0.0235839700748683,
-0.012041517857397));
#35591=CARTESIAN_POINT('Ctrl Pts',(-0.00249746073549553,-0.0235852578803534,
-0.0120617362495059));
#35592=CARTESIAN_POINT('Ctrl Pts',(-0.00249816045946761,-0.0235864183625859,
-0.0120799662762149));
#35593=CARTESIAN_POINT('Ctrl Pts',(-0.0024988601834397,-0.0235875788448184,
-0.0120981963029239));
#35594=CARTESIAN_POINT('Ctrl Pts',(-0.00249927457514363,-0.0235886120037982,
-0.0121144391812369));
#35595=CARTESIAN_POINT('Ctrl Pts',(-0.00249951245441347,-0.0235893781501396,
-0.0121264823413376));
#35596=CARTESIAN_POINT('Ctrl Pts',(-0.00249975033368331,-0.023590144296481,
-0.0121385255014383));
#35597=CARTESIAN_POINT('Ctrl Pts',(-0.00249984712543923,-0.0235906434301841,
-0.0121463673677798));
#35598=CARTESIAN_POINT('Ctrl Pts',(-0.00249992599526052,-0.0235912943128788,
-0.0121566174288783));
#35599=CARTESIAN_POINT('Ctrl Pts',(-0.00249996543017117,-0.0235916197542261,
-0.0121617424594276));
#35600=CARTESIAN_POINT('Ctrl Pts',(-0.00249997734888517,-0.0235918394918372,
-0.0121652016109821));
#35601=CARTESIAN_POINT('Ctrl Pts',(-0.00249997918792211,-0.023591868492253,
-0.012165652308355));
#35602=CARTESIAN_POINT('Ctrl Pts',(-0.00249998102695905,-0.0235918974926687,
-0.0121661030057279));
#35603=CARTESIAN_POINT('Ctrl Pts',(-0.00250002847430832,-0.0235921907273404,
-0.012170729115383));
#35604=CARTESIAN_POINT('Ctrl Pts',(-0.00249998763931371,-0.0235930136443261,
-0.0121837147926892));
#35605=CARTESIAN_POINT('Ctrl Pts',(-0.00249994680431911,-0.0235938365613117,
-0.0121967004699954));
#35606=CARTESIAN_POINT('Ctrl Pts',(-0.00249928104897629,-0.0235973078898677,
-0.0122515009405181));
#35607=CARTESIAN_POINT('Ctrl Pts',(-0.00249703476091654,-0.023600232019034,
-0.012297580041113));
#35608=CARTESIAN_POINT('Ctrl Pts',(-0.00249478847285679,-0.0236031561482002,
-0.012343659141708));
#35609=CARTESIAN_POINT('Ctrl Pts',(-0.00249187034452298,-0.0236055330779767,
-0.0123810623250591));
#35610=CARTESIAN_POINT('Ctrl Pts',(-0.00248805263063428,-0.023608010349694,
-0.0124199723296372));
#35611=CARTESIAN_POINT('Ctrl Pts',(-0.00248041720285686,-0.0236129648931285,
-0.0124977923387934));
#35612=CARTESIAN_POINT('Ctrl Pts',(-0.00246825871826857,-0.0236183208043258,
-0.0125815028094976));
#35613=CARTESIAN_POINT('Ctrl Pts',(-0.00245213816847964,-0.02362357025559,
-0.0126626986446394));
#35614=CARTESIAN_POINT('Ctrl Pts',(-0.00243601761869071,-0.0236288197068541,
-0.0127438944797812));
#35615=CARTESIAN_POINT('Ctrl Pts',(-0.00241625300993701,-0.0236339626981851,
-0.012822672110062));
#35616=CARTESIAN_POINT('Ctrl Pts',(-0.00239260239173008,-0.0236391344875873,
-0.0129007352045886));
#35617=CARTESIAN_POINT('Ctrl Pts',(-0.00236895177352315,-0.0236443062769895,
-0.0129787982991151));
#35618=CARTESIAN_POINT('Ctrl Pts',(-0.00234133816747274,-0.0236495068644631,
-0.0130561057737264));
#35619=CARTESIAN_POINT('Ctrl Pts',(-0.00231001880530941,-0.023654703045686,
-0.0131317890161534));
#35620=CARTESIAN_POINT('Ctrl Pts',(-0.00224738008098274,-0.0236650954081317,
-0.0132831555010074));
#35621=CARTESIAN_POINT('Ctrl Pts',(-0.00216995704282236,-0.0236754701455747,
-0.0134280726485577));
#35622=CARTESIAN_POINT('Ctrl Pts',(-0.00207910465144895,-0.023685853140187,
-0.0135641341833234));
#35623=CARTESIAN_POINT('Ctrl Pts',(-0.00198825226007553,-0.0236962361347994,
-0.013700195718089));
#35624=CARTESIAN_POINT('Ctrl Pts',(-0.00188395549441474,-0.0237066273865811,
-0.0138273654487582));
#35625=CARTESIAN_POINT('Ctrl Pts',(-0.00176827181384625,-0.0237170205390933,
-0.0139431152344189));
#35626=CARTESIAN_POINT('Ctrl Pts',(-0.00153690445270928,-0.0237378068441178,
-0.0141746148057404));
#35627=CARTESIAN_POINT('Ctrl Pts',(-0.00125955589036972,-0.0237586007520643,
-0.0143600247471864));
#35628=CARTESIAN_POINT('Ctrl Pts',(-0.000957255209870739,-0.0237794072501214,
-0.0144853256209183));
#35629=CARTESIAN_POINT('Ctrl Pts',(-0.000654954529371758,-0.0238002137481785,
-0.0146106264946503));
#35630=CARTESIAN_POINT('Ctrl Pts',(-0.000327662745678227,-0.023821032836346,
-0.0146757918206047));
#35631=CARTESIAN_POINT('Ctrl Pts',(-4.69308788134662E-7,-0.02384186317877,
-0.014675853242508));
#35632=CARTESIAN_POINT('Ctrl Pts',(0.000326724128101958,-0.0238626935211941,
-0.0146759146644112));
#35633=CARTESIAN_POINT('Ctrl Pts',(0.000653877233610468,-0.0238835351178747,
-0.0146109397642855));
#35634=CARTESIAN_POINT('Ctrl Pts',(0.000956388057863023,-0.0239043883250395,
-0.0144856848567764));
#35635=CARTESIAN_POINT('Ctrl Pts',(0.00125889888211558,-0.0239252415322042,
-0.0143604299492672));
#35636=CARTESIAN_POINT('Ctrl Pts',(0.00153643866694449,-0.0239461063498532,
-0.0141749069905738));
#35637=CARTESIAN_POINT('Ctrl Pts',(0.00176760817590136,-0.0239669826889295,
-0.0139437790023297));
#35638=CARTESIAN_POINT('Ctrl Pts',(0.0021151382352358,-0.0239983672577275,
-0.0135963113634064));
#35639=CARTESIAN_POINT('Ctrl Pts',(0.00235715461429183,-0.0240297778658631,
-0.0131433768144827));
#35640=CARTESIAN_POINT('Ctrl Pts',(0.00245257461427401,-0.0240612145511598,
-0.0126604951764301));
#35641=CARTESIAN_POINT('Ctrl Pts',(0.00248409625812313,-0.0240715995438019,
-0.0125009770144219));
#35642=CARTESIAN_POINT('Ctrl Pts',(0.00250000029698955,-0.0240819873822101,
-0.012338390140462));
#35643=CARTESIAN_POINT('Ctrl Pts',(0.00249999999999583,-0.0240923780677479,
-0.0121758487185883));
#35644=CARTESIAN_POINT('',(0.00249999990985199,-0.0250924186728815,-0.012175385970229));
#35645=CARTESIAN_POINT('Ctrl Pts',(0.00249999974369977,-0.0240924495244571,
-0.0121747212525069));
#35646=CARTESIAN_POINT('Ctrl Pts',(0.00249977984012064,-0.0241233665601626,
-0.0116890831297981));
#35647=CARTESIAN_POINT('Ctrl Pts',(0.00235376883046109,-0.024154283595868,
-0.011203535107439));
#35648=CARTESIAN_POINT('Ctrl Pts',(0.00208632057554545,-0.0241852006315734,
-0.0107984403288524));
#35649=CARTESIAN_POINT('Ctrl Pts',(0.00199335298094986,-0.02419594769157,
-0.0106576254741796));
#35650=CARTESIAN_POINT('Ctrl Pts',(0.00188616035506248,-0.0242066947515666,
-0.010526385852805));
#35651=CARTESIAN_POINT('Ctrl Pts',(0.00176706770513845,-0.0242174418115632,
-0.010407387362245));
#35652=CARTESIAN_POINT('Ctrl Pts',(0.00143077553186628,-0.0242477892105408,
-0.010071361074879));
#35653=CARTESIAN_POINT('Ctrl Pts',(0.000994267223898821,-0.0242781366095183,
-0.00983300824219008));
#35654=CARTESIAN_POINT('Ctrl Pts',(0.00052806958498167,-0.0243084840084958,
-0.00973226115336212));
#35655=CARTESIAN_POINT('Ctrl Pts',(0.000354222155843106,-0.0243198007052203,
-0.00969469206050567));
#35656=CARTESIAN_POINT('Ctrl Pts',(0.000176510666734036,-0.0243311174019448,
-0.00967579345856524));
#35657=CARTESIAN_POINT('Ctrl Pts',(-8.4534646565241E-7,-0.0243424340986693,
-0.00967585342948023));
#35658=CARTESIAN_POINT('Ctrl Pts',(-0.000478210896877666,-0.0243728937434441,
-0.00967601484520181));
#35659=CARTESIAN_POINT('Ctrl Pts',(-0.000957059738941487,-0.0244033533882188,
-0.00981722155050242));
#35660=CARTESIAN_POINT('Ctrl Pts',(-0.0013588336126529,-0.0244338130329935,
-0.0100773845083475));
#35661=CARTESIAN_POINT('Ctrl Pts',(-0.00150662442522366,-0.0244450174839208,
-0.0101730843471288));
#35662=CARTESIAN_POINT('Ctrl Pts',(-0.00164412826440501,-0.024456221934848,
-0.0102843780503469));
#35663=CARTESIAN_POINT('Ctrl Pts',(-0.00176826327412012,-0.0244674263857754,
-0.0104085827941326));
#35664=CARTESIAN_POINT('Ctrl Pts',(-0.00210566471563643,-0.0244978803077024,
-0.0107461737742488));
#35665=CARTESIAN_POINT('Ctrl Pts',(-0.00234441242205592,-0.0245283342296294,
-0.0111845192387378));
#35666=CARTESIAN_POINT('Ctrl Pts',(-0.00244459956833509,-0.0245587881515564,
-0.0116524672430912));
#35667=CARTESIAN_POINT('Ctrl Pts',(-0.00248147873688702,-0.0245699983253314,
-0.0118247202113313));
#35668=CARTESIAN_POINT('Ctrl Pts',(-0.00250003919620521,-0.0245812084991065,
-0.0120007294925313));
#35669=CARTESIAN_POINT('Ctrl Pts',(-0.00249999993758005,-0.0245924186728815,
-0.0121764119454272));
#35670=CARTESIAN_POINT('Ctrl Pts',(-0.00249989328632472,-0.0246228725948085,
-0.0126536765991072));
#35671=CARTESIAN_POINT('Ctrl Pts',(-0.0023587989597219,-0.0246533265167354,
-0.0131324578205044));
#35672=CARTESIAN_POINT('Ctrl Pts',(-0.00209877251553004,-0.0246837804386625,
-0.0135342177177973));
#35673=CARTESIAN_POINT('Ctrl Pts',(-0.00200305605469169,-0.0246949906124375,
-0.0136821066588439));
#35674=CARTESIAN_POINT('Ctrl Pts',(-0.00189172719648904,-0.0247062007862125,
-0.0138197012239855));
#35675=CARTESIAN_POINT('Ctrl Pts',(-0.00176747325647235,-0.0247174109599876,
-0.0139439138872319));
#35676=CARTESIAN_POINT('Ctrl Pts',(-0.0014298575378662,-0.0247478706047623,
-0.0142814174509523));
#35677=CARTESIAN_POINT('Ctrl Pts',(-0.000991445184562082,-0.0247783302495369,
-0.0145202373086957));
#35678=CARTESIAN_POINT('Ctrl Pts',(-0.000523409044334443,-0.0248087898943116,
-0.0146204479303199));
#35679=CARTESIAN_POINT('Ctrl Pts',(-0.000351243938529629,-0.024819994345239,
-0.0146573099817553));
#35680=CARTESIAN_POINT('Ctrl Pts',(-0.000175324927440846,-0.0248311987961663,
-0.0146758723746888));
#35681=CARTESIAN_POINT('Ctrl Pts',(2.71971265063508E-7,-0.0248424032470937,
-0.0146758532717644));
#35682=CARTESIAN_POINT('Ctrl Pts',(0.000475878422558642,-0.0248727506460713,
-0.0146758015312488));
#35683=CARTESIAN_POINT('Ctrl Pts',(0.000953148934426867,-0.0249030980450488,
-0.0145357066301931));
#35684=CARTESIAN_POINT('Ctrl Pts',(0.00135401726721916,-0.0249334454440264,
-0.0142774329876573));
#35685=CARTESIAN_POINT('Ctrl Pts',(0.00150350307165344,-0.0249447621407509,
-0.0141811214557643));
#35686=CARTESIAN_POINT('Ctrl Pts',(0.00164250888723086,-0.0249560788374753,
-0.0140688911999047));
#35687=CARTESIAN_POINT('Ctrl Pts',(0.00176785790397681,-0.0249673955341998,
-0.0139435292838344));
#35688=CARTESIAN_POINT('Ctrl Pts',(0.00211030942677976,-0.0249983125699053,
-0.0136010425202822));
#35689=CARTESIAN_POINT('Ctrl Pts',(0.00235098062427899,-0.025029229605611,
-0.0131552093338355));
#35690=CARTESIAN_POINT('Ctrl Pts',(0.00244882364769221,-0.0250601466413165,
-0.0126791054524783));
#35691=CARTESIAN_POINT('Ctrl Pts',(0.00248283482692923,-0.025070893701313,
-0.0125136071483643));
#35692=CARTESIAN_POINT('Ctrl Pts',(0.00249999900623557,-0.0250816407613094,
-0.0123446805186293));
#35693=CARTESIAN_POINT('Ctrl Pts',(0.00249999999995669,-0.0250923878213059,
-0.0121758680029006));
#35694=CARTESIAN_POINT('',(0.00249999972657487,-0.0260925452264452,-0.0121764958944254));
#35695=CARTESIAN_POINT('Ctrl Pts',(0.00249999981974729,-0.0250924495244571,
-0.0121749039375575));
#35696=CARTESIAN_POINT('Ctrl Pts',(0.00249981540284905,-0.0251233724506544,
-0.0116892635544426));
#35697=CARTESIAN_POINT('Ctrl Pts',(0.00235383859928715,-0.0251542953768517,
-0.0112037029975709));
#35698=CARTESIAN_POINT('Ctrl Pts',(0.00208641781767861,-0.025185218303049,
-0.010798587629514));
#35699=CARTESIAN_POINT('Ctrl Pts',(0.00199350618779638,-0.0251959620435183,
-0.0106578359313471));
#35700=CARTESIAN_POINT('Ctrl Pts',(0.00188638296860404,-0.0252067057839877,
-0.0105266489217477));
#35701=CARTESIAN_POINT('Ctrl Pts',(0.00176736936274355,-0.0252174495244571,
-0.0104076888327712));
#35702=CARTESIAN_POINT('Ctrl Pts',(0.00143113101664912,-0.0252478028399471,
-0.0100716016830753));
#35703=CARTESIAN_POINT('Ctrl Pts',(0.000994658671625173,-0.0252781561554371,
-0.0098331736123015));
#35704=CARTESIAN_POINT('Ctrl Pts',(0.000528473902838359,-0.0253085094709272,
-0.00973234856300654));
#35705=CARTESIAN_POINT('Ctrl Pts',(0.00035471654166248,-0.0253198228221038,
-0.00969476883994628));
#35706=CARTESIAN_POINT('Ctrl Pts',(0.000177095770510817,-0.0253311361732804,
-0.00967584087809031));
#35707=CARTESIAN_POINT('Ctrl Pts',(-1.750795227525E-7,-0.0253424495244571,
-0.00967585329268867));
#35708=CARTESIAN_POINT('Ctrl Pts',(-0.000477545299838025,-0.0253729150913717,
-0.00967588672378889));
#35709=CARTESIAN_POINT('Ctrl Pts',(-0.000956435630825558,-0.0254033806582862,
-0.00981696765543438));
#35710=CARTESIAN_POINT('Ctrl Pts',(-0.00135828107907325,-0.0254338462252008,
-0.0100770268263114));
#35711=CARTESIAN_POINT('Ctrl Pts',(-0.00150602528364958,-0.0254450473249529,
-0.0101726412858295));
#35712=CARTESIAN_POINT('Ctrl Pts',(-0.00164349666043961,-0.025456248424705,
-0.0102838371082915));
#35713=CARTESIAN_POINT('Ctrl Pts',(-0.00176761700091796,-0.0254674495244571,
-0.010407936394262));
#35714=CARTESIAN_POINT('Ctrl Pts',(-0.00210514504448296,-0.02549790936102,
-0.0107454071830146));
#35715=CARTESIAN_POINT('Ctrl Pts',(-0.00234405371722318,-0.025528369197583,
-0.0111836696319958));
#35716=CARTESIAN_POINT('Ctrl Pts',(-0.00244441050475252,-0.025558829034146,
-0.0116515849542553));
#35717=CARTESIAN_POINT('Ctrl Pts',(-0.00248133392898926,-0.0255700358642497,
-0.0118237410821666));
#35718=CARTESIAN_POINT('Ctrl Pts',(-0.00249995784166091,-0.0255812426943533,
-0.0119996564809227));
#35719=CARTESIAN_POINT('Ctrl Pts',(-0.00249999992819427,-0.0255924495244571,
-0.0121752540965862));
#35720=CARTESIAN_POINT('Ctrl Pts',(-0.00250011431816146,-0.02562290936102,
-0.0126525232819346));
#35721=CARTESIAN_POINT('Ctrl Pts',(-0.00235923919965624,-0.0256533691975828,
-0.0131313733530485));
#35722=CARTESIAN_POINT('Ctrl Pts',(-0.00209939501672301,-0.0256838290341457,
-0.0135332554243782));
#35723=CARTESIAN_POINT('Ctrl Pts',(-0.00200379274369099,-0.0256950358642495,
-0.0136811164966417));
#35724=CARTESIAN_POINT('Ctrl Pts',(-0.00189258855932867,-0.0257062426943533,
-0.0138187003778426));
#35725=CARTESIAN_POINT('Ctrl Pts',(-0.00176846425227196,-0.0257174495244571,
-0.0139429226650592));
#35726=CARTESIAN_POINT('Ctrl Pts',(-0.00143103454669657,-0.0257479150913717,
-0.0142806187279443));
#35727=CARTESIAN_POINT('Ctrl Pts',(-0.000992751745445068,-0.0257783806582862,
-0.0145196850860781));
#35728=CARTESIAN_POINT('Ctrl Pts',(-0.000524767767902572,-0.0258088462252008,
-0.0146201566207968));
#35729=CARTESIAN_POINT('Ctrl Pts',(-0.000352706790683817,-0.0258200473249529,
-0.0146570964120631));
#35730=CARTESIAN_POINT('Ctrl Pts',(-0.000176885396462903,-0.025831248424705,
-0.0146757564858568));
#35731=CARTESIAN_POINT('Ctrl Pts',(-1.37345940904288E-6,-0.0258424495244571,
-0.0146758529092799));
#35732=CARTESIAN_POINT('Ctrl Pts',(0.000474237803374116,-0.0258728028399471,
-0.0146761142024249));
#35733=CARTESIAN_POINT('Ctrl Pts',(0.000951604262650088,-0.0259031561554371,
-0.0145363307230201));
#35734=CARTESIAN_POINT('Ctrl Pts',(0.00135264445426317,-0.0259335094709272,
-0.0142783168368607));
#35735=CARTESIAN_POINT('Ctrl Pts',(0.00150212099250688,-0.0259448228221038,
-0.0141821493620578));
#35736=CARTESIAN_POINT('Ctrl Pts',(0.0016411380949844,-0.0259561361732805,
-0.0140700717454712));
#35737=CARTESIAN_POINT('Ctrl Pts',(0.00176652158658883,-0.0259674495244572,
-0.0139448647291767));
#35738=CARTESIAN_POINT('Ctrl Pts',(0.00210923387375378,-0.0259983724506545,
-0.0136026348042137));
#35739=CARTESIAN_POINT('Ctrl Pts',(0.00235024223510933,-0.0260292953768519,
-0.0131569809680466));
#35740=CARTESIAN_POINT('Ctrl Pts',(0.00244844407310773,-0.0260602183030492,
-0.0126809489417202));
#35741=CARTESIAN_POINT('Ctrl Pts',(0.00248256293541502,-0.0260709620435185,
-0.0125155582373186));
#35742=CARTESIAN_POINT('Ctrl Pts',(0.00249985412379925,-0.0260817057839878,
-0.0123467299594587));
#35743=CARTESIAN_POINT('Ctrl Pts',(0.0024999990774521,-0.0260924495244571,
-0.0121780010152726));
#35744=CARTESIAN_POINT('',(0.00250030482084482,-0.0270929049799219,-0.0121755425884962));
#35745=CARTESIAN_POINT('Ctrl Pts',(0.00249999999998503,-0.0260925855360718,
-0.0121758619383234));
#35746=CARTESIAN_POINT('Ctrl Pts',(0.00250000168063414,-0.026123477185258,
-0.0116902243085716));
#35747=CARTESIAN_POINT('Ctrl Pts',(0.00235421253766726,-0.0261543704232938,
-0.0112046101782478));
#35748=CARTESIAN_POINT('Ctrl Pts',(0.00199403555690222,-0.0261960117468405,
-0.0106585198828652));
#35749=CARTESIAN_POINT('Ctrl Pts',(0.00188688869552743,-0.0262067545940619,
-0.0105272170746364));
#35750=CARTESIAN_POINT('Ctrl Pts',(0.00143168700788836,-0.0262478328793858,
-0.0100719809913161));
#35751=CARTESIAN_POINT('Ctrl Pts',(0.000995281622552827,-0.0262781746182928,
-0.00983343888535285));
#35752=CARTESIAN_POINT('Ctrl Pts',(0.000355274318464984,-0.0263198252081222,
-0.00969484091355799));
#35753=CARTESIAN_POINT('Ctrl Pts',(0.000177548413150109,-0.0263311385297115,
-0.00967586537989346));
#35754=CARTESIAN_POINT('Ctrl Pts',(-0.000477186214621105,-0.0263728930165037,
-0.0096758207626205));
#35755=CARTESIAN_POINT('Ctrl Pts',(-0.000956084164253438,-0.0264033256581309,
-0.00981682778217999));
#35756=CARTESIAN_POINT('Ctrl Pts',(-0.00150581592258683,-0.0264450043787476,
-0.0101724736200223));
#35757=CARTESIAN_POINT('Ctrl Pts',(-0.00164338878537718,-0.0264562192685052,
-0.0102837326518929));
#35758=CARTESIAN_POINT('Ctrl Pts',(-0.00210513380752868,-0.0264979387827995,
-0.0107453867082514));
#35759=CARTESIAN_POINT('Ctrl Pts',(-0.00234405249367148,-0.0265284892035263,
-0.0111836595020973));
#35760=CARTESIAN_POINT('Ctrl Pts',(-0.00248135359723824,-0.0265701233990174,
-0.0118238344146244));
#35761=CARTESIAN_POINT('Ctrl Pts',(-0.00249997733682184,-0.0265813094217105,
-0.0119998426203243));
#35762=CARTESIAN_POINT('Ctrl Pts',(-0.00250006149980523,-0.0266227971072005,
-0.012652885375613));
#35763=CARTESIAN_POINT('Ctrl Pts',(-0.00235908466725583,-0.0266529419769236,
-0.0131318040709003));
#35764=CARTESIAN_POINT('Ctrl Pts',(-0.00200345043979713,-0.0266942330651809,
-0.0136815752320274));
#35765=CARTESIAN_POINT('Ctrl Pts',(-0.00189219565810716,-0.0267053439854017,
-0.013819156319645));
#35766=CARTESIAN_POINT('Ctrl Pts',(-0.00143061510762509,-0.0267467057992126,
-0.014280867634229));
#35767=CARTESIAN_POINT('Ctrl Pts',(-0.000992428644244417,-0.0267770625758946,
-0.0145197947799587));
#35768=CARTESIAN_POINT('Ctrl Pts',(-0.000352195105386843,-0.0268186881980405,
-0.0146571913964735));
#35769=CARTESIAN_POINT('Ctrl Pts',(-0.000176051527598052,-0.0268299035408566,
-0.0146758371889194));
#35770=CARTESIAN_POINT('Ctrl Pts',(0.000475393790923074,-0.0268714776936433,
-0.0146758967939031));
#35771=CARTESIAN_POINT('Ctrl Pts',(0.000952706281399202,-0.0269018704543449,
-0.0145358883263421));
#35772=CARTESIAN_POINT('Ctrl Pts',(0.00150320018578933,-0.0269436776881657,
-0.0141813551430691));
#35773=CARTESIAN_POINT('Ctrl Pts',(0.00164228050286924,-0.0269550442330534,
-0.0140690963115757));
#35774=CARTESIAN_POINT('Ctrl Pts',(0.00211017853281865,-0.0269974831572675,
-0.0136012369892513));
#35775=CARTESIAN_POINT('Ctrl Pts',(0.002350891697643,-0.0270286110534918,
-0.0131554239049857));
#35776=CARTESIAN_POINT('Ctrl Pts',(0.0024828208666546,-0.0270706431659741,
-0.0125137508768078));
#35777=CARTESIAN_POINT('Ctrl Pts',(0.00250000040700823,-0.0270814960885248,
-0.0123447418903043));
#35778=CARTESIAN_POINT('Ctrl Pts',(0.00249999999999274,-0.0270923558261894,
-0.0121758472618626));
#35779=CARTESIAN_POINT('',(0.00214222575379317,-0.0271787743239008,-0.0108871062905246));
#35780=CARTESIAN_POINT('Ctrl Pts',(0.00249999955999433,-0.0270924495244571,
-0.0121743700373619));
#35781=CARTESIAN_POINT('Ctrl Pts',(0.0024997320825269,-0.027121224457605,
-0.0117235398244762));
#35782=CARTESIAN_POINT('Ctrl Pts',(0.00237462822344567,-0.0271499993907529,
-0.0112734183970132));
#35783=CARTESIAN_POINT('Ctrl Pts',(0.00214222575379317,-0.0271787743239008,
-0.0108871062905246));
#35784=CARTESIAN_POINT('',(0.000601546286298534,-0.0271787743898723,-0.0146024027019709));
#35785=CARTESIAN_POINT('Origin',(0.,-0.0271787743898623,-0.0121758532865581));
#35786=CARTESIAN_POINT('Ctrl Pts',(0.000601546286299188,-0.0271787743898619,
-0.0146024027019708));
#35787=CARTESIAN_POINT('Ctrl Pts',(0.000126738896001363,-0.027147632217151,
-0.0147201083709866));
#35788=CARTESIAN_POINT('Ctrl Pts',(-0.000383109998025324,-0.02711649004444,
-0.0146942108575127));
#35789=CARTESIAN_POINT('Ctrl Pts',(-0.000843239394494906,-0.0270853478717291,
-0.0145293501154431));
#35790=CARTESIAN_POINT('Ctrl Pts',(-0.0008686421319187,-0.0270836285804987,
-0.0145202485145143));
#35791=CARTESIAN_POINT('Ctrl Pts',(-0.000893894938573373,-0.0270819092892684,
-0.0145107365109282));
#35792=CARTESIAN_POINT('Ctrl Pts',(-0.000918984460815858,-0.027080189998038,
-0.0145008194284146));
#35793=CARTESIAN_POINT('Ctrl Pts',(-0.00136814286693025,-0.0270494108504236,
-0.0143232815330307));
#35794=CARTESIAN_POINT('Ctrl Pts',(-0.001764642299577,-0.0270186317028091,
-0.0140114859226347));
#35795=CARTESIAN_POINT('Ctrl Pts',(-0.00204312006724602,-0.0269878525551947,
-0.0136165685224103));
#35796=CARTESIAN_POINT('Ctrl Pts',(-0.00206196005624111,-0.0269857702388677,
-0.0135898509875188));
#35797=CARTESIAN_POINT('Ctrl Pts',(-0.00208027307942609,-0.0269836879225407,
-0.0135627678475282));
#35798=CARTESIAN_POINT('Ctrl Pts',(-0.0020980451501482,-0.0269816056062137,
-0.0135353408914812));
#35799=CARTESIAN_POINT('Ctrl Pts',(-0.00236143589829022,-0.0269507446635681,
-0.0131288600381567));
#35800=CARTESIAN_POINT('Ctrl Pts',(-0.00250323124197211,-0.0269198837209227,
-0.0126433620392557));
#35801=CARTESIAN_POINT('Ctrl Pts',(-0.00249994239890872,-0.0268890227782772,
-0.0121588826608035));
#35802=CARTESIAN_POINT('Ctrl Pts',(-0.0024997292038465,-0.0268870222569812,
-0.0121274769022309));
#35803=CARTESIAN_POINT('Ctrl Pts',(-0.00249892415377076,-0.0268850217356852,
-0.0120960794293595));
#35804=CARTESIAN_POINT('Ctrl Pts',(-0.00249752835018408,-0.0268830212143892,
-0.0120647131046851));
#35805=CARTESIAN_POINT('Ctrl Pts',(-0.00247600401678539,-0.0268521716824375,
-0.0115810209604391));
#35806=CARTESIAN_POINT('Ctrl Pts',(-0.00230970714499795,-0.0268213221504857,
-0.011103562613496));
#35807=CARTESIAN_POINT('Ctrl Pts',(-0.00202594829224241,-0.026790472618534,
-0.0107110893065395));
#35808=CARTESIAN_POINT('Ctrl Pts',(-0.00200744222498325,-0.0267884606865443,
-0.0106854931450614));
#35809=CARTESIAN_POINT('Ctrl Pts',(-0.00198845358085418,-0.0267864487545546,
-0.0106602512927708));
#35810=CARTESIAN_POINT('Ctrl Pts',(-0.00196899678345204,-0.0267844368225649,
-0.0106353820382852));
#35811=CARTESIAN_POINT('Ctrl Pts',(-0.00167066011192626,-0.0267535872906131,
-0.0102540546053463));
#35812=CARTESIAN_POINT('Ctrl Pts',(-0.00125806535609302,-0.0267227377586614,
-0.00996184533361782));
#35813=CARTESIAN_POINT('Ctrl Pts',(-0.000799163457009108,-0.0266918882267096,
-0.00980702704367298));
#35814=CARTESIAN_POINT('Ctrl Pts',(-0.000769234983140153,-0.0266898762947199,
-0.00979693016860164));
#35815=CARTESIAN_POINT('Ctrl Pts',(-0.000739119260466096,-0.0266878643627303,
-0.00978740194915553));
#35816=CARTESIAN_POINT('Ctrl Pts',(-0.000708838650548186,-0.0266858524307406,
-0.00977844890525548));
#35817=CARTESIAN_POINT('Ctrl Pts',(-0.000244365611328204,-0.0266549914880951,
-0.00964111853041157));
#35818=CARTESIAN_POINT('Ctrl Pts',(0.000261411968019987,-0.0266241305454496,
-0.00964279177763323));
#35819=CARTESIAN_POINT('Ctrl Pts',(0.000725083113859513,-0.0265932696028041,
-0.00978331185995839));
#35820=CARTESIAN_POINT('Ctrl Pts',(0.000755140005258831,-0.0265912690815081,
-0.00979242089529899));
#35821=CARTESIAN_POINT('Ctrl Pts',(0.000785021163560474,-0.0265892685602122,
-0.00980209517023468));
#35822=CARTESIAN_POINT('Ctrl Pts',(0.000814704975023284,-0.0265872680389162,
-0.00981232714884092));
#35823=CARTESIAN_POINT('Ctrl Pts',(0.00127140714391061,-0.0265564888913018,
-0.00996975190634997));
#35824=CARTESIAN_POINT('Ctrl Pts',(0.00168135077208624,-0.0265257097436874,
-0.0102636595335939));
#35825=CARTESIAN_POINT('Ctrl Pts',(0.00197705538432398,-0.026494930596073,
-0.0106457382558119));
#35826=CARTESIAN_POINT('Ctrl Pts',(0.00199706082923621,-0.026492848279746,
-0.010671587209508));
#35827=CARTESIAN_POINT('Ctrl Pts',(0.00201655600260596,-0.0264907659634189,
-0.0106978243520202));
#35828=CARTESIAN_POINT('Ctrl Pts',(0.0020355260119502,-0.0264886836470919,
-0.0107244285194158));
#35829=CARTESIAN_POINT('Ctrl Pts',(0.00231923281463639,-0.0264575414743809,
-0.0111223083060285));
#35830=CARTESIAN_POINT('Ctrl Pts',(0.00248283134186161,-0.0264263993016699,
-0.0116058591319997));
#35831=CARTESIAN_POINT('Ctrl Pts',(0.00249868673047212,-0.0263952571289589,
-0.0120948309256781));
#35832=CARTESIAN_POINT('Ctrl Pts',(0.00249956207179293,-0.0263935378377284,
-0.0121218259887593));
#35833=CARTESIAN_POINT('Ctrl Pts',(0.00249999986217964,-0.026391818546498,
-0.012148833995825));
#35834=CARTESIAN_POINT('Ctrl Pts',(0.00249999999996746,-0.0263900992552675,
-0.0121758405315141));
#35835=CARTESIAN_POINT('Origin',(0.,-0.0271787743898723,-0.0121758532865581));
#35836=CARTESIAN_POINT('',(-0.00299896195254882,-0.0191803670938455,-0.012169853924649));
#35837=CARTESIAN_POINT('',(0.00299896819192659,-0.019680486974571,-0.0121759389411417));
#35838=CARTESIAN_POINT('Ctrl Pts',(-0.00299896195254882,-0.0191803670938455,
-0.012169853924649));
#35839=CARTESIAN_POINT('Ctrl Pts',(-0.00299880224766938,-0.0191818636123297,
-0.0121992568003792));
#35840=CARTESIAN_POINT('Ctrl Pts',(-0.00299852404358193,-0.0191833290209218,
-0.0122250123092027));
#35841=CARTESIAN_POINT('Ctrl Pts',(-0.00299800114766971,-0.0191846148334388,
-0.0122482025519681));
#35842=CARTESIAN_POINT('Ctrl Pts',(-0.00299740209262557,-0.0191860879229316,
-0.0122747704244237));
#35843=CARTESIAN_POINT('Ctrl Pts',(-0.00299648390590115,-0.0191873213968317,
-0.0122979737332858));
#35844=CARTESIAN_POINT('Ctrl Pts',(-0.00299528035553771,-0.0191885761336485,
-0.0123217600538735));
#35845=CARTESIAN_POINT('Ctrl Pts',(-0.00299287325481085,-0.0191910856072822,
-0.0123693326950491));
#35846=CARTESIAN_POINT('Ctrl Pts',(-0.0029892837839955,-0.0191937517300053,
-0.0124192300566519));
#35847=CARTESIAN_POINT('Ctrl Pts',(-0.00298449948012424,-0.0191963745757028,
-0.0124685748257699));
#35848=CARTESIAN_POINT('Ctrl Pts',(-0.0029749308723817,-0.0192016202670976,
-0.0125672643640059));
#35849=CARTESIAN_POINT('Ctrl Pts',(-0.00296064216996607,-0.0192065882359609,
-0.0126637584356527));
#35850=CARTESIAN_POINT('Ctrl Pts',(-0.00294167528334986,-0.0192114919847212,
-0.01275981020314));
#35851=CARTESIAN_POINT('Ctrl Pts',(-0.00292270839673364,-0.0192163957334815,
-0.0128558619706273));
#35852=CARTESIAN_POINT('Ctrl Pts',(-0.00289904298078549,-0.0192212721522644,
-0.0129514639649636));
#35853=CARTESIAN_POINT('Ctrl Pts',(-0.00287077868553411,-0.0192260969694797,
-0.0130455753309895));
#35854=CARTESIAN_POINT('Ctrl Pts',(-0.00284251439028272,-0.019230921786695,
-0.0131396866970154));
#35855=CARTESIAN_POINT('Ctrl Pts',(-0.00280965551856699,-0.0192356858357989,
-0.0132323106181608));
#35856=CARTESIAN_POINT('Ctrl Pts',(-0.0027723055452403,-0.0192404774689402,
-0.013323121329571));
#35857=CARTESIAN_POINT('Ctrl Pts',(-0.00270257498363687,-0.0192494232121411,
-0.0134926604575071));
#35858=CARTESIAN_POINT('Ctrl Pts',(-0.00261717238342509,-0.019258491751231,
-0.0136559066227712));
#35859=CARTESIAN_POINT('Ctrl Pts',(-0.00251731130281746,-0.0192682599616135,
-0.0138097133907207));
#35860=CARTESIAN_POINT('Ctrl Pts',(-0.00251019465052561,-0.0192689560982503,
-0.0138206745107183));
#35861=CARTESIAN_POINT('Ctrl Pts',(-0.00250300455829962,-0.0192696557883602,
-0.0138315880401406));
#35862=CARTESIAN_POINT('Ctrl Pts',(-0.00249574239501426,-0.0192703592407384,
-0.013842453612651));
#35863=CARTESIAN_POINT('Ctrl Pts',(-0.00238657733645111,-0.0192809335582027,
-0.0140057852278754));
#35864=CARTESIAN_POINT('Ctrl Pts',(-0.00226104203758436,-0.0192922469269428,
-0.0141580541481476));
#35865=CARTESIAN_POINT('Ctrl Pts',(-0.00212187971374463,-0.0193034712736315,
-0.0142965100605622));
#35866=CARTESIAN_POINT('Ctrl Pts',(-0.00184355506606512,-0.0193259199670087,
-0.0145734218853915));
#35867=CARTESIAN_POINT('Ctrl Pts',(-0.00151080520325619,-0.0193478617734335,
-0.0147952418066359));
#35868=CARTESIAN_POINT('Ctrl Pts',(-0.00114835782098663,-0.0193677192990411,
-0.0149461198238439));
#35869=CARTESIAN_POINT('Ctrl Pts',(-0.000790043872778773,-0.0193873503648183,
-0.0150952771931288));
#35870=CARTESIAN_POINT('Ctrl Pts',(-0.000402166286245195,-0.0194051547993873,
-0.0151750374146334));
#35871=CARTESIAN_POINT('Ctrl Pts',(-1.39131433410026E-5,-0.0194258308536781,
-0.0151767688928234));
#35872=CARTESIAN_POINT('Ctrl Pts',(-9.43433704985339E-6,-0.0194260693682754,
-0.0151767888667902));
#35873=CARTESIAN_POINT('Ctrl Pts',(-4.95535653832698E-6,-0.0194263082650118,
-0.0151767984904286));
#35874=CARTESIAN_POINT('Ctrl Pts',(-4.76237866949609E-7,-0.0194265475510998,
-0.0151767977970567));
#35875=CARTESIAN_POINT('Ctrl Pts',(0.000392283102934089,-0.0194475297694933,
-0.0151767369975265));
#35876=CARTESIAN_POINT('Ctrl Pts',(0.000784350710633772,-0.0194711918902264,
-0.0150970096259685));
#35877=CARTESIAN_POINT('Ctrl Pts',(0.00114706628041126,-0.0194929067069842,
-0.014946525686211));
#35878=CARTESIAN_POINT('Ctrl Pts',(0.00150978185018874,-0.019514621523742,
-0.0147960417464534));
#35879=CARTESIAN_POINT('Ctrl Pts',(0.00184354545898445,-0.0195344202044027,
-0.014574687276006));
#35880=CARTESIAN_POINT('Ctrl Pts',(0.00212119098327946,-0.0195531656601654,
-0.0142974175110577));
#35881=CARTESIAN_POINT('Ctrl Pts',(0.00226334811709381,-0.0195627635107702,
-0.014155452769582));
#35882=CARTESIAN_POINT('Ctrl Pts',(0.00239186651239939,-0.0195731695487958,
-0.0140003848492412));
#35883=CARTESIAN_POINT('Ctrl Pts',(0.00250275064154011,-0.0195840122226612,
-0.0138334451870744));
#35884=CARTESIAN_POINT('Ctrl Pts',(0.00282499616095954,-0.0196155226209365,
-0.013348294078764));
#35885=CARTESIAN_POINT('Ctrl Pts',(0.00299816054098966,-0.0196507207089565,
-0.0127602146141065));
#35886=CARTESIAN_POINT('Ctrl Pts',(0.00299896819192659,-0.019680486974571,
-0.0121759389411417));
#35887=CARTESIAN_POINT('',(0.00299999984374834,-0.0246800791551026,-0.0121768215375359));
#35888=CARTESIAN_POINT('Ctrl Pts',(0.00299999999774018,-0.0196810819667495,
-0.0121759697293255));
#35889=CARTESIAN_POINT('Ctrl Pts',(0.00300000942085986,-0.0196932559099264,
-0.0119331950198641));
#35890=CARTESIAN_POINT('Ctrl Pts',(0.00297055154201463,-0.0197045033254348,
-0.0116913234487237));
#35891=CARTESIAN_POINT('Ctrl Pts',(0.00288497146224982,-0.0197215353186389,
-0.0113452722338703));
#35892=CARTESIAN_POINT('Ctrl Pts',(0.00285142836003338,-0.0197270473697668,
-0.0112365570788726));
#35893=CARTESIAN_POINT('Ctrl Pts',(0.00280154164464815,-0.0197343362154213,
-0.0111024332638439));
#35894=CARTESIAN_POINT('Ctrl Pts',(0.00279087696749342,-0.0197358535763954,
-0.0110750028145183));
#35895=CARTESIAN_POINT('Ctrl Pts',(0.00277416703216802,-0.0197381779544933,
-0.0110338276581702));
#35896=CARTESIAN_POINT('Ctrl Pts',(0.00276841903686469,-0.0197389686957665,
-0.0110199634666039));
#35897=CARTESIAN_POINT('Ctrl Pts',(0.00275771198906117,-0.0197404268147673,
-0.0109946760528532));
#35898=CARTESIAN_POINT('Ctrl Pts',(0.00275278551259007,-0.0197410923173646,
-0.010983239779294));
#35899=CARTESIAN_POINT('Ctrl Pts',(0.00274132094684287,-0.0197426287040395,
-0.0109570755732567));
#35900=CARTESIAN_POINT('Ctrl Pts',(0.00273473526014656,-0.0197435023038016,
-0.0109423693256647));
#35901=CARTESIAN_POINT('Ctrl Pts',(0.0027129404632505,-0.0197463630938318,
-0.0108947327789585));
#35902=CARTESIAN_POINT('Ctrl Pts',(0.00269725301474739,-0.0197483757861134,
-0.0108620261826589));
#35903=CARTESIAN_POINT('Ctrl Pts',(0.0025954709778507,-0.019761118544118,
-0.0106593317430168));
#35904=CARTESIAN_POINT('Ctrl Pts',(0.00249394052655557,-0.019772456052928,
-0.0104975916122593));
#35905=CARTESIAN_POINT('Ctrl Pts',(0.00228706715201482,-0.0197923412922303,
-0.0102286892166359));
#35906=CARTESIAN_POINT('Ctrl Pts',(0.00218772104820752,-0.019800934113632,
-0.0101176965903746));
#35907=CARTESIAN_POINT('Ctrl Pts',(0.00204046551884058,-0.0198123102878746,
-0.00997594539406847));
#35908=CARTESIAN_POINT('Ctrl Pts',(0.00199932318697792,-0.0198153622794282,
-0.00993848840368143));
#35909=CARTESIAN_POINT('Ctrl Pts',(0.00193639885452232,-0.0198198473456321,
-0.00988432323864402));
#35910=CARTESIAN_POINT('Ctrl Pts',(0.00191539231956945,-0.0198213157146306,
-0.00986673596299922));
#35911=CARTESIAN_POINT('Ctrl Pts',(0.00187704472145465,-0.0198239454088719,
-0.0098355136715209));
#35912=CARTESIAN_POINT('Ctrl Pts',(0.0018597887736179,-0.0198251107002371,
-0.00982177763943566));
#35913=CARTESIAN_POINT('Ctrl Pts',(0.001822282715594,-0.0198276056542681,
-0.00979259200263082));
#35914=CARTESIAN_POINT('Ctrl Pts',(0.00180198408116384,-0.0198289327384977,
-0.00977720740474276));
#35915=CARTESIAN_POINT('Ctrl Pts',(0.00174571834056147,-0.0198325499745693,
-0.00973568028140222));
#35916=CARTESIAN_POINT('Ctrl Pts',(0.00170936151388481,-0.0198348198162695,
-0.00971007545957484));
#35917=CARTESIAN_POINT('Ctrl Pts',(0.00149261545771245,-0.0198479892643146,
-0.00956452763602865));
#35918=CARTESIAN_POINT('Ctrl Pts',(0.00130023521666765,-0.0198581755577152,
-0.00946359988869757));
#35919=CARTESIAN_POINT('Ctrl Pts',(0.000996835947108489,-0.0198736423375735,
-0.00934419474795427));
#35920=CARTESIAN_POINT('Ctrl Pts',(0.000892909671420817,-0.0198788562507925,
-0.00930972665712547));
#35921=CARTESIAN_POINT('Ctrl Pts',(0.000730074500464841,-0.0198871927288724,
-0.00926543870069178));
#35922=CARTESIAN_POINT('Ctrl Pts',(0.000672363449334335,-0.0198901792665594,
-0.0092515673234337));
#35923=CARTESIAN_POINT('Ctrl Pts',(0.000595150796872156,-0.0198942613762364,
-0.00923541495603533));
#35924=CARTESIAN_POINT('Ctrl Pts',(0.000575980754474471,-0.0198952818794518,
-0.0092315998704853));
#35925=CARTESIAN_POINT('Ctrl Pts',(0.000544069140181193,-0.0198969943083237,
-0.00922557262594156));
#35926=CARTESIAN_POINT('Ctrl Pts',(0.000531347732794319,-0.0198976805498759,
-0.00922325497541845));
#35927=CARTESIAN_POINT('Ctrl Pts',(0.000506939874544787,-0.0198990047216707,
-0.0092189710781141));
#35928=CARTESIAN_POINT('Ctrl Pts',(0.000495256090501816,-0.0198996418414808,
-0.00921699171050771));
#35929=CARTESIAN_POINT('Ctrl Pts',(0.00046321519864308,-0.0199013973612555,
-0.00921175870693947));
#35930=CARTESIAN_POINT('Ctrl Pts',(0.000442836148301305,-0.0199025231115508,
-0.00920864566046527));
#35931=CARTESIAN_POINT('Ctrl Pts',(0.000359542717456324,-0.019907157220927,
-0.0091967991606986));
#35932=CARTESIAN_POINT('Ctrl Pts',(0.000296393888987575,-0.019910746820327,
-0.0091898552821384));
#35933=CARTESIAN_POINT('Ctrl Pts',(6.65736953401946E-5,-0.0199239765889576,
-0.00917194590946633));
#35934=CARTESIAN_POINT('Ctrl Pts',(-0.00010071849450859,-0.0199339043657393,
-0.00917289703441693));
#35935=CARTESIAN_POINT('Ctrl Pts',(-0.000376889693571773,-0.0199501171452961,
-0.00919757977549564));
#35936=CARTESIAN_POINT('Ctrl Pts',(-0.000486101343359905,-0.0199564864687802,
-0.00921344419637997));
#35937=CARTESIAN_POINT('Ctrl Pts',(-0.000665312466432556,-0.0199667846106084,
-0.0092496572911397));
#35938=CARTESIAN_POINT('Ctrl Pts',(-0.000735885303288047,-0.0199708006126325,
-0.00926660291706258));
#35939=CARTESIAN_POINT('Ctrl Pts',(-0.000834885786172269,-0.0199763769904146,
-0.00929420812692323));
#35940=CARTESIAN_POINT('Ctrl Pts',(-0.000863869378479237,-0.019978002586475,
-0.00930276385362857));
#35941=CARTESIAN_POINT('Ctrl Pts',(-0.00091409052330962,-0.0199808080416776,
-0.00931841744172763));
#35942=CARTESIAN_POINT('Ctrl Pts',(-0.000935386692247302,-0.0199819941215276,
-0.00932531774659095));
#35943=CARTESIAN_POINT('Ctrl Pts',(-0.000979314076889665,-0.0199844338868793,
-0.00934009623424393));
#35944=CARTESIAN_POINT('Ctrl Pts',(-0.00100193218597993,-0.0199856863665396,
-0.00934800851370281));
#35945=CARTESIAN_POINT('Ctrl Pts',(-0.0010605615242782,-0.0199889245151301,
-0.00936931001272005));
#35946=CARTESIAN_POINT('Ctrl Pts',(-0.00109641516670566,-0.0199908963149319,
-0.00938312167629061));
#35947=CARTESIAN_POINT('Ctrl Pts',(-0.0012831739973483,-0.0200011374855641,
-0.00945921676269332));
#35948=CARTESIAN_POINT('Ctrl Pts',(-0.00142908240008463,-0.0200090154656167,
-0.00953305550697632));
#35949=CARTESIAN_POINT('Ctrl Pts',(-0.00170369694802678,-0.0200243327118081,
-0.00970145330428935));
#35950=CARTESIAN_POINT('Ctrl Pts',(-0.00183231026747759,-0.0200317587103755,
-0.00979512378401006));
#35951=CARTESIAN_POINT('Ctrl Pts',(-0.00199021555579363,-0.0200419362372399,
-0.00993053393145888));
#35952=CARTESIAN_POINT('Ctrl Pts',(-0.00202674145422159,-0.0200443743030958,
-0.00996344834147788));
#35953=CARTESIAN_POINT('Ctrl Pts',(-0.00208764533376151,-0.0200486174838141,
-0.0100211046748876));
#35954=CARTESIAN_POINT('Ctrl Pts',(-0.00211243314293161,-0.0200503976619801,
-0.0100454001323372));
#35955=CARTESIAN_POINT('Ctrl Pts',(-0.00214802909963873,-0.0200530429173887,
-0.0100815211149638));
#35956=CARTESIAN_POINT('Ctrl Pts',(-0.00215917365006069,-0.0200538842751676,
-0.0100930125858848));
#35957=CARTESIAN_POINT('Ctrl Pts',(-0.00217880792384195,-0.0200553913300773,
-0.0101135849830775));
#35958=CARTESIAN_POINT('Ctrl Pts',(-0.00218733395524536,-0.0200560542955639,
-0.0101226302875094));
#35959=CARTESIAN_POINT('Ctrl Pts',(-0.00220623921133514,-0.0200575436798906,
-0.0101429383593398));
#35960=CARTESIAN_POINT('Ctrl Pts',(-0.00221658846832652,-0.0200583721440548,
-0.0101542276780704));
#35961=CARTESIAN_POINT('Ctrl Pts',(-0.00224762053487566,-0.0200608949479944,
-0.0101886032574669));
#35962=CARTESIAN_POINT('Ctrl Pts',(-0.00226803186464373,-0.0200626071380429,
-0.0102119306656247));
#35963=CARTESIAN_POINT('Ctrl Pts',(-0.00237867623234598,-0.0200721648017542,
-0.0103424078821197));
#35964=CARTESIAN_POINT('Ctrl Pts',(-0.0024616746123822,-0.0200803677998503,
-0.0104554535792134));
#35965=CARTESIAN_POINT('Ctrl Pts',(-0.00260416314206305,-0.0200960553509669,
-0.0106810602528687));
#35966=CARTESIAN_POINT('Ctrl Pts',(-0.00266500079234953,-0.0201035189721637,
-0.0107924352771941));
#35967=CARTESIAN_POINT('Ctrl Pts',(-0.00275158144974282,-0.0201153152728251,
-0.0109779887758199));
#35968=CARTESIAN_POINT('Ctrl Pts',(-0.00278178615861875,-0.0201197444727173,
-0.0110499105920363));
#35969=CARTESIAN_POINT('Ctrl Pts',(-0.00282921700862539,-0.0201272750004197,
-0.0111764543467603));
#35970=CARTESIAN_POINT('Ctrl Pts',(-0.00284774534043282,-0.0201304138390153,
-0.0112305415912974));
#35971=CARTESIAN_POINT('Ctrl Pts',(-0.00287293470464104,-0.0201349989912632,
-0.0113115546823074));
#35972=CARTESIAN_POINT('Ctrl Pts',(-0.00288078569278209,-0.0201364829528375,
-0.0113380945167813));
#35973=CARTESIAN_POINT('Ctrl Pts',(-0.00289418241640879,-0.0201391187464281,
-0.0113857984891497));
#35974=CARTESIAN_POINT('Ctrl Pts',(-0.00289986594512205,-0.0201402749035637,
-0.0114069215752569));
#35975=CARTESIAN_POINT('Ctrl Pts',(-0.00291159796098504,-0.0201427470703293,
-0.0114525054334494));
#35976=CARTESIAN_POINT('Ctrl Pts',(-0.00291757035792206,-0.0201440605934702,
-0.0114769841571138));
#35977=CARTESIAN_POINT('Ctrl Pts',(-0.00293294300647906,-0.0201476003020756,
-0.0115436261188216));
#35978=CARTESIAN_POINT('Ctrl Pts',(-0.00294174230999734,-0.0201498076448016,
-0.0115859225366728));
#35979=CARTESIAN_POINT('Ctrl Pts',(-0.00299131615892334,-0.0201635277426357,
-0.0118530195192053));
#35980=CARTESIAN_POINT('Ctrl Pts',(-0.00300721299564807,-0.0201742288384246,
-0.0120816661477068));
#35981=CARTESIAN_POINT('Ctrl Pts',(-0.00299241555553404,-0.0201899561963817,
-0.0124124718653403));
#35982=CARTESIAN_POINT('Ctrl Pts',(-0.00298256687078906,-0.0201948644538741,
-0.0125147218640876));
#35983=CARTESIAN_POINT('Ctrl Pts',(-0.00295911256298726,-0.0202027714239048,
-0.0126727590124251));
#35984=CARTESIAN_POINT('Ctrl Pts',(-0.00294911614480763,-0.0202056502094231,
-0.0127290039632965));
#35985=CARTESIAN_POINT('Ctrl Pts',(-0.00293360498392159,-0.0202096058214925,
-0.012803813373982));
#35986=CARTESIAN_POINT('Ctrl Pts',(-0.0029295068379246,-0.0202106133370104,
-0.0128226621625127));
#35987=CARTESIAN_POINT('Ctrl Pts',(-0.00292236951597387,-0.0202123100750276,
-0.0128540290138118));
#35988=CARTESIAN_POINT('Ctrl Pts',(-0.00291943088581132,-0.020212993836971,
-0.0128665697285904));
#35989=CARTESIAN_POINT('Ctrl Pts',(-0.00291322411689053,-0.0202144090540339,
-0.0128923099448489));
#35990=CARTESIAN_POINT('Ctrl Pts',(-0.00290994686141008,-0.0202151409576377,
-0.0129055067301678));
#35991=CARTESIAN_POINT('Ctrl Pts',(-0.00290096427991589,-0.0202171063427593,
-0.012940654327349));
#35992=CARTESIAN_POINT('Ctrl Pts',(-0.00289509965088559,-0.0202183482269523,
-0.0129625631033061));
#35993=CARTESIAN_POINT('Ctrl Pts',(-0.00286538194683253,-0.0202244419059285,
-0.0130687459525988));
#35994=CARTESIAN_POINT('Ctrl Pts',(-0.00283809595356002,-0.0202294493686955,
-0.0131520090316973));
#35995=CARTESIAN_POINT('Ctrl Pts',(-0.00273316094970527,-0.0202467199716527,
-0.0134304088053662));
#35996=CARTESIAN_POINT('Ctrl Pts',(-0.00263868528334712,-0.0202592514776756,
-0.0136185691746219));
#35997=CARTESIAN_POINT('Ctrl Pts',(-0.00248801231823542,-0.0202752362849872,
-0.0138535228774343));
#35998=CARTESIAN_POINT('Ctrl Pts',(-0.00244868556063563,-0.0202791419270268,
-0.0139104196688076));
#35999=CARTESIAN_POINT('Ctrl Pts',(-0.0023761801214289,-0.0202858874761807,
-0.0140079313815856));
#36000=CARTESIAN_POINT('Ctrl Pts',(-0.00234383847415808,-0.0202887549861224,
-0.0140491295043748));
#36001=CARTESIAN_POINT('Ctrl Pts',(-0.00229334912919302,-0.0202930262566952,
-0.014110088826567));
#36002=CARTESIAN_POINT('Ctrl Pts',(-0.00227598896752729,-0.0202944605377628,
-0.0141304866627678));
#36003=CARTESIAN_POINT('Ctrl Pts',(-0.00224527058404976,-0.0202969402845401,
-0.0141656159004601));
#36004=CARTESIAN_POINT('Ctrl Pts',(-0.00223203493829109,-0.0202979906240181,
-0.0141804518286653));
#36005=CARTESIAN_POINT('Ctrl Pts',(-0.00220173096618436,-0.0203003554421572,
-0.0142137474843456));
#36006=CARTESIAN_POINT('Ctrl Pts',(-0.00218457600651364,-0.0203016662110502,
-0.0142321265492309));
#36007=CARTESIAN_POINT('Ctrl Pts',(-0.00213749974708217,-0.0203051902298643,
-0.0142813077883869));
#36008=CARTESIAN_POINT('Ctrl Pts',(-0.00210714436952688,-0.0203073849279842,
-0.0143116872377933));
#36009=CARTESIAN_POINT('Ctrl Pts',(-0.00188553440550454,-0.0203228940255787,
-0.0145241479132106));
#36010=CARTESIAN_POINT('Ctrl Pts',(-0.00167164363907698,-0.0203350745480223,
-0.0146809153804785));
#36011=CARTESIAN_POINT('Ctrl Pts',(-0.00134576887739119,-0.0203528626470813,
-0.0148592171273823));
#36012=CARTESIAN_POINT('Ctrl Pts',(-0.00124885408079294,-0.0203580880841256,
-0.0149056692558978));
#36013=CARTESIAN_POINT('Ctrl Pts',(-0.00112316556939509,-0.0203650261742712,
-0.0149578170334922));
#36014=CARTESIAN_POINT('Ctrl Pts',(-0.00109650929841579,-0.0203665066015079,
-0.0149684310258501));
#36015=CARTESIAN_POINT('Ctrl Pts',(-0.00105582192866817,-0.0203687856210796,
-0.0149839595694495));
#36016=CARTESIAN_POINT('Ctrl Pts',(-0.00104189911941838,-0.0203695688786154,
-0.0149891550918779));
#36017=CARTESIAN_POINT('Ctrl Pts',(-0.00101622404757766,-0.0203710204979734,
-0.0149985194322769));
#36018=CARTESIAN_POINT('Ctrl Pts',(-0.00100448361276045,-0.0203716871161402,
-0.015002718713082));
#36019=CARTESIAN_POINT('Ctrl Pts',(-0.000977325480671667,-0.020373235510257,
-0.0150122420022128));
#36020=CARTESIAN_POINT('Ctrl Pts',(-0.000961890172656447,-0.0203741201632206,
-0.0150175135958196));
#36021=CARTESIAN_POINT('Ctrl Pts',(-0.00091089574395287,-0.0203770562240958,
-0.0150344665585622));
#36022=CARTESIAN_POINT('Ctrl Pts',(-0.000875162161939421,-0.0203791349404358,
-0.015045607951547));
#36023=CARTESIAN_POINT('Ctrl Pts',(-0.000657360091845289,-0.0203918946501266,
-0.0151090704720735));
#36024=CARTESIAN_POINT('Ctrl Pts',(-0.000470887041336941,-0.0204031659265746,
-0.0151447159342289));
#36025=CARTESIAN_POINT('Ctrl Pts',(-0.000134905140236743,-0.0204229443996268,
-0.0151764735785013));
#36026=CARTESIAN_POINT('Ctrl Pts',(1.33388720978418E-5,-0.0204314966286613,
-0.0151794763981626));
#36027=CARTESIAN_POINT('Ctrl Pts',(0.000216824902070318,-0.0204428391592764,
-0.0151685257942992));
#36028=CARTESIAN_POINT('Ctrl Pts',(0.00027234617117966,-0.020445894970584,
-0.0151639847926802));
#36029=CARTESIAN_POINT('Ctrl Pts',(0.000354954855349634,-0.0204503844475721,
-0.0151549065282144));
#36030=CARTESIAN_POINT('Ctrl Pts',(0.000382156524678651,-0.0204518535096552,
-0.0151515393627822));
#36031=CARTESIAN_POINT('Ctrl Pts',(0.000431157947552576,-0.0204544839487054,
-0.0151447906826176));
#36032=CARTESIAN_POINT('Ctrl Pts',(0.000452973558752462,-0.020455649301627,
-0.0151415406313959));
#36033=CARTESIAN_POINT('Ctrl Pts',(0.000499890259380584,-0.0204581438554286,
-0.0151340212848174));
#36034=CARTESIAN_POINT('Ctrl Pts',(0.000524976948216953,-0.020459470485612,
-0.0151296724132539));
#36035=CARTESIAN_POINT('Ctrl Pts',(0.000593671700948981,-0.0204630851143049,
-0.015116861097396));
#36036=CARTESIAN_POINT('Ctrl Pts',(0.000637152696479634,-0.0204653528529032,
-0.0151077485319775));
#36037=CARTESIAN_POINT('Ctrl Pts',(0.000891826619596656,-0.0204785434197699,
-0.0150484415238024));
#36038=CARTESIAN_POINT('Ctrl Pts',(0.00109726742167923,-0.0204887493580625,
-0.0149764120974078));
#36039=CARTESIAN_POINT('Ctrl Pts',(0.00139163601876189,-0.0205042254131153,
-0.0148357898537147));
#36040=CARTESIAN_POINT('Ctrl Pts',(0.00148747776550082,-0.0205094272115502,
-0.0147834040169232));
#36041=CARTESIAN_POINT('Ctrl Pts',(0.00163061781184453,-0.0205177467488282,
-0.014694701664933));
#36042=CARTESIAN_POINT('Ctrl Pts',(0.00168005016802281,-0.02052072911589,
-0.0146620033628829));
#36043=CARTESIAN_POINT('Ctrl Pts',(0.00174444656171948,-0.0205248063359435,
-0.0146166088785961));
#36044=CARTESIAN_POINT('Ctrl Pts',(0.00176030356309906,-0.0205258263477646,
-0.0146051974353997));
#36045=CARTESIAN_POINT('Ctrl Pts',(0.00178646731883081,-0.0205275381833709,
-0.014585978112248));
#36046=CARTESIAN_POINT('Ctrl Pts',(0.00179683736896153,-0.0205282243315903,
-0.0145782567956686));
#36047=CARTESIAN_POINT('Ctrl Pts',(0.00181661783993641,-0.0205295485289889,
-0.0145633289629271));
#36048=CARTESIAN_POINT('Ctrl Pts',(0.0018260360061562,-0.0205301857701985,
-0.0145561333071093));
#36049=CARTESIAN_POINT('Ctrl Pts',(0.00185172684373345,-0.0205319420189543,
-0.0145362628159982));
#36050=CARTESIAN_POINT('Ctrl Pts',(0.00186791154304711,-0.020533068386712,
-0.0145234758863733));
#36051=CARTESIAN_POINT('Ctrl Pts',(0.00193347393326414,-0.0205377088933039,
-0.0144705702996683));
#36052=CARTESIAN_POINT('Ctrl Pts',(0.00198169872866843,-0.0205413045442231,
-0.0144290547277521));
#36053=CARTESIAN_POINT('Ctrl Pts',(0.0021515462439045,-0.0205545365781522,
-0.0142731645081597));
#36054=CARTESIAN_POINT('Ctrl Pts',(0.00226489024162764,-0.0205644596693824,
-0.014150223232666));
#36055=CARTESIAN_POINT('Ctrl Pts',(0.00243512801042965,-0.0205806659576667,
-0.0139315023930857));
#36056=CARTESIAN_POINT('Ctrl Pts',(0.00249799485177614,-0.0205870334287672,
-0.0138408389070902));
#36057=CARTESIAN_POINT('Ctrl Pts',(0.00259371944215801,-0.020597329027143,
-0.013685118419402));
#36058=CARTESIAN_POINT('Ctrl Pts',(0.00262945491167657,-0.0206013442807375,
-0.013621961810522));
#36059=CARTESIAN_POINT('Ctrl Pts',(0.00267678423629044,-0.0206069198293628,
-0.0135307477982825));
#36060=CARTESIAN_POINT('Ctrl Pts',(0.0026902950449282,-0.0206085453180598,
-0.0135037183578124));
#36061=CARTESIAN_POINT('Ctrl Pts',(0.00271310037616789,-0.0206113506516388,
-0.0134563170420844));
#36062=CARTESIAN_POINT('Ctrl Pts',(0.00272257930431704,-0.020612536715622,
-0.013436037022608));
#36063=CARTESIAN_POINT('Ctrl Pts',(0.00274173307154,-0.0206149765057216,
-0.0133938327297171));
#36064=CARTESIAN_POINT('Ctrl Pts',(0.00275137401338352,-0.0206162290252235,
-0.0133718947748602));
#36065=CARTESIAN_POINT('Ctrl Pts',(0.00277578660096375,-0.0206194674023976,
-0.0133144862066364));
#36066=CARTESIAN_POINT('Ctrl Pts',(0.00279014171648493,-0.0206214393872089,
-0.0132788426576845));
#36067=CARTESIAN_POINT('Ctrl Pts',(0.00286190338657024,-0.0206316848528137,
-0.0130902849029507));
#36068=CARTESIAN_POINT('Ctrl Pts',(0.0029074389690806,-0.0206395665137156,
-0.0129331391784095));
#36069=CARTESIAN_POINT('Ctrl Pts',(0.00297156808176349,-0.02065488406393,
-0.0126174405475281));
#36070=CARTESIAN_POINT('Ctrl Pts',(0.00299077219366521,-0.0206623069356738,
-0.0124595664868214));
#36071=CARTESIAN_POINT('Ctrl Pts',(0.00299944094061995,-0.0206724806131768,
-0.0122518137264891));
#36072=CARTESIAN_POINT('Ctrl Pts',(0.00300028278161035,-0.0206749181885004,
-0.0122026632409654));
#36073=CARTESIAN_POINT('Ctrl Pts',(0.00299965846296588,-0.0206791606015538,
-0.0121188151077759));
#36074=CARTESIAN_POINT('Ctrl Pts',(0.00299879800491358,-0.0206809405146866,
-0.0120841222628853));
#36075=CARTESIAN_POINT('Ctrl Pts',(0.00299666157164527,-0.0206835854488807,
-0.0120334606865239));
#36076=CARTESIAN_POINT('Ctrl Pts',(0.00299585916587873,-0.0206844267587009,
-0.0120174737949181));
#36077=CARTESIAN_POINT('Ctrl Pts',(0.00299420640871956,-0.0206859337642829,
-0.0119890846979385));
#36078=CARTESIAN_POINT('Ctrl Pts',(0.00299340685696831,-0.0206865967291995,
-0.0119766802376367));
#36079=CARTESIAN_POINT('Ctrl Pts',(0.00299145005531643,-0.0206880861586951,
-0.011949002783292));
#36080=CARTESIAN_POINT('Ctrl Pts',(0.00299025293570462,-0.0206889146693103,
-0.0119337335957787));
#36081=CARTESIAN_POINT('Ctrl Pts',(0.00298627937454701,-0.0206914377598778,
-0.0118875886297702));
#36082=CARTESIAN_POINT('Ctrl Pts',(0.00298314129640574,-0.0206931501958046,
-0.0118567469187812));
#36083=CARTESIAN_POINT('Ctrl Pts',(0.0029631186028233,-0.0207027414972802,
-0.0116862428268249));
#36084=CARTESIAN_POINT('Ctrl Pts',(0.00293690505829126,-0.0207109809644874,
-0.0115478618239667));
#36085=CARTESIAN_POINT('Ctrl Pts',(0.00286849300119061,-0.0207267744796425,
-0.0112880893931355));
#36086=CARTESIAN_POINT('Ctrl Pts',(0.00282801573819313,-0.0207343075714324,
-0.0111665432863211));
#36087=CARTESIAN_POINT('Ctrl Pts',(0.00275095547654377,-0.0207461083871148,
-0.0109766159551572));
#36088=CARTESIAN_POINT('Ctrl Pts',(0.00271927640245593,-0.0207504786362945,
-0.0109064190280484));
#36089=CARTESIAN_POINT('Ctrl Pts',(0.00265966502553371,-0.0207579216449709,
-0.0107868286874288));
#36090=CARTESIAN_POINT('Ctrl Pts',(0.00263296872806532,-0.0207610307250221,
-0.0107368662649599));
#36091=CARTESIAN_POINT('Ctrl Pts',(0.00259119171484513,-0.0207655816225221,
-0.0106637401541188));
#36092=CARTESIAN_POINT('Ctrl Pts',(0.0025771808929533,-0.0207670602738008,
-0.010639982412334));
#36093=CARTESIAN_POINT('Ctrl Pts',(0.00255137322697377,-0.0207697010359709,
-0.0105975688924264));
#36094=CARTESIAN_POINT('Ctrl Pts',(0.00253969447675147,-0.0207708672591209,
-0.0105788439028333));
#36095=CARTESIAN_POINT('Ctrl Pts',(0.00251416618964412,-0.0207733564043156,
-0.0105389017805349));
#36096=CARTESIAN_POINT('Ctrl Pts',(0.00250025228299103,-0.0207746768609968,
-0.0105177277077988));
#36097=CARTESIAN_POINT('Ctrl Pts',(0.00246153296909395,-0.0207782561566436,
-0.0104604007090515));
#36098=CARTESIAN_POINT('Ctrl Pts',(0.00243620021526385,-0.0207804954096929,
-0.0104246106242727));
#36099=CARTESIAN_POINT('Ctrl Pts',(0.00227740445250603,-0.0207939546857506,
-0.0102103819121834));
#36100=CARTESIAN_POINT('Ctrl Pts',(0.00212519094255011,-0.0208044110159279,
-0.0100467173973649));
#36101=CARTESIAN_POINT('Ctrl Pts',(0.00187603371900854,-0.0208200099993034,
-0.00983241741400301));
#36102=CARTESIAN_POINT('Ctrl Pts',(0.00179222995620551,-0.0208250605404119,
-0.00976772046284651));
#36103=CARTESIAN_POINT('Ctrl Pts',(0.00165733134163275,-0.020833168007507,
-0.00967452637443893));
#36104=CARTESIAN_POINT('Ctrl Pts',(0.00160852474342964,-0.020836097618851,
-0.00964286476406511));
#36105=CARTESIAN_POINT('Ctrl Pts',(0.00154224646274915,-0.0208401129327455,
-0.00960255721782676));
#36106=CARTESIAN_POINT('Ctrl Pts',(0.00152556406545788,-0.0208411266375725,
-0.00959263222495757));
#36107=CARTESIAN_POINT('Ctrl Pts',(0.00149763342765964,-0.0208428308446952,
-0.00957638014054555));
#36108=CARTESIAN_POINT('Ctrl Pts',(0.00148643825423223,-0.020843515780168,
-0.00956996230039344));
#36109=CARTESIAN_POINT('Ctrl Pts',(0.00146485784422212,-0.020844840283607,
-0.00955777524634868));
#36110=CARTESIAN_POINT('Ctrl Pts',(0.00145447917651087,-0.0208454790753456,
-0.00955199516466442));
#36111=CARTESIAN_POINT('Ctrl Pts',(0.00142586328161577,-0.0208472446804427,
-0.00953628036724891));
#36112=CARTESIAN_POINT('Ctrl Pts',(0.00140755711420797,-0.020848378981683,
-0.00952647331817275));
#36113=CARTESIAN_POINT('Ctrl Pts',(0.0013315541525163,-0.0208531034472814,
-0.00948676675088753));
#36114=CARTESIAN_POINT('Ctrl Pts',(0.00127299825484383,-0.0208567787432643,
-0.00945855735008313));
#36115=CARTESIAN_POINT('Ctrl Pts',(0.00106184419740905,-0.02087004091851,
-0.00936515687992956));
#36116=CARTESIAN_POINT('Ctrl Pts',(0.000904808406850817,-0.0208799028571829,
-0.00931074453435733));
#36117=CARTESIAN_POINT('Ctrl Pts',(0.000597498983964137,-0.0208984491060018,
-0.00923206492601655));
#36118=CARTESIAN_POINT('Ctrl Pts',(0.000448273629090484,-0.0209071353400333,
-0.00920567567001786));
#36119=CARTESIAN_POINT('Ctrl Pts',(0.000252605066647527,-0.0209179846881952,
-0.00918616391769422));
#36120=CARTESIAN_POINT('Ctrl Pts',(0.000207433800087171,-0.0209204537919721,
-0.00918269051722269));
#36121=CARTESIAN_POINT('Ctrl Pts',(0.000136850255024302,-0.0209242579269562,
-0.00917886872314797));
#36122=CARTESIAN_POINT('Ctrl Pts',(0.000111484155088653,-0.0209256142168391,
-0.00917781796280831));
#36123=CARTESIAN_POINT('Ctrl Pts',(6.40541183576163E-5,-0.0209281307089639,
-0.00917645604533503));
#36124=CARTESIAN_POINT('Ctrl Pts',(4.19943152725023E-5,-0.0209292932507632,
-0.0091760660852877));
#36125=CARTESIAN_POINT('Ctrl Pts',(-7.57507594749086E-6,-0.0209318886048304,
-0.00917573674204599));
#36126=CARTESIAN_POINT('Ctrl Pts',(-3.5083739688327E-5,-0.0209333171846789,
-0.00917593231115193));
#36127=CARTESIAN_POINT('Ctrl Pts',(-0.000106187070892492,-0.0209369816788542,
-0.00917741600201071));
#36128=CARTESIAN_POINT('Ctrl Pts',(-0.000149763941693255,-0.0209392001892945,
-0.0091792764321678));
#36129=CARTESIAN_POINT('Ctrl Pts',(-0.000428410252006269,-0.0209532404945661,
-0.00919726663890821));
#36130=CARTESIAN_POINT('Ctrl Pts',(-0.000660920002255194,-0.0209642090100372,
-0.0092400904908678));
#36131=CARTESIAN_POINT('Ctrl Pts',(-0.00101503623141154,-0.0209818633078989,
-0.00934955999582587));
#36132=CARTESIAN_POINT('Ctrl Pts',(-0.00114118855565647,-0.0209883789393967,
-0.00939809988093033));
#36133=CARTESIAN_POINT('Ctrl Pts',(-0.00128551591720627,-0.0209965474965692,
-0.00946512807873946));
#36134=CARTESIAN_POINT('Ctrl Pts',(-0.00130727813672281,-0.0209977992555091,
-0.00947555587172245));
#36135=CARTESIAN_POINT('Ctrl Pts',(-0.0013413829062071,-0.0209997963558616,
-0.00949240673324522));
#36136=CARTESIAN_POINT('Ctrl Pts',(-0.00135381103275982,-0.0210005316270779,
-0.00949865527783052));
#36137=CARTESIAN_POINT('Ctrl Pts',(-0.00137738844339629,-0.0210019416829354,
-0.00951071555053032));
#36138=CARTESIAN_POINT('Ctrl Pts',(-0.00138854531996769,-0.021002615528051,
-0.00951651127214551));
#36139=CARTESIAN_POINT('Ctrl Pts',(-0.0014132828749569,-0.0210041238950519,
-0.00952955992511013));
#36140=CARTESIAN_POINT('Ctrl Pts',(-0.00142684481116017,-0.0210049604700519,
-0.00953684762070687));
#36141=CARTESIAN_POINT('Ctrl Pts',(-0.00147349547495861,-0.0210078699817501,
-0.00956238072356904));
#36142=CARTESIAN_POINT('Ctrl Pts',(-0.00150629405645,-0.0210099713015423,
-0.0095811460362178));
#36143=CARTESIAN_POINT('Ctrl Pts',(-0.00170029169243828,-0.0210226977382789,
-0.00969705730843852));
#36144=CARTESIAN_POINT('Ctrl Pts',(-0.0018524058701787,-0.0210338956861871,
-0.00980857451044751));
#36145=CARTESIAN_POINT('Ctrl Pts',(-0.00210317848294954,-0.0210535572724552,
-0.0100314779950751));
#36146=CARTESIAN_POINT('Ctrl Pts',(-0.00220594287360274,-0.0210620658274687,
-0.0101373417623571));
#36147=CARTESIAN_POINT('Ctrl Pts',(-0.00233629980723495,-0.0210733709046007,
-0.0102930865035584));
#36148=CARTESIAN_POINT('Ctrl Pts',(-0.0023708823466686,-0.0210764296494589,
-0.0103368250088186));
#36149=CARTESIAN_POINT('Ctrl Pts',(-0.00242062610603733,-0.0210809225126571,
-0.0104034760853746));
#36150=CARTESIAN_POINT('Ctrl Pts',(-0.00243672300396489,-0.0210823921058821,
-0.0104256725078518));
#36151=CARTESIAN_POINT('Ctrl Pts',(-0.00246521625306922,-0.0210850231150675,
-0.0104661178417662));
#36152=CARTESIAN_POINT('Ctrl Pts',(-0.0024777197584763,-0.021086188514531,
-0.0104842885379199));
#36153=CARTESIAN_POINT('Ctrl Pts',(-0.0025042180518513,-0.0210886827599708,
-0.0105237214006665));
#36154=CARTESIAN_POINT('Ctrl Pts',(-0.00251814498520116,-0.0210900090411845,
-0.0105450272059759));
#36155=CARTESIAN_POINT('Ctrl Pts',(-0.00255561025165671,-0.0210936216693006,
-0.0106039670403765));
#36156=CARTESIAN_POINT('Ctrl Pts',(-0.00257858757427925,-0.0210958877947361,
-0.0106419509078619));
#36157=CARTESIAN_POINT('Ctrl Pts',(-0.00270909250784214,-0.0211090949608693,
-0.0108689144046996));
#36158=CARTESIAN_POINT('Ctrl Pts',(-0.00279666020176482,-0.0211193162988675,
-0.0110686176684838));
#36159=CARTESIAN_POINT('Ctrl Pts',(-0.00289455212634948,-0.0211347996494708,
-0.0113799666564299));
#36160=CARTESIAN_POINT('Ctrl Pts',(-0.00292154022871089,-0.021139991958695,
-0.0114855868122083));
#36161=CARTESIAN_POINT('Ctrl Pts',(-0.00295423467757847,-0.0211482982237187,
-0.0116504952620033));
#36162=CARTESIAN_POINT('Ctrl Pts',(-0.00296402420910677,-0.021151277319334,
-0.0117088808654383));
#36163=CARTESIAN_POINT('Ctrl Pts',(-0.00297473803497446,-0.021155350702416,
-0.0117868610107671));
#36164=CARTESIAN_POINT('Ctrl Pts',(-0.00297720709618309,-0.0211563703266816,
-0.0118062328936693));
#36165=CARTESIAN_POINT('Ctrl Pts',(-0.00298099596312594,-0.0211580816931108,
-0.0118384659940107));
#36166=CARTESIAN_POINT('Ctrl Pts',(-0.00298242211488947,-0.0211587677664061,
-0.011851314474669));
#36167=CARTESIAN_POINT('Ctrl Pts',(-0.0029849967411681,-0.0211600919805377,
-0.0118759616797686));
#36168=CARTESIAN_POINT('Ctrl Pts',(-0.00298615840161401,-0.0211607293153368,
-0.0118877586641524));
#36169=CARTESIAN_POINT('Ctrl Pts',(-0.002989150519189,-0.0211624861302781,
-0.0119201093193191));
#36170=CARTESIAN_POINT('Ctrl Pts',(-0.00299083884355015,-0.0211636129783424,
-0.0119406751235815));
#36171=CARTESIAN_POINT('Ctrl Pts',(-0.00299687158423067,-0.0211682584856751,
-0.0120247948753659));
#36172=CARTESIAN_POINT('Ctrl Pts',(-0.00299940312266734,-0.0211718588700796,
-0.0120884587491634));
#36173=CARTESIAN_POINT('Ctrl Pts',(-0.00300122478128989,-0.0211850926846474,
-0.0123190145293164));
#36174=CARTESIAN_POINT('Ctrl Pts',(-0.00298861888737859,-0.0211950121219328,
-0.0124856941718688));
#36175=CARTESIAN_POINT('Ctrl Pts',(-0.00294478445964149,-0.021211213351149,
-0.0127592840504605));
#36176=CARTESIAN_POINT('Ctrl Pts',(-0.00292136378111559,-0.0212175793809198,
-0.0128670723621105));
#36177=CARTESIAN_POINT('Ctrl Pts',(-0.00287278238565809,-0.021227872998984,
-0.0130432526598134));
#36178=CARTESIAN_POINT('Ctrl Pts',(-0.00285097235238797,-0.0212318876692016,
-0.0131124525409196));
#36179=CARTESIAN_POINT('Ctrl Pts',(-0.00281655284832227,-0.0212374625696946,
-0.0132092665366904));
#36180=CARTESIAN_POINT('Ctrl Pts',(-0.00280600194062214,-0.0212390879730306,
-0.0132375811673358));
#36181=CARTESIAN_POINT('Ctrl Pts',(-0.00278689265475383,-0.021241893208216,
-0.0132865874584071));
#36182=CARTESIAN_POINT('Ctrl Pts',(-0.00277852718755164,-0.0212430792579223,
-0.013307351308735));
#36183=CARTESIAN_POINT('Ctrl Pts',(-0.00276072713277685,-0.0212455190626807,
-0.0133501445134297));
#36184=CARTESIAN_POINT('Ctrl Pts',(-0.00275125940240042,-0.0212467716105276,
-0.0133721584029861));
#36185=CARTESIAN_POINT('Ctrl Pts',(-0.00272592604562911,-0.0212500101571559,
-0.0134291703209422));
#36186=CARTESIAN_POINT('Ctrl Pts',(-0.00270964976913099,-0.0212519822802417,
-0.0134639816550492));
#36187=CARTESIAN_POINT('Ctrl Pts',(-0.00262067485815676,-0.0212622309455375,
-0.013645124990929));
#36188=CARTESIAN_POINT('Ctrl Pts',(-0.00253677635653375,-0.0212701153474075,
-0.0137856572748455));
#36189=CARTESIAN_POINT('Ctrl Pts',(-0.00234962476401415,-0.0212854331205784,
-0.0140478743764583));
#36190=CARTESIAN_POINT('Ctrl Pts',(-0.00224729947677344,-0.0212928536601149,
-0.0141695533335899));
#36191=CARTESIAN_POINT('Ctrl Pts',(-0.00210132351848718,-0.0213030244664125,
-0.0143175476283018));
#36192=CARTESIAN_POINT('Ctrl Pts',(-0.0020659593705846,-0.0213054616750342,
-0.0143516810969872));
#36193=CARTESIAN_POINT('Ctrl Pts',(-0.00200422401679125,-0.021309703513845,
-0.0144084056512836));
#36194=CARTESIAN_POINT('Ctrl Pts',(-0.00197826927830292,-0.0213114832284217,
-0.0144314362355991));
#36195=CARTESIAN_POINT('Ctrl Pts',(-0.00193976699157837,-0.0213141279213132,
-0.0144644249421457));
#36196=CARTESIAN_POINT('Ctrl Pts',(-0.00192752908158028,-0.021314969194496,
-0.0144747416748173));
#36197=CARTESIAN_POINT('Ctrl Pts',(-0.00190564151295149,-0.021316476162103,
-0.0144928955708241));
#36198=CARTESIAN_POINT('Ctrl Pts',(-0.00189602484649981,-0.0213171391262862,
-0.0145007714131726));
#36199=CARTESIAN_POINT('Ctrl Pts',(-0.00187444928540479,-0.0213186285893507,
-0.0145182184331059));
#36200=CARTESIAN_POINT('Ctrl Pts',(-0.00186246597466497,-0.021319457134808,
-0.0145277578501826));
#36201=CARTESIAN_POINT('Ctrl Pts',(-0.00182600704438916,-0.0213219804386885,
-0.0145563279216827));
#36202=CARTESIAN_POINT('Ctrl Pts',(-0.00180130962606329,-0.0213236930573088,
-0.0145750708045668));
#36203=CARTESIAN_POINT('Ctrl Pts',(-0.00166246850104765,-0.0213333187042689,
-0.0146770851821278));
#36204=CARTESIAN_POINT('Ctrl Pts',(-0.00154284994277481,-0.021341595501662,
-0.0147525897628802));
#36205=CARTESIAN_POINT('Ctrl Pts',(-0.00123769929215294,-0.0213619560712537,
-0.0149163164100325));
#36206=CARTESIAN_POINT('Ctrl Pts',(-0.0010475461800233,-0.0213739865394142,
-0.0149944885071188));
#36207=CARTESIAN_POINT('Ctrl Pts',(-0.000796941372126417,-0.0213885390732949,
-0.0150686113769277));
#36208=CARTESIAN_POINT('Ctrl Pts',(-0.000742553655963941,-0.021391626836907,
-0.0150830477353186));
#36209=CARTESIAN_POINT('Ctrl Pts',(-0.000661011412830097,-0.0213961531723039,
-0.0151022539357962));
#36210=CARTESIAN_POINT('Ctrl Pts',(-0.000634147246587491,-0.0213976279996285,
-0.0151081926574016));
#36211=CARTESIAN_POINT('Ctrl Pts',(-0.000585797080727557,-0.021400253865997,
-0.0151181856329597));
#36212=CARTESIAN_POINT('Ctrl Pts',(-0.000564341511285612,-0.0214014091010214,
-0.0151223760760515));
#36213=CARTESIAN_POINT('Ctrl Pts',(-0.000517950754755852,-0.021403886070058,
-0.0151309112462756));
#36214=CARTESIAN_POINT('Ctrl Pts',(-0.000493002415159303,-0.0214052052205168,
-0.015135175708913));
#36215=CARTESIAN_POINT('Ctrl Pts',(-0.000424817909479392,-0.0214087770513755,
-0.0151459443924384));
#36216=CARTESIAN_POINT('Ctrl Pts',(-0.000381488031400211,-0.0214110102869559,
-0.0151518201144713));
#36217=CARTESIAN_POINT('Ctrl Pts',(-0.000115536105605697,-0.0214245212488271,
-0.0151819799918598));
#36218=CARTESIAN_POINT('Ctrl Pts',(0.00010909390890025,-0.0214350259731176,
-0.0151822219030969));
#36219=CARTESIAN_POINT('Ctrl Pts',(0.00043619871549183,-0.0214506497260402,
-0.0151458350794988));
#36220=CARTESIAN_POINT('Ctrl Pts',(0.00054003720482919,-0.0214556717306781,
-0.0151287194743732));
#36221=CARTESIAN_POINT('Ctrl Pts',(0.000699369742092979,-0.0214637390650677,
-0.0150937705616322));
#36222=CARTESIAN_POINT('Ctrl Pts',(0.00075560798319205,-0.0214666585768238,
-0.0150797153789685));
#36223=CARTESIAN_POINT('Ctrl Pts',(0.000830065265031124,-0.0214706620321117,
-0.0150587975330248));
#36224=CARTESIAN_POINT('Ctrl Pts',(0.000848678370577245,-0.0214716745158966,
-0.0150533732009282));
#36225=CARTESIAN_POINT('Ctrl Pts',(0.000879585921006186,-0.021473377248088,
-0.0150440399969895));
#36226=CARTESIAN_POINT('Ctrl Pts',(0.000891910421517026,-0.0214740619506699,
-0.0150402314378059));
#36227=CARTESIAN_POINT('Ctrl Pts',(0.000915542361791507,-0.0214753865219293,
-0.0150327613075562));
#36228=CARTESIAN_POINT('Ctrl Pts',(0.000926853228380179,-0.0214760256205961,
-0.0150291118342597));
#36229=CARTESIAN_POINT('Ctrl Pts',(0.000957894447307013,-0.0214777930729377,
-0.01501889227325));
#36230=CARTESIAN_POINT('Ctrl Pts',(0.000977578290467563,-0.021478928939772,
-0.0150121842070055));
#36231=CARTESIAN_POINT('Ctrl Pts',(0.00105873833926493,-0.0214836703250271,
-0.0149835804509855));
#36232=CARTESIAN_POINT('Ctrl Pts',(0.00111955842974213,-0.021487361715491,
-0.0149598875027504));
#36233=CARTESIAN_POINT('Ctrl Pts',(0.00135038522493828,-0.0215017839381054,
-0.0148611800566739));
#36234=CARTESIAN_POINT('Ctrl Pts',(0.00151405971007277,-0.0215128631267645,
-0.0147724172285096));
#36235=CARTESIAN_POINT('Ctrl Pts',(0.00176702535379605,-0.0215305777122009,
-0.0146031323507912));
#36236=CARTESIAN_POINT('Ctrl Pts',(0.00186158798475756,-0.0215373627190307,
-0.0145313907886546));
#36237=CARTESIAN_POINT('Ctrl Pts',(0.00199176160682566,-0.0215468811248799,
-0.0144198839227839));
#36238=CARTESIAN_POINT('Ctrl Pts',(0.00203094853441844,-0.0215497731835642,
-0.0143844809876869));
#36239=CARTESIAN_POINT('Ctrl Pts',(0.00208863530351017,-0.0215540729979919,
-0.0143295302260942));
#36240=CARTESIAN_POINT('Ctrl Pts',(0.0021078388763649,-0.0215555118916898,
-0.0143107390272776));
#36241=CARTESIAN_POINT('Ctrl Pts',(0.00214081486899442,-0.0215579966934802,
-0.0142775923882731));
#36242=CARTESIAN_POINT('Ctrl Pts',(0.00215470152783834,-0.0215590475385496,
-0.0142633534437889));
#36243=CARTESIAN_POINT('Ctrl Pts',(0.00218577628607213,-0.0215614097863671,
-0.0142308498739207));
#36244=CARTESIAN_POINT('Ctrl Pts',(0.00220287912141226,-0.0215627175309422,
-0.0142125055821429));
#36245=CARTESIAN_POINT('Ctrl Pts',(0.00224844688518236,-0.0215662243281809,
-0.0141623845326164));
#36246=CARTESIAN_POINT('Ctrl Pts',(0.00227646782318025,-0.0215684051462365,
-0.0141302110496065));
#36247=CARTESIAN_POINT('Ctrl Pts',(0.00247375039618694,-0.0215839689152265,
-0.0138936898067993));
#36248=CARTESIAN_POINT('Ctrl Pts',(0.00261591545379976,-0.0215962035866839,
-0.0136682977111132));
#36249=CARTESIAN_POINT('Ctrl Pts',(0.00277112007888546,-0.0216140268087185,
-0.0133301033872699));
#36250=CARTESIAN_POINT('Ctrl Pts',(0.00281043785297068,-0.0216192232928378,
-0.0132307633683977));
#36251=CARTESIAN_POINT('Ctrl Pts',(0.00285347109973722,-0.0216261259518728,
-0.0131024176386094));
#36252=CARTESIAN_POINT('Ctrl Pts',(0.0028621787970604,-0.0216276025656415,
-0.0130751592611842));
#36253=CARTESIAN_POINT('Ctrl Pts',(0.00287480964959381,-0.0216298768994019,
-0.0130335769388411));
#36254=CARTESIAN_POINT('Ctrl Pts',(0.00287901876515703,-0.0216306593803561,
-0.0130193408779302));
#36255=CARTESIAN_POINT('Ctrl Pts',(0.00288656913398805,-0.0216321103404783,
-0.0129930889744409));
#36256=CARTESIAN_POINT('Ctrl Pts',(0.00288994135691478,-0.0216327770897573,
-0.0129810827391017));
#36257=CARTESIAN_POINT('Ctrl Pts',(0.0028975568477285,-0.0216343267955963,
-0.012953304927055));
#36258=CARTESIAN_POINT('Ctrl Pts',(0.00290174629040852,-0.0216352126465991,
-0.0129375193427555));
#36259=CARTESIAN_POINT('Ctrl Pts',(0.00291514339204965,-0.0216381569526274,
-0.0128853245039356));
#36260=CARTESIAN_POINT('Ctrl Pts',(0.00292379595731421,-0.0216402429176858,
-0.0128487777651147));
#36261=CARTESIAN_POINT('Ctrl Pts',(0.00297190863058026,-0.0216530045343649,
-0.0126270724928342));
#36262=CARTESIAN_POINT('Ctrl Pts',(0.00299445353082488,-0.0216642686155563,
-0.0124386886723795));
#36263=CARTESIAN_POINT('Ctrl Pts',(0.0030027274638194,-0.0216840355884287,
-0.0121015036464619));
#36264=CARTESIAN_POINT('Ctrl Pts',(0.00299540642979166,-0.021692583502484,
-0.0119534829003213));
#36265=CARTESIAN_POINT('Ctrl Pts',(0.00297033202492817,-0.0217039223733126,
-0.0117513181493819));
#36266=CARTESIAN_POINT('Ctrl Pts',(0.00296193783075799,-0.0217069785122006,
-0.0116962417083047));
#36267=CARTESIAN_POINT('Ctrl Pts',(0.00294713196708965,-0.0217114683674922,
-0.0116144582447007));
#36268=CARTESIAN_POINT('Ctrl Pts',(0.00294187989719302,-0.0217129374890491,
-0.011587555774586));
#36269=CARTESIAN_POINT('Ctrl Pts',(0.002931737491046,-0.0217155679921089,
-0.0115391416372691));
#36270=CARTESIAN_POINT('Ctrl Pts',(0.00292697722321101,-0.0217167333504085,
-0.0115176049972699));
#36271=CARTESIAN_POINT('Ctrl Pts',(0.00291621147847062,-0.0217192278702063,
-0.0114713259624122));
#36272=CARTESIAN_POINT('Ctrl Pts',(0.00291012764128102,-0.0217205544616695,
-0.0114466034657669));
#36273=CARTESIAN_POINT('Ctrl Pts',(0.00289256829316838,-0.0217241688677026,
-0.011378971000477));
#36274=CARTESIAN_POINT('Ctrl Pts',(0.00288045321620186,-0.0217264364266493,
-0.0113362329946691));
#36275=CARTESIAN_POINT('Ctrl Pts',(0.00280355853226712,-0.0217396288571486,
-0.0110862686529421));
#36276=CARTESIAN_POINT('Ctrl Pts',(0.00271738883586907,-0.0217498365236231,
-0.0108863027527758));
#36277=CARTESIAN_POINT('Ctrl Pts',(0.0025566054011644,-0.0217653133966032,
-0.0106024248559886));
#36278=CARTESIAN_POINT('Ctrl Pts',(0.00249768783074411,-0.0217705141299547,
-0.0105104820760344));
#36279=CARTESIAN_POINT('Ctrl Pts',(0.002399256479319,-0.0217788321778329,
-0.0103738879571371));
#36280=CARTESIAN_POINT('Ctrl Pts',(0.00236320185483031,-0.021781814178055,
-0.0103268571094016));
#36281=CARTESIAN_POINT('Ctrl Pts',(0.00231344136213341,-0.0217858909679136,
-0.0102657824247298));
#36282=CARTESIAN_POINT('Ctrl Pts',(0.00230095463788213,-0.0217869109363552,
-0.0102507586528688));
#36283=CARTESIAN_POINT('Ctrl Pts',(0.00227996183846282,-0.0217886227194699,
-0.0102259965822281));
#36284=CARTESIAN_POINT('Ctrl Pts',(0.00227153770091601,-0.0217893088593279,
-0.0102161891265516));
#36285=CARTESIAN_POINT('Ctrl Pts',(0.00225526953057183,-0.0217906330585487,
-0.0101974954244839));
#36286=CARTESIAN_POINT('Ctrl Pts',(0.002247435789575,-0.0217912703101578,
-0.0101886006986672));
#36287=CARTESIAN_POINT('Ctrl Pts',(0.00222582488967767,-0.0217930266221008,
-0.0101643540818985));
#36288=CARTESIAN_POINT('Ctrl Pts',(0.00221194201716796,-0.0217941530435087,
-0.010149097762112));
#36289=CARTESIAN_POINT('Ctrl Pts',(0.00215459533492618,-0.0217987941089578,
-0.0100873687365295));
#36290=CARTESIAN_POINT('Ctrl Pts',(0.00210981782575442,-0.0218023902888924,
-0.0100421437281432));
#36291=CARTESIAN_POINT('Ctrl Pts',(0.00194248262051159,-0.021815622521921,
-0.00988355649016529));
#36292=CARTESIAN_POINT('Ctrl Pts',(0.00181195642250678,-0.0218255452048675,
-0.00977904788177661));
#36293=CARTESIAN_POINT('Ctrl Pts',(0.00158192632857605,-0.0218417509279117,
-0.0096244496106172));
#36294=CARTESIAN_POINT('Ctrl Pts',(0.00148710991988152,-0.0218481182380285,
-0.00956804598993847));
#36295=CARTESIAN_POINT('Ctrl Pts',(0.00132510879460373,-0.0218584136150603,
-0.00948339190283278));
#36296=CARTESIAN_POINT('Ctrl Pts',(0.00125961949759353,-0.0218624288033541,
-0.00945213862613759));
#36297=CARTESIAN_POINT('Ctrl Pts',(0.00116533420114157,-0.0218680042792457,
-0.00941127209320417));
#36298=CARTESIAN_POINT('Ctrl Pts',(0.00113743024086137,-0.0218696297582169,
-0.00939967506590343));
#36299=CARTESIAN_POINT('Ctrl Pts',(0.00108855702388138,-0.0218724350804154,
-0.00938022371796871));
#36300=CARTESIAN_POINT('Ctrl Pts',(0.00106766656590156,-0.0218736211426054,
-0.0093721790509184));
#36301=CARTESIAN_POINT('Ctrl Pts',(0.00102423166521441,-0.0218760609338708,
-0.00935600867056513));
#36302=CARTESIAN_POINT('Ctrl Pts',(0.00100167593238024,-0.0218773134562668,
-0.00934791772636746));
#36303=CARTESIAN_POINT('Ctrl Pts',(0.000942707344764414,-0.0218805518515019,
-0.009327559224151));
#36304=CARTESIAN_POINT('Ctrl Pts',(0.000906150956446747,-0.0218825238511704,
-0.00931571923059809));
#36305=CARTESIAN_POINT('Ctrl Pts',(0.000713049804537019,-0.0218927696662601,
-0.00925725116838311));
#36306=CARTESIAN_POINT('Ctrl Pts',(0.000553109596414376,-0.0219006516266715,
-0.00922276080093842));
#36307=CARTESIAN_POINT('Ctrl Pts',(0.000233712367778685,-0.0219159692029597,
-0.00918075848110149));
#36308=CARTESIAN_POINT('Ctrl Pts',(7.48903184489933E-5,-0.0219233918215225,
-0.00917258820905025));
#36309=CARTESIAN_POINT('Ctrl Pts',(-0.000132955502815853,-0.0219335651874415,
-0.00917839791636385));
#36310=CARTESIAN_POINT('Ctrl Pts',(-0.00018204457507849,-0.0219360027229384,
-0.00918097845890368));
#36311=CARTESIAN_POINT('Ctrl Pts',(-0.000265644717133675,-0.0219402450735879,
-0.00918743612987579));
#36312=CARTESIAN_POINT('Ctrl Pts',(-0.000300193144802116,-0.0219420249651103,
-0.00919070871709235));
#36313=CARTESIAN_POINT('Ctrl Pts',(-0.000350582718806955,-0.0219446698729446,
-0.00919636541408512));
#36314=CARTESIAN_POINT('Ctrl Pts',(-0.000366474935124503,-0.0219455111786728,
-0.00919827837994413));
#36315=CARTESIAN_POINT('Ctrl Pts',(-0.000394680110815065,-0.0219470181799374,
-0.00920190269286606));
#36316=CARTESIAN_POINT('Ctrl Pts',(-0.000406998854596002,-0.0219476811446947,
-0.00920356352157882));
#36317=CARTESIAN_POINT('Ctrl Pts',(-0.000434473099811644,-0.0219491705776657,
-0.00920744163858167));
#36318=CARTESIAN_POINT('Ctrl Pts',(-0.000449622029310982,-0.021949999091974,
-0.00920969843609453));
#36319=CARTESIAN_POINT('Ctrl Pts',(-0.000495379012331518,-0.0219525222051482,
-0.00921687361943071));
#36320=CARTESIAN_POINT('Ctrl Pts',(-0.000525927913363199,-0.0219542346604364,
-0.00922215040384301));
#36321=CARTESIAN_POINT('Ctrl Pts',(-0.000698268341881028,-0.0219640330920767,
-0.00925467744159176));
#36322=CARTESIAN_POINT('Ctrl Pts',(-0.000838020304194822,-0.0219724991807633,
-0.00929166136062239));
#36323=CARTESIAN_POINT('Ctrl Pts',(-0.00112197445151132,-0.0219901538864227,
-0.00938919404126638));
#36324=CARTESIAN_POINT('Ctrl Pts',(-0.00126523405204063,-0.0219993148720676,
-0.00945124579585816));
#36325=CARTESIAN_POINT('Ctrl Pts',(-0.00145641618585282,-0.0220116177100778,
-0.00955240137190435));
#36326=CARTESIAN_POINT('Ctrl Pts',(-0.00150893992611529,-0.0220150087000287,
-0.00958225558945518));
#36327=CARTESIAN_POINT('Ctrl Pts',(-0.00160096939735291,-0.0220209650181399,
-0.00963830740734429));
#36328=CARTESIAN_POINT('Ctrl Pts',(-0.0016408224100256,-0.0220235496703174,
-0.00966389304307682));
#36329=CARTESIAN_POINT('Ctrl Pts',(-0.00170143074430163,-0.022027490017923,
-0.00970486175621376));
#36330=CARTESIAN_POINT('Ctrl Pts',(-0.0017226199654381,-0.0220288695109033,
-0.00971958656005426));
#36331=CARTESIAN_POINT('Ctrl Pts',(-0.00176154538277091,-0.0220314079841257,
-0.00974738808106528));
#36332=CARTESIAN_POINT('Ctrl Pts',(-0.0017793324229179,-0.0220325696500739,
-0.00976039027645391));
#36333=CARTESIAN_POINT('Ctrl Pts',(-0.00181857258874413,-0.0220351369951552,
-0.00978974322909495));
#36334=CARTESIAN_POINT('Ctrl Pts',(-0.00183995181243218,-0.0220365388692148,
-0.00980618983867333));
#36335=CARTESIAN_POINT('Ctrl Pts',(-0.00189385431099838,-0.0220400834199648,
-0.00984882531421506));
#36336=CARTESIAN_POINT('Ctrl Pts',(-0.00192605841184427,-0.0220422106275502,
-0.00987540929877964));
#36337=CARTESIAN_POINT('Ctrl Pts',(-0.00210026431969435,-0.0220537927483132,
-0.0100254371190867));
#36338=CARTESIAN_POINT('Ctrl Pts',(-0.00223097199378551,-0.0220627306866264,
-0.0101613629732309));
#36339=CARTESIAN_POINT('Ctrl Pts',(-0.00242805632135967,-0.0220777329034768,
-0.0104092038783085));
#36340=CARTESIAN_POINT('Ctrl Pts',(-0.00250147726794621,-0.0220838043314496,
-0.010514794645838));
#36341=CARTESIAN_POINT('Ctrl Pts',(-0.00259072448680345,-0.0220922945642758,
-0.0106625471479935));
#36342=CARTESIAN_POINT('Ctrl Pts',(-0.00261271141670614,-0.0220944945843775,
-0.0107008320724447));
#36343=CARTESIAN_POINT('Ctrl Pts',(-0.00264919515476018,-0.0220983627385461,
-0.0107677364301181));
#36344=CARTESIAN_POINT('Ctrl Pts',(-0.00266409274639131,-0.0221000114360775,
-0.0107961294979881));
#36345=CARTESIAN_POINT('Ctrl Pts',(-0.00268552129340751,-0.0221024965732946,
-0.0108386112601502));
#36346=CARTESIAN_POINT('Ctrl Pts',(-0.00269240296945313,-0.0221033131810294,
-0.0108525214747711));
#36347=CARTESIAN_POINT('Ctrl Pts',(-0.00270406198285871,-0.022104730099961,
-0.0108765557455737));
#36348=CARTESIAN_POINT('Ctrl Pts',(-0.00270889105787199,-0.0221053272852062,
-0.010886654102348));
#36349=CARTESIAN_POINT('Ctrl Pts',(-0.00272012001133121,-0.0221067405482624,
-0.0109104772793919));
#36350=CARTESIAN_POINT('Ctrl Pts',(-0.00272647247867412,-0.0221075593571746,
-0.0109242235014021));
#36351=CARTESIAN_POINT('Ctrl Pts',(-0.00274514505802295,-0.0221100234681322,
-0.0109654461876865));
#36352=CARTESIAN_POINT('Ctrl Pts',(-0.00275715551332704,-0.0221116854769967,
-0.010993059951077));
#36353=CARTESIAN_POINT('Ctrl Pts',(-0.00283612734214268,-0.0221231336134954,
-0.0111823692331312));
#36354=CARTESIAN_POINT('Ctrl Pts',(-0.00288923950074892,-0.0221334843104636,
-0.0113494656580827));
#36355=CARTESIAN_POINT('Ctrl Pts',(-0.00295710066008395,-0.0221517345325836,
-0.0116524764824545));
#36356=CARTESIAN_POINT('Ctrl Pts',(-0.00297772528765525,-0.0221596437306527,
-0.0117865914270376));
#36357=CARTESIAN_POINT('Ctrl Pts',(-0.00299620029652009,-0.0221719987161479,
-0.0120038413913217));
#36358=CARTESIAN_POINT('Ctrl Pts',(-0.00299979743429729,-0.0221765855549523,
-0.0120862909117538));
#36359=CARTESIAN_POINT('Ctrl Pts',(-0.00300006613385393,-0.0221827892278334,
-0.0122004087489637));
#36360=CARTESIAN_POINT('Ctrl Pts',(-0.00299964069417185,-0.0221844929160432,
-0.0122320279070503));
#36361=CARTESIAN_POINT('Ctrl Pts',(-0.00299806021748773,-0.0221873769809811,
-0.0122860184767575));
#36362=CARTESIAN_POINT('Ctrl Pts',(-0.00299715438798948,-0.0221885648940955,
-0.0123083940273983));
#36363=CARTESIAN_POINT('Ctrl Pts',(-0.00299478752303314,-0.0221909808071725,
-0.0123541714208326));
#36364=CARTESIAN_POINT('Ctrl Pts',(-0.00299330250209953,-0.0221922079845099,
-0.0123775705072845));
#36365=CARTESIAN_POINT('Ctrl Pts',(-0.00298884842571801,-0.0221952941349685,
-0.0124367652798569));
#36366=CARTESIAN_POINT('Ctrl Pts',(-0.00298551052183768,-0.0221971416924579,
-0.012472529952921));
#36367=CARTESIAN_POINT('Ctrl Pts',(-0.00296771426552442,-0.0222053220867497,
-0.0126321697723249));
#36368=CARTESIAN_POINT('Ctrl Pts',(-0.00294618197791558,-0.0222114371849998,
-0.0127551360597183));
#36369=CARTESIAN_POINT('Ctrl Pts',(-0.00288909348363007,-0.0222231872977006,
-0.0129928459641426));
#36370=CARTESIAN_POINT('Ctrl Pts',(-0.00285418507381699,-0.0222288222154665,
-0.013107500304734));
#36371=CARTESIAN_POINT('Ctrl Pts',(-0.00276086151948031,-0.0222415624585182,
-0.0133589345842988));
#36372=CARTESIAN_POINT('Ctrl Pts',(-0.0026989510516914,-0.0222486784599728,
-0.0134940687630364));
#36373=CARTESIAN_POINT('Ctrl Pts',(-0.00261548014216787,-0.0222575493354705,
-0.0136455006917983));
#36374=CARTESIAN_POINT('Ctrl Pts',(-0.00260339506845473,-0.0222588192365489,
-0.0136668039611273));
#36375=CARTESIAN_POINT('Ctrl Pts',(-0.0025840005302212,-0.0222608387541011,
-0.0137000373043808));
#36376=CARTESIAN_POINT('Ctrl Pts',(-0.00257686589707012,-0.0222615779177206,
-0.0137120686990122));
#36377=CARTESIAN_POINT('Ctrl Pts',(-0.00256310140165208,-0.0222629977254138,
-0.0137349145765833));
#36378=CARTESIAN_POINT('Ctrl Pts',(-0.00255648670917778,-0.0222636774529654,
-0.0137457375452049));
#36379=CARTESIAN_POINT('Ctrl Pts',(-0.00254020917814553,-0.0222653434369309,
-0.0137719951758081));
#36380=CARTESIAN_POINT('Ctrl Pts',(-0.00253047412683002,-0.0222663341560335,
-0.0137873843163532));
#36381=CARTESIAN_POINT('Ctrl Pts',(-0.00249421876549608,-0.022270000568166,
-0.0138435581304638));
#36382=CARTESIAN_POINT('Ctrl Pts',(-0.00246684872924702,-0.0222727238273082,
-0.0138837828909727));
#36383=CARTESIAN_POINT('Ctrl Pts',(-0.00239207133013985,-0.0222800140460087,
-0.0139881313970417));
#36384=CARTESIAN_POINT('Ctrl Pts',(-0.00234306512956684,-0.0222846436701589,
-0.0140510604152399));
#36385=CARTESIAN_POINT('Ctrl Pts',(-0.00212251389387266,-0.0223046481960207,
-0.0143121091987214));
#36386=CARTESIAN_POINT('Ctrl Pts',(-0.00192788479875701,-0.0223201747986316,
-0.0144892833378718));
#36387=CARTESIAN_POINT('Ctrl Pts',(-0.00167708118250625,-0.0223370070963812,
-0.0146636796448001));
#36388=CARTESIAN_POINT('Ctrl Pts',(-0.00164093642426968,-0.0223393693352635,
-0.014687667212669));
#36389=CARTESIAN_POINT('Ctrl Pts',(-0.00158296019067432,-0.0223430605417988,
-0.0147243575108832));
#36390=CARTESIAN_POINT('Ctrl Pts',(-0.00156146768515415,-0.0223444083038223,
-0.014737582286195));
#36391=CARTESIAN_POINT('Ctrl Pts',(-0.00152104224537875,-0.0223469058372614,
-0.0147617590700424));
#36392=CARTESIAN_POINT('Ctrl Pts',(-0.00150215157867311,-0.0223480579621607,
-0.0147727781799165));
#36393=CARTESIAN_POINT('Ctrl Pts',(-0.00145913475852153,-0.0223506486410041,
-0.0147972438569291));
#36394=CARTESIAN_POINT('Ctrl Pts',(-0.00143493985121314,-0.0223520827399218,
-0.0148105658809706));
#36395=CARTESIAN_POINT('Ctrl Pts',(-0.00136039271092404,-0.0223564341551935,
-0.0148502809346667));
#36396=CARTESIAN_POINT('Ctrl Pts',(-0.00130947016684187,-0.0223593139268372,
-0.0148755791933653));
#36397=CARTESIAN_POINT('Ctrl Pts',(-0.00118760376923174,-0.0223660153684573,
-0.0149318622843445));
#36398=CARTESIAN_POINT('Ctrl Pts',(-0.00111611861718849,-0.0223697985100823,
-0.014961579134383));
#36399=CARTESIAN_POINT('Ctrl Pts',(-0.000923635682447565,-0.0223797014644557,
-0.0150329950647879));
#36400=CARTESIAN_POINT('Ctrl Pts',(-0.00080098508514844,-0.0223857198465289,
-0.0150697754669045));
#36401=CARTESIAN_POINT('Ctrl Pts',(-0.000539947572133343,-0.0223984430494374,
-0.0151301826462491));
#36402=CARTESIAN_POINT('Ctrl Pts',(-0.000401502187463013,-0.0224051445719702,
-0.0151521587846218));
#36403=CARTESIAN_POINT('Ctrl Pts',(-0.000231165498714199,-0.0224138358757515,
-0.0151670943760587));
#36404=CARTESIAN_POINT('Ctrl Pts',(-0.00020024913034703,-0.0224154313853954,
-0.0151693229937273));
#36405=CARTESIAN_POINT('Ctrl Pts',(-0.000154014054578636,-0.0224178515147535,
-0.0151719364345054));
#36406=CARTESIAN_POINT('Ctrl Pts',(-0.000138717090381707,-0.0224186577817739,
-0.0151726836300155));
#36407=CARTESIAN_POINT('Ctrl Pts',(-0.000110995066660502,-0.0224201300717305,
-0.0151738250378248));
#36408=CARTESIAN_POINT('Ctrl Pts',(-9.85723484036395E-5,-0.0224207939515171,
-0.0151742591971416));
#36409=CARTESIAN_POINT('Ctrl Pts',(-7.01456901468166E-5,-0.022422322497064,
-0.0151750758259489));
#36410=CARTESIAN_POINT('Ctrl Pts',(-5.41411408996982E-5,-0.0224231897987845,
-0.0151754074155413));
#36411=CARTESIAN_POINT('Ctrl Pts',(-3.43016299497264E-6,-0.0224259574924225,
-0.0151760520897919));
#36412=CARTESIAN_POINT('Ctrl Pts',(3.12783665409965E-5,-0.0224278808984236,
-0.0151758909675471));
#36413=CARTESIAN_POINT('Ctrl Pts',(0.000115125658412668,-0.0224325852705832,
-0.0151740465859631));
#36414=CARTESIAN_POINT('Ctrl Pts',(0.000164240481776405,-0.0224353889560151,
-0.015171757427574));
#36415=CARTESIAN_POINT('Ctrl Pts',(0.000371733148112998,-0.0224473794009763,
-0.0151569690381535));
#36416=CARTESIAN_POINT('Ctrl Pts',(0.000529041856396036,-0.0224568150509789,
-0.0151331072210719));
#36417=CARTESIAN_POINT('Ctrl Pts',(0.000842667011886648,-0.0224756435907731,
-0.0150596980503088));
#36418=CARTESIAN_POINT('Ctrl Pts',(0.0009983284072594,-0.0224849933752691,
-0.0150095789023201));
#36419=CARTESIAN_POINT('Ctrl Pts',(0.00118464014059581,-0.0224960464107419,
-0.0149323190444764));
#36420=CARTESIAN_POINT('Ctrl Pts',(0.0012198405390155,-0.0224981295230377,
-0.0149169233298935));
#36421=CARTESIAN_POINT('Ctrl Pts',(0.00127650075573758,-0.0225014753064585,
-0.0148908339352574));
#36422=CARTESIAN_POINT('Ctrl Pts',(0.00129814439834198,-0.0225027516175345,
-0.0148805520254744));
#36423=CARTESIAN_POINT('Ctrl Pts',(0.00133976615710941,-0.022505203294868,
-0.0148601646965864));
#36424=CARTESIAN_POINT('Ctrl Pts',(0.00135975884324625,-0.0225063797011921,
-0.014850092809491));
#36425=CARTESIAN_POINT('Ctrl Pts',(0.00140647101227962,-0.0225091263036935,
-0.0148259009212793));
#36426=CARTESIAN_POINT('Ctrl Pts',(0.00143309381572103,-0.0225106900898947,
-0.0148115989828092));
#36427=CARTESIAN_POINT('Ctrl Pts',(0.00152289044467476,-0.0225159633104295,
-0.0147615968092931));
#36428=CARTESIAN_POINT('Ctrl Pts',(0.00158498533151552,-0.0225196068228695,
-0.0147240070075853));
#36429=CARTESIAN_POINT('Ctrl Pts',(0.00173787272045709,-0.0225286315201982,
-0.0146237016948439));
#36430=CARTESIAN_POINT('Ctrl Pts',(0.00182668324072589,-0.0225339220731381,
-0.0145581617647929));
#36431=CARTESIAN_POINT('Ctrl Pts',(0.00204043508879636,-0.0225471067924608,
-0.014381422086363));
#36432=CARTESIAN_POINT('Ctrl Pts',(0.00216005926051084,-0.0225549086665976,
-0.0142644046738105));
#36433=CARTESIAN_POINT('Ctrl Pts',(0.00231082028504639,-0.0225662505602816,
-0.0140900466921178));
#36434=CARTESIAN_POINT('Ctrl Pts',(0.00235078930311023,-0.0225694322918355,
-0.0140407434832586));
#36435=CARTESIAN_POINT('Ctrl Pts',(0.00240162659897542,-0.022573773316639,
-0.0139738005642736));
#36436=CARTESIAN_POINT('Ctrl Pts',(0.0024139209104093,-0.0225748475444231,
-0.0139572601820664));
#36437=CARTESIAN_POINT('Ctrl Pts',(0.00243301373169981,-0.0225765569991578,
-0.0139310127049008));
#36438=CARTESIAN_POINT('Ctrl Pts',(0.00243992701338234,-0.0225771847431408,
-0.013921389468448));
#36439=CARTESIAN_POINT('Ctrl Pts',(0.00245426591355026,-0.022578505809994,
-0.0139011782035867));
#36440=CARTESIAN_POINT('Ctrl Pts',(0.0024616803286926,-0.0225791999030353,
-0.0138905827648177));
#36441=CARTESIAN_POINT('Ctrl Pts',(0.002480131856961,-0.0225809544236205,
-0.0138638486210385));
#36442=CARTESIAN_POINT('Ctrl Pts',(0.00249108004436049,-0.0225820204401341,
-0.0138476494612212));
#36443=CARTESIAN_POINT('Ctrl Pts',(0.00253464584589147,-0.0225863609092288,
-0.0137818104555379));
#36444=CARTESIAN_POINT('Ctrl Pts',(0.0025659426011696,-0.0225897073016119,
-0.0137313164614743));
#36445=CARTESIAN_POINT('Ctrl Pts',(0.00265065524652938,-0.0225993744060296,
-0.0135851203895325));
#36446=CARTESIAN_POINT('Ctrl Pts',(0.00270035450372961,-0.0226058094553392,
-0.0134873755430876));
#36447=CARTESIAN_POINT('Ctrl Pts',(0.00283193651514683,-0.0226249749353865,
-0.0131892294871944));
#36448=CARTESIAN_POINT('Ctrl Pts',(0.00289762989870859,-0.0226376229889528,
-0.0129824276156023));
#36449=CARTESIAN_POINT('Ctrl Pts',(0.002949323349224,-0.0226520122311989,
-0.0127267349323925));
#36450=CARTESIAN_POINT('Ctrl Pts',(0.00295716772792673,-0.0226544368677631,
-0.0126829411705067));
#36451=CARTESIAN_POINT('Ctrl Pts',(0.00296796806537692,-0.0226582025795226,
-0.0126138195551786));
#36452=CARTESIAN_POINT('Ctrl Pts',(0.00297157994979023,-0.0226595637321218,
-0.0125886020549129));
#36453=CARTESIAN_POINT('Ctrl Pts',(0.00297771884988576,-0.0226620847460379,
-0.0125414717133667));
#36454=CARTESIAN_POINT('Ctrl Pts',(0.0029803262215699,-0.0226632470201509,
-0.0125195712387592));
#36455=CARTESIAN_POINT('Ctrl Pts',(0.00298562969415798,-0.0226658360833862,
-0.0124704130636376));
#36456=CARTESIAN_POINT('Ctrl Pts',(0.00298819450458233,-0.0226672587347878,
-0.0124431430168683));
#36457=CARTESIAN_POINT('Ctrl Pts',(0.0029948326521407,-0.0226715353304101,
-0.0123604278865456));
#36458=CARTESIAN_POINT('Ctrl Pts',(0.00299773879177757,-0.0226743536673376,
-0.0123048998635374));
#36459=CARTESIAN_POINT('Ctrl Pts',(0.003002749106918,-0.0226845779136009,
-0.0121003682146989));
#36460=CARTESIAN_POINT('Ctrl Pts',(0.00299529632880228,-0.022691709560899,
-0.0119513435583257));
#36461=CARTESIAN_POINT('Ctrl Pts',(0.0029531023130733,-0.022707838376723,
-0.0116140360066398));
#36462=CARTESIAN_POINT('Ctrl Pts',(0.00291137573080329,-0.0227167550548723,
-0.0114273017333655));
#36463=CARTESIAN_POINT('Ctrl Pts',(0.00284214618952716,-0.0227280377211407,
-0.01121499094986));
#36464=CARTESIAN_POINT('Ctrl Pts',(0.0028315952364804,-0.0227296968193252,
-0.0111843293811954));
#36465=CARTESIAN_POINT('Ctrl Pts',(0.00281514967861382,-0.0227322052645117,
-0.0111389427038347));
#36466=CARTESIAN_POINT('Ctrl Pts',(0.00280963164633446,-0.0227330350391886,
-0.0111240827506006));
#36467=CARTESIAN_POINT('Ctrl Pts',(0.00279948762523685,-0.0227345406621734,
-0.0110974146678914));
#36468=CARTESIAN_POINT('Ctrl Pts',(0.00279490395685265,-0.0227352141113977,
-0.0110855906179998));
#36469=CARTESIAN_POINT('Ctrl Pts',(0.00278521988879893,-0.0227366234938713,
-0.0110610719950753));
#36470=CARTESIAN_POINT('Ctrl Pts',(0.00278010743530948,-0.022737360072112,
-0.0110483827591145));
#36471=CARTESIAN_POINT('Ctrl Pts',(0.00276614362526174,-0.0227393513211228,
-0.0110143967265378));
#36472=CARTESIAN_POINT('Ctrl Pts',(0.00275713333421183,-0.0227406147655919,
-0.0109931666798029));
#36473=CARTESIAN_POINT('Ctrl Pts',(0.00270570164132528,-0.0227477023053815,
-0.0108757660176438));
#36474=CARTESIAN_POINT('Ctrl Pts',(0.0026584963238782,-0.0227537527298463,
-0.0107817794216991));
#36475=CARTESIAN_POINT('Ctrl Pts',(0.00250148702830404,-0.0227722598170136,
-0.0105062685323013));
#36476=CARTESIAN_POINT('Ctrl Pts',(0.00237726799819849,-0.0227848745162435,
-0.0103336908587693));
#36477=CARTESIAN_POINT('Ctrl Pts',(0.00217911778439241,-0.0228017556413523,
-0.0101121926451168));
#36478=CARTESIAN_POINT('Ctrl Pts',(0.00211967007436097,-0.0228065007385733,
-0.0100511767805065));
#36479=CARTESIAN_POINT('Ctrl Pts',(0.00203379013168693,-0.0228129266850183,
-0.00997022921803805));
#36480=CARTESIAN_POINT('Ctrl Pts',(0.00200950818109512,-0.0228146995771691,
-0.00994808381507069));
#36481=CARTESIAN_POINT('Ctrl Pts',(0.00196944927229389,-0.0228175548744493,
-0.00991273766544224));
#36482=CARTESIAN_POINT('Ctrl Pts',(0.00195389224793098,-0.0228186472542774,
-0.00989929275308995));
#36483=CARTESIAN_POINT('Ctrl Pts',(0.00192082308474554,-0.0228209353600627,
-0.00987130195295136));
#36484=CARTESIAN_POINT('Ctrl Pts',(0.00190328107853154,-0.0228221295486507,
-0.00985679327310194));
#36485=CARTESIAN_POINT('Ctrl Pts',(0.00186034961519805,-0.022825006151969,
-0.00982210071252365));
#36486=CARTESIAN_POINT('Ctrl Pts',(0.00183479442940087,-0.0228266802986708,
-0.00980212596924957));
#36487=CARTESIAN_POINT('Ctrl Pts',(0.0017380103619275,-0.0228328856380354,
-0.0097289735191961));
#36488=CARTESIAN_POINT('Ctrl Pts',(0.00166475097203775,-0.022837313136912,
-0.00967855343167439));
#36489=CARTESIAN_POINT('Ctrl Pts',(0.00145827531335508,-0.0228492092109301,
-0.00954957844397204));
#36490=CARTESIAN_POINT('Ctrl Pts',(0.00132105944640269,-0.022856480624913,
-0.00947794847188107));
#36491=CARTESIAN_POINT('Ctrl Pts',(0.00104442860403589,-0.0228707544211676,
-0.00935972736946574));
#36492=CARTESIAN_POINT('Ctrl Pts',(0.000905909573580902,-0.0228777362502304,
-0.00931216398627652));
#36493=CARTESIAN_POINT('Ctrl Pts',(0.000734529195063823,-0.0228867449418894,
-0.00926700010677626));
#36494=CARTESIAN_POINT('Ctrl Pts',(0.00070444943541359,-0.0228883398212591,
-0.00925956955350818));
#36495=CARTESIAN_POINT('Ctrl Pts',(0.00065934003519541,-0.0228907591794718,
-0.00924916485052493));
#36496=CARTESIAN_POINT('Ctrl Pts',(0.000644393129839122,-0.0228915653228285,
-0.00924583759409903));
#36497=CARTESIAN_POINT('Ctrl Pts',(0.000617267434001677,-0.0228930374964899,
-0.00924001687355079));
#36498=CARTESIAN_POINT('Ctrl Pts',(0.00060509771003202,-0.0228937013857558,
-0.00923748447434438));
#36499=CARTESIAN_POINT('Ctrl Pts',(0.000577217386921786,-0.022895230096769,
-0.00923186340251633));
#36500=CARTESIAN_POINT('Ctrl Pts',(0.000561497558760526,-0.0228960975568538,
-0.00922882481404518));
#36501=CARTESIAN_POINT('Ctrl Pts',(0.000511610527919068,-0.0228988662801009,
-0.00921959545242807));
#36502=CARTESIAN_POINT('Ctrl Pts',(0.000477360835994778,-0.0229007905804083,
-0.00921387216832633));
#36503=CARTESIAN_POINT('Ctrl Pts',(0.000394367173750417,-0.022905497614691,
-0.00920148032707446));
#36504=CARTESIAN_POINT('Ctrl Pts',(0.000345544041368787,-0.0229083030992029,
-0.00919541391209181));
#36505=CARTESIAN_POINT('Ctrl Pts',(0.000138308451148491,-0.0229203074734349,
-0.00917482461799437));
#36506=CARTESIAN_POINT('Ctrl Pts',(-2.09767918662082E-5,-0.0229297557057958,
-0.00917171251906662));
#36507=CARTESIAN_POINT('Ctrl Pts',(-0.000342466307622283,-0.0229485812984738,
-0.00919101044932174));
#36508=CARTESIAN_POINT('Ctrl Pts',(-0.000504126132214393,-0.0229579165995115,
-0.00921402295924528));
#36509=CARTESIAN_POINT('Ctrl Pts',(-0.000700588261347361,-0.022968955784303,
-0.00925855127254133));
#36510=CARTESIAN_POINT('Ctrl Pts',(-0.000737878009532388,-0.0229710383253205,
-0.00926775920595564));
#36511=CARTESIAN_POINT('Ctrl Pts',(-0.000798126993262842,-0.0229743834280791,
-0.00928387000461224));
#36512=CARTESIAN_POINT('Ctrl Pts',(-0.000821197557063287,-0.0229756596194627,
-0.00929033624143045));
#36513=CARTESIAN_POINT('Ctrl Pts',(-0.00086567022482869,-0.0229781112188349,
-0.0093033776640103));
#36514=CARTESIAN_POINT('Ctrl Pts',(-0.000887080988239808,-0.0229792876647352,
-0.0093099174016066));
#36515=CARTESIAN_POINT('Ctrl Pts',(-0.000937222337681476,-0.0229820345896755,
-0.00932584840906725));
#36516=CARTESIAN_POINT('Ctrl Pts',(-0.000965888416280869,-0.0229835986541698,
-0.0093354355066179));
#36517=CARTESIAN_POINT('Ctrl Pts',(-0.00106289789811331,-0.0229888740268977,
-0.00936951789488818));
#36518=CARTESIAN_POINT('Ctrl Pts',(-0.00113049717084552,-0.0229925193368616,
-0.00939606059001765));
#36519=CARTESIAN_POINT('Ctrl Pts',(-0.00129827759875929,-0.0230015499381171,
-0.00946907330223513));
#36520=CARTESIAN_POINT('Ctrl Pts',(-0.00139698078253561,-0.0230068444297298,
-0.00951866883164786));
#36521=CARTESIAN_POINT('Ctrl Pts',(-0.00163783387362543,-0.023020043552775,
-0.0096568289468316));
#36522=CARTESIAN_POINT('Ctrl Pts',(-0.00177571317877768,-0.0230278557468406,
-0.0097520505103187));
#36523=CARTESIAN_POINT('Ctrl Pts',(-0.00195372373463717,-0.0230391965145519,
-0.00989836499833351));
#36524=CARTESIAN_POINT('Ctrl Pts',(-0.00200123607809152,-0.0230423640171239,
-0.00993999941923989));
#36525=CARTESIAN_POINT('Ctrl Pts',(-0.00206243655992725,-0.0230466883961414,
-0.00999714291755532));
#36526=CARTESIAN_POINT('Ctrl Pts',(-0.00207733177614196,-0.0230477610313858,
-0.0100113403892821));
#36527=CARTESIAN_POINT('Ctrl Pts',(-0.00210056755779622,-0.0230494685627229,
-0.0100339484814817));
#36528=CARTESIAN_POINT('Ctrl Pts',(-0.00210900663111077,-0.0230500960049795,
-0.0100422574299579));
#36529=CARTESIAN_POINT('Ctrl Pts',(-0.00212656154367453,-0.0230514170883795,
-0.0100597475728918));
#36530=CARTESIAN_POINT('Ctrl Pts',(-0.00213566749634862,-0.023052111507196,
-0.0100689380732353));
#36531=CARTESIAN_POINT('Ctrl Pts',(-0.00215840453463852,-0.0230538679299092,
-0.0100921850649516));
#36532=CARTESIAN_POINT('Ctrl Pts',(-0.00217195786982498,-0.0230549355470293,
-0.0101063165354204));
#36533=CARTESIAN_POINT('Ctrl Pts',(-0.00222623725557716,-0.0230592917244094,
-0.0101640317718339));
#36534=CARTESIAN_POINT('Ctrl Pts',(-0.002265795476054,-0.0230626528545809,
-0.010208690836643));
#36535=CARTESIAN_POINT('Ctrl Pts',(-0.00237467881292944,-0.0230723812373582,
-0.0103392582024945));
#36536=CARTESIAN_POINT('Ctrl Pts',(-0.00244062978192046,-0.0230788643175511,
-0.0104278529158088));
#36537=CARTESIAN_POINT('Ctrl Pts',(-0.00262023135593886,-0.0230979995435695,
-0.0106991619459459));
#36538=CARTESIAN_POINT('Ctrl Pts',(-0.00271931457749544,-0.0231105669534358,
-0.0108907140410943));
#36539=CARTESIAN_POINT('Ctrl Pts',(-0.00281319465099427,-0.0231248916448978,
-0.0111328169037544));
#36540=CARTESIAN_POINT('Ctrl Pts',(-0.00282839011552863,-0.0231273227423607,
-0.0111747545481903));
#36541=CARTESIAN_POINT('Ctrl Pts',(-0.00285079489111302,-0.0231310961601406,
-0.0112411776012326));
#36542=CARTESIAN_POINT('Ctrl Pts',(-0.00285863616818458,-0.0231324586926874,
-0.0112654415883313));
#36543=CARTESIAN_POINT('Ctrl Pts',(-0.0028726803670096,-0.0231349809984428,
-0.0113108713225446));
#36544=CARTESIAN_POINT('Ctrl Pts',(-0.00287896103140741,-0.0231361432051581,
-0.01133201105998));
#36545=CARTESIAN_POINT('Ctrl Pts',(-0.00289250933946686,-0.0231387305260738,
-0.0113795254374897));
#36546=CARTESIAN_POINT('Ctrl Pts',(-0.00289965051084627,-0.0231401515288994,
-0.0114059342641506));
#36547=CARTESIAN_POINT('Ctrl Pts',(-0.00292016100649074,-0.0231444174218248,
-0.0114861213218808));
#36548=CARTESIAN_POINT('Ctrl Pts',(-0.00293240287541535,-0.0231472269774604,
-0.0115401769976581));
#36549=CARTESIAN_POINT('Ctrl Pts',(-0.00297207236807625,-0.0231574592920736,
-0.0117410213835194));
#36550=CARTESIAN_POINT('Ctrl Pts',(-0.00299002971515789,-0.0231646059010671,
-0.0118894622990809));
#36551=CARTESIAN_POINT('Ctrl Pts',(-0.00300559583878791,-0.0231807522976641,
-0.0122294141504176));
#36552=CARTESIAN_POINT('Ctrl Pts',(-0.0029960925765037,-0.0231896718262875,
-0.0124205786570992));
#36553=CARTESIAN_POINT('Ctrl Pts',(-0.00296381075814312,-0.0232009555258161,
-0.0126415501064568));
#36554=CARTESIAN_POINT('Ctrl Pts',(-0.00295861376559142,-0.0232026118335257,
-0.0126734999185925));
#36555=CARTESIAN_POINT('Ctrl Pts',(-0.00295010556193767,-0.0232051167442208,
-0.0127209477958998));
#36556=CARTESIAN_POINT('Ctrl Pts',(-0.00294718672836175,-0.0232059458503163,
-0.0127365146975156));
#36557=CARTESIAN_POINT('Ctrl Pts',(-0.00294170977354681,-0.0232074506346619,
-0.0127644994811818));
#36558=CARTESIAN_POINT('Ctrl Pts',(-0.00293919589356769,-0.0232081239226253,
-0.0127769258528152));
#36559=CARTESIAN_POINT('Ctrl Pts',(-0.00293380447619497,-0.0232095334851328,
-0.0128027333555016));
#36560=CARTESIAN_POINT('Ctrl Pts',(-0.00293091403207324,-0.0232102704110402,
-0.0128161112402563));
#36561=CARTESIAN_POINT('Ctrl Pts',(-0.00292290124489559,-0.0232122635857939,
-0.0128520052848254));
#36562=CARTESIAN_POINT('Ctrl Pts',(-0.00291761039856934,-0.0232135286362112,
-0.0128744824515229));
#36563=CARTESIAN_POINT('Ctrl Pts',(-0.00288665617718246,-0.0232206506095388,
-0.0129994967135615));
#36564=CARTESIAN_POINT('Ctrl Pts',(-0.002855848825205,-0.0232267363709775,
-0.0131006755329025));
#36565=CARTESIAN_POINT('Ctrl Pts',(-0.00274638886205968,-0.023245452260209,
-0.0134020477730704));
#36566=CARTESIAN_POINT('Ctrl Pts',(-0.00265149540460457,-0.0232582410588757,
-0.013595639514043));
#36567=CARTESIAN_POINT('Ctrl Pts',(-0.00249270407568463,-0.0232751102625787,
-0.0138471475353924));
#36568=CARTESIAN_POINT('Ctrl Pts',(-0.00244582931164683,-0.0232796997731493,
-0.0139150251589628));
#36569=CARTESIAN_POINT('Ctrl Pts',(-0.00237667169176011,-0.0232859552279127,
-0.0140068329757861));
#36570=CARTESIAN_POINT('Ctrl Pts',(-0.00235670862254464,-0.0232877068922193,
-0.0140324575884491));
#36571=CARTESIAN_POINT('Ctrl Pts',(-0.00232219008759264,-0.0232906470566577,
-0.014075311496423));
#36572=CARTESIAN_POINT('Ctrl Pts',(-0.0023078496472254,-0.0232918438269465,
-0.0140927096549726));
#36573=CARTESIAN_POINT('Ctrl Pts',(-0.0022783432070652,-0.0232942574521064,
-0.0141276963843144));
#36574=CARTESIAN_POINT('Ctrl Pts',(-0.0022631663700046,-0.0232954737501677,
-0.0141452738280123));
#36575=CARTESIAN_POINT('Ctrl Pts',(-0.00222473302081043,-0.0232984929567715,
-0.0141887553493092));
#36576=CARTESIAN_POINT('Ctrl Pts',(-0.00220122658527684,-0.0233002854819867,
-0.0142144345031235));
#36577=CARTESIAN_POINT('Ctrl Pts',(-0.002100671207382,-0.0233077392388126,
-0.014320516539461));
#36578=CARTESIAN_POINT('Ctrl Pts',(-0.00201962073313046,-0.0233132304196038,
-0.0143970095609957));
#36579=CARTESIAN_POINT('Ctrl Pts',(-0.00173040184436039,-0.023331515734298,
-0.0146410133396785));
#36580=CARTESIAN_POINT('Ctrl Pts',(-0.00150425926905786,-0.023343617765556,
-0.0147851588788914));
#36581=CARTESIAN_POINT('Ctrl Pts',(-0.00123021960874593,-0.0233588937189667,
-0.0149122362854303));
#36582=CARTESIAN_POINT('Ctrl Pts',(-0.00119811876274534,-0.0233606935068962,
-0.0149264429384479));
#36583=CARTESIAN_POINT('Ctrl Pts',(-0.0011509620525543,-0.0233633625733339,
-0.0149463306618513));
#36584=CARTESIAN_POINT('Ctrl Pts',(-0.00113609705993683,-0.0233642075243567,
-0.0149524594849928));
#36585=CARTESIAN_POINT('Ctrl Pts',(-0.00110965097839164,-0.023365718308758,
-0.0149631152596545));
#36586=CARTESIAN_POINT('Ctrl Pts',(-0.00109808995778753,-0.0233663813511167,
-0.0149676901436489));
#36587=CARTESIAN_POINT('Ctrl Pts',(-0.00107228129811609,-0.0233678674723673,
-0.0149777179384334));
#36588=CARTESIAN_POINT('Ctrl Pts',(-0.00105802044053036,-0.0233686925440834,
-0.014983134077151));
#36589=CARTESIAN_POINT('Ctrl Pts',(-0.00101495229980725,-0.0233711946348244,
-0.0149991161721482));
#36590=CARTESIAN_POINT('Ctrl Pts',(-0.000986024379158144,-0.0233728890964912,
-0.0150093488791007));
#36591=CARTESIAN_POINT('Ctrl Pts',(-0.000838439061164374,-0.0233815858327414,
-0.0150590207443831));
#36592=CARTESIAN_POINT('Ctrl Pts',(-0.000717562990775569,-0.0233888727326024,
-0.0150914550096578));
#36593=CARTESIAN_POINT('Ctrl Pts',(-0.000361166688076326,-0.023410222604845,
-0.0151635762786417));
#36594=CARTESIAN_POINT('Ctrl Pts',(-0.000122455609657768,-0.0234242767349491,
-0.0151828397785596));
#36595=CARTESIAN_POINT('Ctrl Pts',(0.000161450816837787,-0.0234399626810071,
-0.0151718504981361));
#36596=CARTESIAN_POINT('Ctrl Pts',(0.000206822055415894,-0.0234424416457245,
-0.0151690606969192));
#36597=CARTESIAN_POINT('Ctrl Pts',(0.000277703535384509,-0.0234462721034308,
-0.0151630828091748));
#36598=CARTESIAN_POINT('Ctrl Pts',(0.000303264674181463,-0.0234476448191112,
-0.0151605961678332));
#36599=CARTESIAN_POINT('Ctrl Pts',(0.000350697010799507,-0.0234501767699155,
-0.0151553662167663));
#36600=CARTESIAN_POINT('Ctrl Pts',(0.000372575828300688,-0.0234513385904576,
-0.0151527095110721));
#36601=CARTESIAN_POINT('Ctrl Pts',(0.000421308516417335,-0.0234539136103442,
-0.0151462462969905));
#36602=CARTESIAN_POINT('Ctrl Pts',(0.00044814420473259,-0.0234553228859412,
-0.0151423162201934));
#36603=CARTESIAN_POINT('Ctrl Pts',(0.000528386912996602,-0.02345951315051,
-0.0151294509372252));
#36604=CARTESIAN_POINT('Ctrl Pts',(0.000581610301473264,-0.0234622607023705,
-0.0151194330323656));
#36605=CARTESIAN_POINT('Ctrl Pts',(0.000837974738500974,-0.0234753842930941,
-0.0150639537211611));
#36606=CARTESIAN_POINT('Ctrl Pts',(0.00103627788179657,-0.0234851475601321,
-0.0149988763968803));
#36607=CARTESIAN_POINT('Ctrl Pts',(0.00135539564432791,-0.0235017481233994,
-0.0148559512421176));
#36608=CARTESIAN_POINT('Ctrl Pts',(0.00148027065097291,-0.0235085161118657,
-0.0147890532592776));
#36609=CARTESIAN_POINT('Ctrl Pts',(0.00162617433732151,-0.0235172830420758,
-0.0146970669449115));
#36610=CARTESIAN_POINT('Ctrl Pts',(0.0016521427825219,-0.02351887898852,
-0.0146801267083532));
#36611=CARTESIAN_POINT('Ctrl Pts',(0.0016905404944525,-0.0235212996522941,
-0.014654221186381));
#36612=CARTESIAN_POINT('Ctrl Pts',(0.00170317188596976,-0.023522106005,
-0.0146455577460638));
#36613=CARTESIAN_POINT('Ctrl Pts',(0.00172593326819518,-0.0235235783755579,
-0.0146296888307665));
#36614=CARTESIAN_POINT('Ctrl Pts',(0.00173608558528243,-0.0235242422487976,
-0.0146225165962814));
#36615=CARTESIAN_POINT('Ctrl Pts',(0.00175920839760339,-0.0235257706797939,
-0.0146059648086507));
#36616=CARTESIAN_POINT('Ctrl Pts',(0.00177214860401666,-0.0235266378718645,
-0.0145965444065685));
#36617=CARTESIAN_POINT('Ctrl Pts',(0.00181289915774787,-0.0235294048528137,
-0.01456637634965));
#36618=CARTESIAN_POINT('Ctrl Pts',(0.00184042440863483,-0.0235313276398202,
-0.0145452501858211));
#36619=CARTESIAN_POINT('Ctrl Pts',(0.00190603417494513,-0.0235360301696671,
-0.0144930603624058));
#36620=CARTESIAN_POINT('Ctrl Pts',(0.00194373338347046,-0.0235388326101583,
-0.0144615293403826));
#36621=CARTESIAN_POINT('Ctrl Pts',(0.00209984895726982,-0.0235508134268864,
-0.0143243005631146));
#36622=CARTESIAN_POINT('Ctrl Pts',(0.00221055291113015,-0.0235602403810694,
-0.0142102196791277));
#36623=CARTESIAN_POINT('Ctrl Pts',(0.00241586060585624,-0.0235790709217195,
-0.0139619999471457));
#36624=CARTESIAN_POINT('Ctrl Pts',(0.00250955849766848,-0.0235884306850111,
-0.0138277705668581));
#36625=CARTESIAN_POINT('Ctrl Pts',(0.0026112132874205,-0.0235994932828823,
-0.0136533652060758));
#36626=CARTESIAN_POINT('Ctrl Pts',(0.00262992283256313,-0.0236015768083667,
-0.0136198000949265));
#36627=CARTESIAN_POINT('Ctrl Pts',(0.00265924540100263,-0.0236049230840802,
-0.0135647334372807));
#36628=CARTESIAN_POINT('Ctrl Pts',(0.00267025417425417,-0.0236061994817181,
-0.0135434485723585));
#36629=CARTESIAN_POINT('Ctrl Pts',(0.00269105157791277,-0.0236086512154649,
-0.0135020291719188));
#36630=CARTESIAN_POINT('Ctrl Pts',(0.00270087214529936,-0.0236098275931987,
-0.0134819125366312));
#36631=CARTESIAN_POINT('Ctrl Pts',(0.00272341720491548,-0.0236125739626949,
-0.0134343888080795));
#36632=CARTESIAN_POINT('Ctrl Pts',(0.00273595472551468,-0.0236141375477828,
-0.0134068954288716));
#36633=CARTESIAN_POINT('Ctrl Pts',(0.00277716940817561,-0.0236194092136078,
-0.013312775030068));
#36634=CARTESIAN_POINT('Ctrl Pts',(0.00280384580791125,-0.0236230514275926,
-0.0132452973815259));
#36635=CARTESIAN_POINT('Ctrl Pts',(0.00286483208484318,-0.0236320718617216,
-0.0130730080707523));
#36636=CARTESIAN_POINT('Ctrl Pts',(0.00289585963240274,-0.0236373595709136,
-0.012967148739534));
#36637=CARTESIAN_POINT('Ctrl Pts',(0.00295904284199911,-0.0236505339000564,
-0.0126973137287968));
#36638=CARTESIAN_POINT('Ctrl Pts',(0.00298346455402076,-0.0236583283326594,
-0.0125319272272697));
#36639=CARTESIAN_POINT('Ctrl Pts',(0.00299802975031829,-0.0236696710627736,
-0.0123018357096217));
#36640=CARTESIAN_POINT('Ctrl Pts',(0.00300002797117741,-0.0236728630743604,
-0.0122381840786));
#36641=CARTESIAN_POINT('Ctrl Pts',(0.00299999054361381,-0.0236772161196921,
-0.012153889558734));
#36642=CARTESIAN_POINT('Ctrl Pts',(0.00299976854987172,-0.0236782914898092,
-0.0121332590510467));
#36643=CARTESIAN_POINT('Ctrl Pts',(0.0029990839987087,-0.0236800023245391,
-0.012100782158435));
#36644=CARTESIAN_POINT('Ctrl Pts',(0.00299876397406545,-0.0236806302852637,
-0.0120889330707929));
#36645=CARTESIAN_POINT('Ctrl Pts',(0.00299794811527417,-0.0236819513424072,
-0.0120641651603841));
#36646=CARTESIAN_POINT('Ctrl Pts',(0.00299743898140654,-0.0236826452036303,
-0.012051247216751));
#36647=CARTESIAN_POINT('Ctrl Pts',(0.00299595105809359,-0.0236843983686079,
-0.0120188222698312));
#36648=CARTESIAN_POINT('Ctrl Pts',(0.00299486523419974,-0.0236854632440509,
-0.0119993209334478));
#36649=CARTESIAN_POINT('Ctrl Pts',(0.00298971982698869,-0.0236897925541175,
-0.0119207414896186));
#36650=CARTESIAN_POINT('Ctrl Pts',(0.00298410203585482,-0.0236931284826456,
-0.0118617818810736));
#36651=CARTESIAN_POINT('Ctrl Pts',(0.00296319571437003,-0.0237027522423811,
-0.0116948584774248));
#36652=CARTESIAN_POINT('Ctrl Pts',(0.00294376189222309,-0.0237091533609841,
-0.0115875091274863));
#36653=CARTESIAN_POINT('Ctrl Pts',(0.00286824243901585,-0.0237283406928037,
-0.0112701011097754));
#36654=CARTESIAN_POINT('Ctrl Pts',(0.00279513604605515,-0.0237410462846934,
-0.0110647988626298));
#36655=CARTESIAN_POINT('Ctrl Pts',(0.00268114283103387,-0.0237554813356063,
-0.0108292114109037));
#36656=CARTESIAN_POINT('Ctrl Pts',(0.00266091923460957,-0.0237579011737365,
-0.0107896785738794));
#36657=CARTESIAN_POINT('Ctrl Pts',(0.00262773162207752,-0.0237616611612863,
-0.01072820882834));
#36658=CARTESIAN_POINT('Ctrl Pts',(0.00261535359962061,-0.0237630212882156,
-0.0107059643253993));
#36659=CARTESIAN_POINT('Ctrl Pts',(0.00259172483963726,-0.0237655413444303,
-0.0106647448157392));
#36660=CARTESIAN_POINT('Ctrl Pts',(0.00258054511684337,-0.023766703671097,
-0.010645731268688));
#36661=CARTESIAN_POINT('Ctrl Pts',(0.00255500200828728,-0.0237692940416021,
-0.0106033660120561));
#36662=CARTESIAN_POINT('Ctrl Pts',(0.00254052608598711,-0.0237707179279876,
-0.0105800842676697));
#36663=CARTESIAN_POINT('Ctrl Pts',(0.00249566212445967,-0.0237750025528376,
-0.0105100874142737));
#36664=CARTESIAN_POINT('Ctrl Pts',(0.00246428904959614,-0.0237778274786264,
-0.0104640164515927));
#36665=CARTESIAN_POINT('Ctrl Pts',(0.00234518414384714,-0.0237879892610772,
-0.0102991787212611));
#36666=CARTESIAN_POINT('Ctrl Pts',(0.00224999924323684,-0.0237950582837991,
-0.0101860533123454));
#36667=CARTESIAN_POINT('Ctrl Pts',(0.00201505041911801,-0.0238110198580356,
-0.00994534071763116));
#36668=CARTESIAN_POINT('Ctrl Pts',(0.0018707964137518,-0.0238198329906898,
-0.00982304171108499));
#36669=CARTESIAN_POINT('Ctrl Pts',(0.00168470088398697,-0.0238312657018724,
-0.00969326558468347));
#36670=CARTESIAN_POINT('Ctrl Pts',(0.0016529595227852,-0.0238332185855835,
-0.00967201956001385));
#36671=CARTESIAN_POINT('Ctrl Pts',(0.00160698944913888,-0.0238360637387799,
-0.00964250468260526));
#36672=CARTESIAN_POINT('Ctrl Pts',(0.00159308379939658,-0.0238369265367141,
-0.0096337371950161));
#36673=CARTESIAN_POINT('Ctrl Pts',(0.00156849450791277,-0.0238384572597799,
-0.00961851467576912));
#36674=CARTESIAN_POINT('Ctrl Pts',(0.00155784156184011,-0.0238391221125371,
-0.00961201135410414));
#36675=CARTESIAN_POINT('Ctrl Pts',(0.00153449332920944,-0.0238405832890102,
-0.00959795717038656));
#36676=CARTESIAN_POINT('Ctrl Pts',(0.00152178287125252,-0.0238413811774976,
-0.00959043358412277));
#36677=CARTESIAN_POINT('Ctrl Pts',(0.00148460701276105,-0.0238437207580452,
-0.00956879752774689));
#36678=CARTESIAN_POINT('Ctrl Pts',(0.00145999782236882,-0.0238452768492956,
-0.0095549366611428));
#36679=CARTESIAN_POINT('Ctrl Pts',(0.00140246836106279,-0.0238489250415796,
-0.00952359545314692));
#36680=CARTESIAN_POINT('Ctrl Pts',(0.00136941097650588,-0.0238510291458285,
-0.00950637721680226));
#36681=CARTESIAN_POINT('Ctrl Pts',(0.00125063463585268,-0.0238585950199303,
-0.00944729831396889));
#36682=CARTESIAN_POINT('Ctrl Pts',(0.00116325269860505,-0.0238641699584645,
-0.00940891621795724));
#36683=CARTESIAN_POINT('Ctrl Pts',(0.00084795183712398,-0.02388400525069,
-0.00928800085618762));
#36684=CARTESIAN_POINT('Ctrl Pts',(0.00061198901376958,-0.0238982542268815,
-0.00922895333819541));
#36685=CARTESIAN_POINT('Ctrl Pts',(0.000329943583971665,-0.0239138851627141,
-0.00919375862347097));
#36686=CARTESIAN_POINT('Ctrl Pts',(0.000288311332469997,-0.023916160630979,
-0.00918944605319591));
#36687=CARTESIAN_POINT('Ctrl Pts',(0.000222008612282317,-0.0239197353439104,
-0.00918397744096975));
#36688=CARTESIAN_POINT('Ctrl Pts',(0.000197391669231275,-0.0239210518606808,
-0.00918225253203083));
#36689=CARTESIAN_POINT('Ctrl Pts',(0.000150622249964357,-0.0239235334687419,
-0.0091795548269802));
#36690=CARTESIAN_POINT('Ctrl Pts',(0.000128474914068545,-0.0239247002811825,
-0.00917852351614038));
#36691=CARTESIAN_POINT('Ctrl Pts',(7.76905004197529E-5,-0.0239273575422776,
-0.00917672262292262));
#36692=CARTESIAN_POINT('Ctrl Pts',(4.90495511143069E-5,-0.023928842852224,
-0.00917611750385087));
#36693=CARTESIAN_POINT('Ctrl Pts',(-4.22941296485705E-5,-0.0239335406998544,
-0.00917549624073787));
#36694=CARTESIAN_POINT('Ctrl Pts',(-0.000104992255973168,-0.0239367060219711,
-0.00917703543593957));
#36695=CARTESIAN_POINT('Ctrl Pts',(-0.000256299349197304,-0.0239442374556768,
-0.00918550163007713));
#36696=CARTESIAN_POINT('Ctrl Pts',(-0.000344738729613,-0.0239485494600936,
-0.00919440248335395));
#36697=CARTESIAN_POINT('Ctrl Pts',(-0.000545584499344328,-0.0239582763654799,
-0.00922367422563607));
#36698=CARTESIAN_POINT('Ctrl Pts',(-0.000657482488847247,-0.0239636465910073,
-0.00924656316237376));
#36699=CARTESIAN_POINT('Ctrl Pts',(-0.000907689727629172,-0.0239759500161392,
-0.00931280612047121));
#36700=CARTESIAN_POINT('Ctrl Pts',(-0.00104469968193725,-0.023982899584126,
-0.00935991046741799));
#36701=CARTESIAN_POINT('Ctrl Pts',(-0.00120015539018096,-0.0239915729879346,
-0.00942626787771243));
#36702=CARTESIAN_POINT('Ctrl Pts',(-0.00122243177870939,-0.0239928356952982,
-0.00943609903565198));
#36703=CARTESIAN_POINT('Ctrl Pts',(-0.00125728484333931,-0.0239948463244324,
-0.00945199028926844));
#36704=CARTESIAN_POINT('Ctrl Pts',(-0.00126994353020839,-0.0239955839457915,
-0.00945786906658127));
#36705=CARTESIAN_POINT('Ctrl Pts',(-0.0012940387654259,-0.0239970029115556,
-0.00946926412476303));
#36706=CARTESIAN_POINT('Ctrl Pts',(-0.00130548199015796,-0.023997683370686,
-0.00947476499309754));
#36707=CARTESIAN_POINT('Ctrl Pts',(-0.00133331782298868,-0.0239993541750954,
-0.00948836414554664));
#36708=CARTESIAN_POINT('Ctrl Pts',(-0.00134967185901501,-0.0240003490445426,
-0.00949653991557034));
#36709=CARTESIAN_POINT('Ctrl Pts',(-0.00140974375741294,-0.0240040496642591,
-0.00952726082024025));
#36710=CARTESIAN_POINT('Ctrl Pts',(-0.00145297804211985,-0.0240068040930066,
-0.00955072970891422));
#36711=CARTESIAN_POINT('Ctrl Pts',(-0.00156589836989284,-0.0240142045036448,
-0.00961567045438753));
#36712=CARTESIAN_POINT('Ctrl Pts',(-0.00163451259410128,-0.0240189152547235,
-0.00965892238592604));
#36713=CARTESIAN_POINT('Ctrl Pts',(-0.00191431720798182,-0.024038808655251,
-0.00985157174534062));
#36714=CARTESIAN_POINT('Ctrl Pts',(-0.00210752725721548,-0.0240541257260356,
-0.0100252101521695));
#36715=CARTESIAN_POINT('Ctrl Pts',(-0.00230480160209691,-0.0240708232947452,
-0.0102549590997473));
#36716=CARTESIAN_POINT('Ctrl Pts',(-0.00233279094855534,-0.0240732264113264,
-0.0102890486935559));
#36717=CARTESIAN_POINT('Ctrl Pts',(-0.00237569514221927,-0.0240769664440387,
-0.010343718659823));
#36718=CARTESIAN_POINT('Ctrl Pts',(-0.00239111682728279,-0.0240783229911736,
-0.0103638916227171));
#36719=CARTESIAN_POINT('Ctrl Pts',(-0.00241945611621449,-0.0240808397212438,
-0.0104019539595377));
#36720=CARTESIAN_POINT('Ctrl Pts',(-0.00243243598096626,-0.0240820022476223,
-0.0104197946446341));
#36721=CARTESIAN_POINT('Ctrl Pts',(-0.00246115110699001,-0.0240845972626595,
-0.0104601926151336));
#36722=CARTESIAN_POINT('Ctrl Pts',(-0.00247677546026185,-0.0240860255239846,
-0.0104828265013731));
#36723=CARTESIAN_POINT('Ctrl Pts',(-0.00252337724409488,-0.0240903386750709,
-0.0105523613026109));
#36724=CARTESIAN_POINT('Ctrl Pts',(-0.00255335063593726,-0.024093187017553,
-0.0105999218259456));
#36725=CARTESIAN_POINT('Ctrl Pts',(-0.00265436373082325,-0.0241030959488388,
-0.0107706606451979));
#36726=CARTESIAN_POINT('Ctrl Pts',(-0.00271796971260307,-0.0241099135746922,
-0.0108980199902509));
#36727=CARTESIAN_POINT('Ctrl Pts',(-0.00284122365024305,-0.024125227474835,
-0.0111960716815049));
#36728=CARTESIAN_POINT('Ctrl Pts',(-0.00289496780241338,-0.0241336481743369,
-0.0113685892165997));
#36729=CARTESIAN_POINT('Ctrl Pts',(-0.00294274324812855,-0.0241449837054204,
-0.0115906563681281));
#36730=CARTESIAN_POINT('Ctrl Pts',(-0.00295151940713886,-0.0241473593751018,
-0.0116366631436839));
#36731=CARTESIAN_POINT('Ctrl Pts',(-0.00296224567888654,-0.024150744668708,
-0.0117010473072671));
#36732=CARTESIAN_POINT('Ctrl Pts',(-0.00296510871728592,-0.0241517094162642,
-0.0117192676521714));
#36733=CARTESIAN_POINT('Ctrl Pts',(-0.00296964436012739,-0.0241533484297562,
-0.0117499764202617));
#36734=CARTESIAN_POINT('Ctrl Pts',(-0.00297140666992105,-0.024154017871949,
-0.0117624513874241));
#36735=CARTESIAN_POINT('Ctrl Pts',(-0.00297494112352456,-0.0241554325833925,
-0.0117886619789096));
#36736=CARTESIAN_POINT('Ctrl Pts',(-0.00297669680059275,-0.0241561786686898,
-0.0118023992207003));
#36737=CARTESIAN_POINT('Ctrl Pts',(-0.00298121629841019,-0.0241582227123249,
-0.0118398206155733));
#36738=CARTESIAN_POINT('Ctrl Pts',(-0.00298379290677064,-0.0241595302210376,
-0.0118635259052746));
#36739=CARTESIAN_POINT('Ctrl Pts',(-0.00299808405839939,-0.0241677545923681,
-0.0120113963404177));
#36740=CARTESIAN_POINT('Ctrl Pts',(-0.00300232786590801,-0.0241749883084336,
-0.0121361514787953));
#36741=CARTESIAN_POINT('Ctrl Pts',(-0.00299292543339883,-0.0241944537032271,
-0.0124680907328181));
#36742=CARTESIAN_POINT('Ctrl Pts',(-0.0029655741872156,-0.0242067291955422,
-0.0126742426040832));
#36743=CARTESIAN_POINT('Ctrl Pts',(-0.00290013222451379,-0.0242225432378703,
-0.0129469332675166));
#36744=CARTESIAN_POINT('Ctrl Pts',(-0.00288050612876583,-0.0242265899030205,
-0.0130172907045883));
#36745=CARTESIAN_POINT('Ctrl Pts',(-0.00284890094943722,-0.0242322433996795,
-0.0131164529252348));
#36746=CARTESIAN_POINT('Ctrl Pts',(-0.00283901196112395,-0.0242339155452147,
-0.013145892194538));
#36747=CARTESIAN_POINT('Ctrl Pts',(-0.00282116586804867,-0.0242367748349669,
-0.0131964072011758));
#36748=CARTESIAN_POINT('Ctrl Pts',(-0.0028134253392826,-0.0242379688864223,
-0.0132175562409481));
#36749=CARTESIAN_POINT('Ctrl Pts',(-0.00279706253746286,-0.0242404019626443,
-0.0132607502246054));
#36750=CARTESIAN_POINT('Ctrl Pts',(-0.00278841602177665,-0.0242416400889513,
-0.0132827843306514));
#36751=CARTESIAN_POINT('Ctrl Pts',(-0.00276558407820692,-0.0242447924676459,
-0.0133390017098491));
#36752=CARTESIAN_POINT('Ctrl Pts',(-0.00275102505997585,-0.0242466942548846,
-0.0133730294725887));
#36753=CARTESIAN_POINT('Ctrl Pts',(-0.00267794369588618,-0.0242557536201294,
-0.0135354590277854));
#36754=CARTESIAN_POINT('Ctrl Pts',(-0.0026110379929825,-0.0242626261821099,
-0.0136599005178529));
#36755=CARTESIAN_POINT('Ctrl Pts',(-0.00250833261636015,-0.0242718130524532,
-0.0138223263822906));
#36756=CARTESIAN_POINT('Ctrl Pts',(-0.00247995185372159,-0.0242742368375516,
-0.0138647715993533));
#36757=CARTESIAN_POINT('Ctrl Pts',(-0.00234010402643788,-0.0242857281933064,
-0.0140627916870461));
#36758=CARTESIAN_POINT('Ctrl Pts',(-0.0022150138999388,-0.0242946959407717,
-0.0142081724513265));
#36759=CARTESIAN_POINT('Ctrl Pts',(-0.00205648872608341,-0.0243058969783698,
-0.0143602658352723));
#36760=CARTESIAN_POINT('Ctrl Pts',(-0.00203575059417655,-0.0243073599010185,
-0.014379605421406));
#36761=CARTESIAN_POINT('Ctrl Pts',(-0.00200365119226635,-0.0243096262983495,
-0.0144087003412662));
#36762=CARTESIAN_POINT('Ctrl Pts',(-0.00199248535873276,-0.0243104150331364,
-0.0144186698520948));
#36763=CARTESIAN_POINT('Ctrl Pts',(-0.00197189184760518,-0.0243118713818575,
-0.0144367817930769));
#36764=CARTESIAN_POINT('Ctrl Pts',(-0.0019624874281233,-0.0243125371556687,
-0.0144449496371799));
#36765=CARTESIAN_POINT('Ctrl Pts',(-0.00194055137058768,-0.0243140915830116,
-0.014463762973664));
#36766=CARTESIAN_POINT('Ctrl Pts',(-0.00192798282004478,-0.0243149832360436,
-0.0144743642348176));
#36767=CARTESIAN_POINT('Ctrl Pts',(-0.00188671358988223,-0.0243179124919269,
-0.0145085971652751));
#36768=CARTESIAN_POINT('Ctrl Pts',(-0.00185766161182833,-0.0243199768675801,
-0.0145317979518989));
#36769=CARTESIAN_POINT('Ctrl Pts',(-0.00178533152702683,-0.024325106633711,
-0.0145873907489847));
#36770=CARTESIAN_POINT('Ctrl Pts',(-0.00174159517949529,-0.0243282000066036,
-0.0146191640112853));
#36771=CARTESIAN_POINT('Ctrl Pts',(-0.00153457327967907,-0.0243427208204296,
-0.0147611762112899));
#36772=CARTESIAN_POINT('Ctrl Pts',(-0.00136153691141119,-0.0243544782662629,
-0.0148563444089712));
#36773=CARTESIAN_POINT('Ctrl Pts',(-0.00106941452980384,-0.0243728244026265,
-0.0149813710614554));
#36774=CARTESIAN_POINT('Ctrl Pts',(-0.000955641409285482,-0.0243796447733796,
-0.0150221372015616));
#36775=CARTESIAN_POINT('Ctrl Pts',(-0.000804799545090952,-0.0243882358332565,
-0.0150661162531718));
#36776=CARTESIAN_POINT('Ctrl Pts',(-0.000769706148129626,-0.0243902042388357,
-0.0150756593020119));
#36777=CARTESIAN_POINT('Ctrl Pts',(-0.000711626713634182,-0.0243934133764966,
-0.0150903243157034));
#36778=CARTESIAN_POINT('Ctrl Pts',(-0.000688739153962839,-0.0243946657342736,
-0.0150958177349251));
#36779=CARTESIAN_POINT('Ctrl Pts',(-0.000643758820624876,-0.0243971036226168,
-0.0151060555057694));
#36780=CARTESIAN_POINT('Ctrl Pts',(-0.00062167245411589,-0.0243982897399379,
-0.0151108207244348));
#36781=CARTESIAN_POINT('Ctrl Pts',(-0.000568685450939444,-0.0244011101683298,
-0.0151216279003162));
#36782=CARTESIAN_POINT('Ctrl Pts',(-0.0005377391137935,-0.0244027370196843,
-0.0151274338730667));
#36783=CARTESIAN_POINT('Ctrl Pts',(-0.000426406157636438,-0.0244085219655865,
-0.0151465123483362));
#36784=CARTESIAN_POINT('Ctrl Pts',(-0.000345575280657453,-0.024412594585354,
-0.0151569967897483));
#36785=CARTESIAN_POINT('Ctrl Pts',(-0.000132199737694094,-0.0244231071782559,
-0.0151758766990228));
#36786=CARTESIAN_POINT('Ctrl Pts',(6.48715944714436E-7,-0.0244294078662443,
-0.0151787883733568));
#36787=CARTESIAN_POINT('Ctrl Pts',(0.000313364980468944,-0.0244442392018449,
-0.0151648841708013));
#36788=CARTESIAN_POINT('Ctrl Pts',(0.000492366994113262,-0.0244527253854847,
-0.0151406576085166));
#36789=CARTESIAN_POINT('Ctrl Pts',(0.000696430413059063,-0.0244633872474118,
-0.0150940427529168));
#36790=CARTESIAN_POINT('Ctrl Pts',(0.000724674107923275,-0.0244648858597611,
-0.0150871575305837));
#36791=CARTESIAN_POINT('Ctrl Pts',(0.000767447975458425,-0.0244671964531476,
-0.015076069175621));
#36792=CARTESIAN_POINT('Ctrl Pts',(0.000782054470761734,-0.0244679928051731,
-0.0150721646275349));
#36793=CARTESIAN_POINT('Ctrl Pts',(0.000808512061225958,-0.0244694496242428,
-0.0150648773652863));
#36794=CARTESIAN_POINT('Ctrl Pts',(0.000820372690964561,-0.0244701080362392,
-0.0150615318053742));
#36795=CARTESIAN_POINT('Ctrl Pts',(0.000847752412282308,-0.0244716402376234,
-0.0150536262920582));
#36796=CARTESIAN_POINT('Ctrl Pts',(0.000863255504750196,-0.0244725168827634,
-0.0150490138344148));
#36797=CARTESIAN_POINT('Ctrl Pts',(0.000912798500201012,-0.0244753457871115,
-0.0150338367041929));
#36798=CARTESIAN_POINT('Ctrl Pts',(0.000946686645037905,-0.024477322451287,
-0.0150227910267888));
#36799=CARTESIAN_POINT('Ctrl Pts',(0.00102855657802995,-0.0244821861649201,
-0.0149944825789868));
#36800=CARTESIAN_POINT('Ctrl Pts',(0.00107631003869392,-0.0244850978421941,
-0.0149765953247235));
#36801=CARTESIAN_POINT('Ctrl Pts',(0.0012829169667477,-0.0244979589918213,
-0.0148931412285657));
#36802=CARTESIAN_POINT('Ctrl Pts',(0.00143642617006764,-0.0245081856067871,
-0.0148152112498838));
#36803=CARTESIAN_POINT('Ctrl Pts',(0.0017083842645252,-0.0245268305120799,
-0.0146463606072049));
#36804=CARTESIAN_POINT('Ctrl Pts',(0.00182838862450916,-0.0245352819933739,
-0.0145589159267533));
#36805=CARTESIAN_POINT('Ctrl Pts',(0.00197026495764921,-0.0245454736888598,
-0.0144384811783818));
#36806=CARTESIAN_POINT('Ctrl Pts',(0.00199861960093413,-0.0245475224839742,
-0.0144134745342386));
#36807=CARTESIAN_POINT('Ctrl Pts',(0.00204406848245994,-0.0245508273779867,
-0.0143718387259144));
#36808=CARTESIAN_POINT('Ctrl Pts',(0.00206144986247046,-0.0245520965025603,
-0.0143555304460652));
#36809=CARTESIAN_POINT('Ctrl Pts',(0.00209481577950532,-0.0245545436449413,
-0.0143234683354241));
#36810=CARTESIAN_POINT('Ctrl Pts',(0.002110821474379,-0.024555722571682,
-0.0143077389044522));
#36811=CARTESIAN_POINT('Ctrl Pts',(0.00214820825818189,-0.0245584892800598,
-0.0142701635648651));
#36812=CARTESIAN_POINT('Ctrl Pts',(0.00216943512202904,-0.0245600703666536,
-0.0142481673558518));
#36813=CARTESIAN_POINT('Ctrl Pts',(0.00224150834893708,-0.0245654790661008,
-0.014171160590113));
#36814=CARTESIAN_POINT('Ctrl Pts',(0.00229062997381936,-0.0245692358539022,
-0.014114570992703));
#36815=CARTESIAN_POINT('Ctrl Pts',(0.00241021144939596,-0.0245786375309269,
-0.0139659111973718));
#36816=CARTESIAN_POINT('Ctrl Pts',(0.0024775492219414,-0.0245841806875644,
-0.0138714884090777));
#36817=CARTESIAN_POINT('Ctrl Pts',(0.00263600350410661,-0.0245983073758991,
-0.0136196301003421));
#36818=CARTESIAN_POINT('Ctrl Pts',(0.00271857249125541,-0.0246067903875411,
-0.0134573988988336));
#36819=CARTESIAN_POINT('Ctrl Pts',(0.00280275794494099,-0.0246181328691637,
-0.0132466472515459));
#36820=CARTESIAN_POINT('Ctrl Pts',(0.00281860531429751,-0.0246204334452691,
-0.013204209011279));
#36821=CARTESIAN_POINT('Ctrl Pts',(0.00283946248174454,-0.0246237279465049,
-0.0131442456962797));
#36822=CARTESIAN_POINT('Ctrl Pts',(0.0028452832819412,-0.0246246800712975,
-0.0131270073529358));
#36823=CARTESIAN_POINT('Ctrl Pts',(0.00285489446407619,-0.0246263108298569,
-0.01309766586315));
#36824=CARTESIAN_POINT('Ctrl Pts',(0.00285876564042425,-0.0246269849350396,
-0.0130855894230883));
#36825=CARTESIAN_POINT('Ctrl Pts',(0.00286674740120017,-0.0246284124479961,
-0.0130601355816776));
#36826=CARTESIAN_POINT('Ctrl Pts',(0.00287084108572552,-0.0246291667128416,
-0.0130467535590475));
#36827=CARTESIAN_POINT('Ctrl Pts',(0.00288185008939962,-0.024631256446154,
-0.0130098445332519));
#36828=CARTESIAN_POINT('Ctrl Pts',(0.0028885706605584,-0.0246326021584463,
-0.0129862610852846));
#36829=CARTESIAN_POINT('Ctrl Pts',(0.00293680454295546,-0.0246427942332822,
-0.0128087739990707));
#36830=CARTESIAN_POINT('Ctrl Pts',(0.00296627808353792,-0.0246521521782912,
-0.0126518741132068));
#36831=CARTESIAN_POINT('Ctrl Pts',(0.00299434044326856,-0.0246677440425888,
-0.0123882387308766));
#36832=CARTESIAN_POINT('Ctrl Pts',(0.00299996571188081,-0.0246739614871394,
-0.0122825746941183));
#36833=CARTESIAN_POINT('Ctrl Pts',(0.00299999984374834,-0.0246800791551026,
-0.0121768215375357));
#36834=CARTESIAN_POINT('',(0.00299999999556417,-0.0266759885990988,-0.0121756901455692));
#36835=CARTESIAN_POINT('Ctrl Pts',(0.00299999984374834,-0.0246800791551026,
-0.0121768215375361));
#36836=CARTESIAN_POINT('Ctrl Pts',(0.0030000271394786,-0.0246849715394514,
-0.0120922492640467));
#36837=CARTESIAN_POINT('Ctrl Pts',(0.00299647877875121,-0.0246897951466881,
-0.012007719316541));
#36838=CARTESIAN_POINT('Ctrl Pts',(0.0029851797271477,-0.0246973003957579,
-0.0118739046611527));
#36839=CARTESIAN_POINT('Ctrl Pts',(0.00297976667861642,-0.0247000442136567,
-0.011824481818541));
#36840=CARTESIAN_POINT('Ctrl Pts',(0.00296977267758926,-0.0247041191505159,
-0.0117503166974606));
#36841=CARTESIAN_POINT('Ctrl Pts',(0.00296610496658861,-0.0247054775876757,
-0.0117254617630247));
#36842=CARTESIAN_POINT('Ctrl Pts',(0.00295883097818313,-0.0247079429921856,
-0.0116801196810558));
#36843=CARTESIAN_POINT('Ctrl Pts',(0.00295532304068977,-0.024709052922994,
-0.0116596185340017));
#36844=CARTESIAN_POINT('Ctrl Pts',(0.00294765741526115,-0.024711325890459,
-0.0116174609867613));
#36845=CARTESIAN_POINT('Ctrl Pts',(0.00294347357689748,-0.0247124880340499,
-0.0115958105855758));
#36846=CARTESIAN_POINT('Ctrl Pts',(0.00293357193311885,-0.0247150736036087,
-0.0115474408326705));
#36847=CARTESIAN_POINT('Ctrl Pts',(0.00292772699980406,-0.024716492944789,
-0.0115207493426016));
#36848=CARTESIAN_POINT('Ctrl Pts',(0.00290938173190182,-0.0247206540978431,
-0.0114421296362844));
#36849=CARTESIAN_POINT('Ctrl Pts',(0.0028958581845863,-0.0247233638757336,
-0.0113904500371739));
#36850=CARTESIAN_POINT('Ctrl Pts',(0.00282939955094125,-0.0247352869549178,
-0.0111616157966445));
#36851=CARTESIAN_POINT('Ctrl Pts',(0.00276153367853952,-0.0247440349531215,
-0.010989212134275));
#36852=CARTESIAN_POINT('Ctrl Pts',(0.0026286760278695,-0.0247580065665102,
-0.0107259716925797));
#36853=CARTESIAN_POINT('Ctrl Pts',(0.00257376619301133,-0.0247632194913892,
-0.010630596062701));
#36854=CARTESIAN_POINT('Ctrl Pts',(0.00248691976406342,-0.0247710047313163,
-0.0104972687386255));
#36855=CARTESIAN_POINT('Ctrl Pts',(0.0024590851232924,-0.0247734423320927,
-0.0104567500457898));
#36856=CARTESIAN_POINT('Ctrl Pts',(0.0024099226142933,-0.0247776847851966,
-0.0103888229955561));
#36857=CARTESIAN_POINT('Ctrl Pts',(0.00238909084963975,-0.0247794647123323,
-0.0103610670769178));
#36858=CARTESIAN_POINT('Ctrl Pts',(0.00235795385591366,-0.0247821096638489,
-0.0103210460613349));
#36859=CARTESIAN_POINT('Ctrl Pts',(0.00234802378661415,-0.0247829509765828,
-0.010308491376139));
#36860=CARTESIAN_POINT('Ctrl Pts',(0.00233020467891303,-0.0247844579850185,
-0.0102863293576096));
#36861=CARTESIAN_POINT('Ctrl Pts',(0.00232235570566486,-0.0247851209498248,
-0.0102766907102858));
#36862=CARTESIAN_POINT('Ctrl Pts',(0.0023047019852878,-0.0247866103758972,
-0.0102552847922193));
#36863=CARTESIAN_POINT('Ctrl Pts',(0.00229486697647337,-0.0247874388831487,
-0.010243543755816));
#36864=CARTESIAN_POINT('Ctrl Pts',(0.00226485497803572,-0.0247899619563692,
-0.0102082677285596));
#36865=CARTESIAN_POINT('Ctrl Pts',(0.00224440323299895,-0.0247916743780112,
-0.010184970321547));
#36866=CARTESIAN_POINT('Ctrl Pts',(0.00212660959357736,-0.0248014779133856,
-0.010054908868805));
#36867=CARTESIAN_POINT('Ctrl Pts',(0.00202202184638895,-0.0248099496334261,
-0.00995497613217003));
#36868=CARTESIAN_POINT('Ctrl Pts',(0.00179053011871227,-0.0248276059760619,
-0.00976374259653401));
#36869=CARTESIAN_POINT('Ctrl Pts',(0.0016628516632203,-0.0248367629338216,
-0.00967401252558521));
#36870=CARTESIAN_POINT('Ctrl Pts',(0.00147681606898583,-0.0248490611889767,
-0.0095638309311238));
#36871=CARTESIAN_POINT('Ctrl Pts',(0.00142393942697235,-0.0248524514176395,
-0.00953463317930624));
#36872=CARTESIAN_POINT('Ctrl Pts',(0.00132809846362635,-0.0248584065537394,
-0.00948542658340009));
#36873=CARTESIAN_POINT('Ctrl Pts',(0.00128547449483161,-0.0248609907740733,
-0.0094648023754128));
#36874=CARTESIAN_POINT('Ctrl Pts',(0.00121889485155252,-0.0248649306120928,
-0.00943451037098353));
#36875=CARTESIAN_POINT('Ctrl Pts',(0.00119527386442428,-0.0248663100176773,
-0.00942412908429987));
#36876=CARTESIAN_POINT('Ctrl Pts',(0.0011512390915213,-0.024868848404098,
-0.0094054500766122));
#36877=CARTESIAN_POINT('Ctrl Pts',(0.00113086229457634,-0.0248700100693831,
-0.00939707011818949));
#36878=CARTESIAN_POINT('Ctrl Pts',(0.00108533696072991,-0.0248725775034092,
-0.00937893154217753));
#36879=CARTESIAN_POINT('Ctrl Pts',(0.00106014525041828,-0.024873979465628,
-0.00936928604667271));
#36880=CARTESIAN_POINT('Ctrl Pts',(0.000995629909773804,-0.0248775244149862,
-0.00934557680984292));
#36881=CARTESIAN_POINT('Ctrl Pts',(0.000956135904486478,-0.0248796519266907,
-0.00933199179282939));
#36882=CARTESIAN_POINT('Ctrl Pts',(0.000737537006826487,-0.0248912171752032,
-0.00926186780337004));
#36883=CARTESIAN_POINT('Ctrl Pts',(0.000553702147464557,-0.0249001400695489,
-0.00922141704469027));
#36884=CARTESIAN_POINT('Ctrl Pts',(0.00023952789727079,-0.0249151378517388,
-0.00918266150627814));
#36885=CARTESIAN_POINT('Ctrl Pts',(0.000110893656095513,-0.0249212202540674,
-0.00917514171568758));
#36886=CARTESIAN_POINT('Ctrl Pts',(-8.29382840763949E-5,-0.0249307537628703,
-0.00917629298347272));
#36887=CARTESIAN_POINT('Ctrl Pts',(-0.000148024479865065,-0.0249340186355012,
-0.00917879999159463));
#36888=CARTESIAN_POINT('Ctrl Pts',(-0.000233088028873369,-0.0249384263639998,
-0.00918485401746374));
#36889=CARTESIAN_POINT('Ctrl Pts',(-0.000253187415226254,-0.0249394781938473,
-0.0091864883461244));
#36890=CARTESIAN_POINT('Ctrl Pts',(-0.000286270943035285,-0.0249412287383808,
-0.00918951448605934));
#36891=CARTESIAN_POINT('Ctrl Pts',(-0.000299265543948449,-0.0249419212212067,
-0.00919078869602892));
#36892=CARTESIAN_POINT('Ctrl Pts',(-0.000323916940709067,-0.024943244883031,
-0.00919336851806675));
#36893=CARTESIAN_POINT('Ctrl Pts',(-0.000335575173114158,-0.0249438751025326,
-0.00919465774238381));
#36894=CARTESIAN_POINT('Ctrl Pts',(-0.000367067573682288,-0.0249455883960714,
-0.00919832739141528));
#36895=CARTESIAN_POINT('Ctrl Pts',(-0.000386885689650826,-0.0249466782517823,
-0.00920083757560438));
#36896=CARTESIAN_POINT('Ctrl Pts',(-0.000464085223446902,-0.0249509654014279,
-0.00921140016014898));
#36897=CARTESIAN_POINT('Ctrl Pts',(-0.000521250793847492,-0.0249542299593569,
-0.00922091602249985));
#36898=CARTESIAN_POINT('Ctrl Pts',(-0.000746175468686555,-0.0249673407682444,
-0.00926508697398773));
#36899=CARTESIAN_POINT('Ctrl Pts',(-0.000911109901030542,-0.0249775256807038,
-0.00931242607945585));
#36900=CARTESIAN_POINT('Ctrl Pts',(-0.00120113197068892,-0.0249956896467627,
-0.00942327987439296));
#36901=CARTESIAN_POINT('Ctrl Pts',(-0.00132755693874223,-0.0250037066676969,
-0.00948197542543346));
#36902=CARTESIAN_POINT('Ctrl Pts',(-0.00149728314555392,-0.0250144876078641,
-0.00957563659779584));
#36903=CARTESIAN_POINT('Ctrl Pts',(-0.0015443795621772,-0.0250174827904314,
-0.00960333002301077));
#36904=CARTESIAN_POINT('Ctrl Pts',(-0.00161376505350052,-0.0250219021941725,
-0.00964672246954577));
#36905=CARTESIAN_POINT('Ctrl Pts',(-0.00163663754514,-0.025023360206945,
-0.00966146311208925));
#36906=CARTESIAN_POINT('Ctrl Pts',(-0.00167767133834964,-0.0250259788418739,
-0.00968870536516019));
#36907=CARTESIAN_POINT('Ctrl Pts',(-0.0016959011985513,-0.0250271432827949,
-0.00970109975096745));
#36908=CARTESIAN_POINT('Ctrl Pts',(-0.00173501163478727,-0.025029644528405,
-0.00972832586253106));
#36909=CARTESIAN_POINT('Ctrl Pts',(-0.00175584232463214,-0.0250309786359784,
-0.00974322638376825));
#36910=CARTESIAN_POINT('Ctrl Pts',(-0.00181283907661768,-0.0250346361936943,
-0.00978511065343833));
#36911=CARTESIAN_POINT('Ctrl Pts',(-0.0018485917528818,-0.0250369385512274,
-0.00981264685138758));
#36912=CARTESIAN_POINT('Ctrl Pts',(-0.00204550391388021,-0.0250496925744515,
-0.00997151011495595));
#36913=CARTESIAN_POINT('Ctrl Pts',(-0.00219329210781418,-0.025059497600809,
-0.0101185024539239));
#36914=CARTESIAN_POINT('Ctrl Pts',(-0.00239729318432934,-0.0250747972721603,
-0.0103685972404435));
#36915=CARTESIAN_POINT('Ctrl Pts',(-0.00246471021951447,-0.0250802559978145,
-0.0104616800527805));
#36916=CARTESIAN_POINT('Ctrl Pts',(-0.0025595396148326,-0.025088933298469,
-0.0106098122484654));
#36917=CARTESIAN_POINT('Ctrl Pts',(-0.00259087771523434,-0.0250920023462928,
-0.0106622221109417));
#36918=CARTESIAN_POINT('Ctrl Pts',(-0.00263020017016898,-0.0250961811488614,
-0.0107327882904812));
#36919=CARTESIAN_POINT('Ctrl Pts',(-0.0026396365257818,-0.0250972112688108,
-0.0107501224249636));
#36920=CARTESIAN_POINT('Ctrl Pts',(-0.00265498900491641,-0.0250989353644997,
-0.0107789991146032));
#36921=CARTESIAN_POINT('Ctrl Pts',(-0.00266100270413413,-0.025099623489405,
-0.0107904895090416));
#36922=CARTESIAN_POINT('Ctrl Pts',(-0.00267235047423996,-0.0251009473524312,
-0.010812518241925));
#36923=CARTESIAN_POINT('Ctrl Pts',(-0.00267769714287106,-0.0251015822329976,
-0.0108230497152173));
#36924=CARTESIAN_POINT('Ctrl Pts',(-0.00269211290247009,-0.0251033241283995,
-0.0108518651181595));
#36925=CARTESIAN_POINT('Ctrl Pts',(-0.00270105766485107,-0.0251044383085421,
-0.0108702101517136));
#36926=CARTESIAN_POINT('Ctrl Pts',(-0.0027362554494885,-0.0251089552167848,
-0.0109443080465254));
#36927=CARTESIAN_POINT('Ctrl Pts',(-0.00276097360798209,-0.0251124342920514,
-0.0110007697374631));
#36928=CARTESIAN_POINT('Ctrl Pts',(-0.00285445578057964,-0.0251268160190748,
-0.0112335697435483));
#36929=CARTESIAN_POINT('Ctrl Pts',(-0.00290820053023947,-0.0251381068496403,
-0.0114154675499832));
#36930=CARTESIAN_POINT('Ctrl Pts',(-0.00296704862807839,-0.0251559913789531,
-0.0117170064762106));
#36931=CARTESIAN_POINT('Ctrl Pts',(-0.00298279797073649,-0.0251627449453282,
-0.0118340366376069));
#36932=CARTESIAN_POINT('Ctrl Pts',(-0.00299563347764602,-0.0251722923041128,
-0.0120053428824403));
#36933=CARTESIAN_POINT('Ctrl Pts',(-0.00299820942203873,-0.0251752405590099,
-0.0120590864430118));
#36934=CARTESIAN_POINT('Ctrl Pts',(-0.00299990679639111,-0.0251796056149532,
-0.0121399208547089));
#36935=CARTESIAN_POINT('Ctrl Pts',(-0.00300010886243288,-0.0251810549876021,
-0.0121669760527427));
#36936=CARTESIAN_POINT('Ctrl Pts',(-0.00299981141119672,-0.0251836644797591,
-0.0122160659536202));
#36937=CARTESIAN_POINT('Ctrl Pts',(-0.00299943511963678,-0.0251848282947188,
-0.0122380992431623));
#36938=CARTESIAN_POINT('Ctrl Pts',(-0.00299809319768953,-0.0251873351886208,
-0.0122858506354184));
#36939=CARTESIAN_POINT('Ctrl Pts',(-0.00299703932724928,-0.0251886754672274,
-0.0123115646102796));
#36940=CARTESIAN_POINT('Ctrl Pts',(-0.00299319585616863,-0.0251923685214541,
-0.0123828970990189));
#36941=CARTESIAN_POINT('Ctrl Pts',(-0.0029896944846547,-0.0251946995049771,
-0.0124284710620837));
#36942=CARTESIAN_POINT('Ctrl Pts',(-0.00296606136054852,-0.0252066824336097,
-0.0126651350908047));
#36943=CARTESIAN_POINT('Ctrl Pts',(-0.00292864567160056,-0.0252157967230421,
-0.0128540558199733));
#36944=CARTESIAN_POINT('Ctrl Pts',(-0.00283730973855783,-0.025230852476253,
-0.0131584290691307));
#36945=CARTESIAN_POINT('Ctrl Pts',(-0.00279368240071036,-0.0252367958495722,
-0.0132763609846854));
#36946=CARTESIAN_POINT('Ctrl Pts',(-0.00272512555053885,-0.0252451244149487,
-0.0134310795476146));
#36947=CARTESIAN_POINT('Ctrl Pts',(-0.00270658974067497,-0.0252472991516676,
-0.0134705632583707));
#36948=CARTESIAN_POINT('Ctrl Pts',(-0.00267307302553228,-0.0252511271985513,
-0.0135380905444445));
#36949=CARTESIAN_POINT('Ctrl Pts',(-0.00265849464954566,-0.0252527616163077,
-0.0135663265130125));
#36950=CARTESIAN_POINT('Ctrl Pts',(-0.00263615882656397,-0.0252552293160507,
-0.0136079516805647));
#36951=CARTESIAN_POINT('Ctrl Pts',(-0.0026287414569832,-0.0252560431686659,
-0.0136215218173752));
#36952=CARTESIAN_POINT('Ctrl Pts',(-0.00261577632345885,-0.0252574572020928,
-0.013644811920748));
#36953=CARTESIAN_POINT('Ctrl Pts',(-0.00261027858707579,-0.0252580543004693,
-0.0136545591172496));
#36954=CARTESIAN_POINT('Ctrl Pts',(-0.00259718858612093,-0.0252594702163244,
-0.0136774665084357));
#36955=CARTESIAN_POINT('Ctrl Pts',(-0.00258955090250267,-0.0252602918072985,
-0.0136905997748071));
#36956=CARTESIAN_POINT('Ctrl Pts',(-0.00256634944299513,-0.0252627727798938,
-0.0137298071533415));
#36957=CARTESIAN_POINT('Ctrl Pts',(-0.00255048961236525,-0.0252644491935699,
-0.0137557028623684));
#36958=CARTESIAN_POINT('Ctrl Pts',(-0.00241664039323987,-0.025278412240182,
-0.0139669805002835));
#36959=CARTESIAN_POINT('Ctrl Pts',(-0.00227900709992473,-0.0252915671254282,
-0.0141391181993388));
#36960=CARTESIAN_POINT('Ctrl Pts',(-0.00204875484969811,-0.0253106048893962,
-0.0143699130791668));
#36961=CARTESIAN_POINT('Ctrl Pts',(-0.00196974481189574,-0.0253167325711406,
-0.014441113337618));
#36962=CARTESIAN_POINT('Ctrl Pts',(-0.00183206378602863,-0.0253266972549476,
-0.0145525227457129));
#36963=CARTESIAN_POINT('Ctrl Pts',(-0.00177544746967256,-0.0253306141489884,
-0.0145951099585081));
#36964=CARTESIAN_POINT('Ctrl Pts',(-0.00169281252376824,-0.0253360802372307,
-0.0146528036382158));
#36965=CARTESIAN_POINT('Ctrl Pts',(-0.00166799560278297,-0.02533769119215,
-0.0146695830318676));
#36966=CARTESIAN_POINT('Ctrl Pts',(-0.00162423459617831,-0.0253404798241438,
-0.0146982254388942));
#36967=CARTESIAN_POINT('Ctrl Pts',(-0.00160540182590532,-0.0253416635086042,
-0.0147102534743738));
#36968=CARTESIAN_POINT('Ctrl Pts',(-0.00156601260719648,-0.0253441060270273,
-0.014734795168874));
#36969=CARTESIAN_POINT('Ctrl Pts',(-0.00154543640099061,-0.0253453635517764,
-0.0147472741812628));
#36970=CARTESIAN_POINT('Ctrl Pts',(-0.00149120137962799,-0.0253486317232652,
-0.0147792803514276));
#36971=CARTESIAN_POINT('Ctrl Pts',(-0.00145730840968821,-0.0253506279964612,
-0.0147984028880236));
#36972=CARTESIAN_POINT('Ctrl Pts',(-0.00127480414179758,-0.0253611501840864,
-0.0148967415019382));
#36973=CARTESIAN_POINT('Ctrl Pts',(-0.00112008471889298,-0.0253692578100808,
-0.0149640024830146));
#36974=CARTESIAN_POINT('Ctrl Pts',(-0.000840686702085648,-0.0253832675895954,
-0.0150584300265544));
#36975=CARTESIAN_POINT('Ctrl Pts',(-0.000718405481583358,-0.0253892092954031,
-0.0150913111756311));
#36976=CARTESIAN_POINT('Ctrl Pts',(-0.000500752380560026,-0.0253999333296747,
-0.0151353091091413));
#36977=CARTESIAN_POINT('Ctrl Pts',(-0.000406242947278311,-0.0254046394816158,
-0.0151497556815451));
#36978=CARTESIAN_POINT('Ctrl Pts',(-0.000288784314962083,-0.02541071732613,
-0.0151620066938834));
#36979=CARTESIAN_POINT('Ctrl Pts',(-0.000266329848170264,-0.0254118895287571,
-0.0151640930537761));
#36980=CARTESIAN_POINT('Ctrl Pts',(-0.000230329878603105,-0.0254137883119842,
-0.0151670290224538));
#36981=CARTESIAN_POINT('Ctrl Pts',(-0.000216798042904016,-0.0254145064304734,
-0.0151680402343232));
#36982=CARTESIAN_POINT('Ctrl Pts',(-0.00019054441623753,-0.0254159089827382,
-0.0151698231025514));
#36983=CARTESIAN_POINT('Ctrl Pts',(-0.000177823794222554,-0.0254165928379668,
-0.0151706055488515));
#36984=CARTESIAN_POINT('Ctrl Pts',(-0.000145879985982581,-0.0254183202401005,
-0.015172366179774));
#36985=CARTESIAN_POINT('Ctrl Pts',(-0.000126651793888489,-0.0254193692054502,
-0.0151732404444429));
#36986=CARTESIAN_POINT('Ctrl Pts',(-5.51238562221319E-5,-0.025423302080105,
-0.0151758031939177));
#36987=CARTESIAN_POINT('Ctrl Pts',(-2.7934491336597E-6,-0.0254262404455392,
-0.0151763081965697));
#36988=CARTESIAN_POINT('Ctrl Pts',(0.000225262751348615,-0.0254392370628772,
-0.0151725432159265));
#36989=CARTESIAN_POINT('Ctrl Pts',(0.000400404943875442,-0.0254496910328864,
-0.0151542030397294));
#36990=CARTESIAN_POINT('Ctrl Pts',(0.000684481379551118,-0.02546663004315,
-0.0150989338718602));
#36991=CARTESIAN_POINT('Ctrl Pts',(0.000794716739886117,-0.0254732041795396,
-0.0150709083107126));
#36992=CARTESIAN_POINT('Ctrl Pts',(0.00097365225308281,-0.0254837826188235,
-0.0150144223723092));
#36993=CARTESIAN_POINT('Ctrl Pts',(0.00104335707163828,-0.0254878805338421,
-0.014989548448926));
#36994=CARTESIAN_POINT('Ctrl Pts',(0.00114033744010028,-0.0254935477396581,
-0.0149508409471969));
#36995=CARTESIAN_POINT('Ctrl Pts',(0.00116842702581515,-0.0254951851776466,
-0.0149391311176765));
#36996=CARTESIAN_POINT('Ctrl Pts',(0.00121689288194461,-0.0254980042721968,
-0.0149180557390365));
#36997=CARTESIAN_POINT('Ctrl Pts',(0.0012373509575093,-0.0254991923230563,
-0.0149088855258758));
#36998=CARTESIAN_POINT('Ctrl Pts',(0.00127938618555014,-0.0255016300766138,
-0.0148894747255589));
#36999=CARTESIAN_POINT('Ctrl Pts',(0.00130094773824838,-0.0255028786547219,
-0.0148792040502657));
#37000=CARTESIAN_POINT('Ctrl Pts',(0.00135652620999398,-0.0255060935888792,
-0.0148519107188751));
#37001=CARTESIAN_POINT('Ctrl Pts',(0.00139034660701288,-0.025508046460882,
-0.0148344964023408));
#37002=CARTESIAN_POINT('Ctrl Pts',(0.00155381147988048,-0.0255174815104599,
-0.0147463548017938));
#37003=CARTESIAN_POINT('Ctrl Pts',(0.0016784503875721,-0.025524650410476,
-0.0146667604106928));
#37004=CARTESIAN_POINT('Ctrl Pts',(0.00193442859958337,-0.0255398989783619,
-0.0144753212762969));
#37005=CARTESIAN_POINT('Ctrl Pts',(0.00206301358235341,-0.0255479049119119,
-0.0143606957851303));
#37006=CARTESIAN_POINT('Ctrl Pts',(0.00221608468519604,-0.0255587930129314,
-0.0141986161868936));
#37007=CARTESIAN_POINT('Ctrl Pts',(0.00225014989421621,-0.0255613179393576,
-0.0141606520412306));
#37008=CARTESIAN_POINT('Ctrl Pts',(0.00230635314405614,-0.0255656968316467,
-0.0140947086696502));
#37009=CARTESIAN_POINT('Ctrl Pts',(0.00232899052884989,-0.0255675236849599,
-0.0140671686263753));
#37010=CARTESIAN_POINT('Ctrl Pts',(0.00236117831096757,-0.0255702255922654,
-0.0140265554917247));
#37011=CARTESIAN_POINT('Ctrl Pts',(0.00237112283675339,-0.0255710754680737,
-0.0140137972841784));
#37012=CARTESIAN_POINT('Ctrl Pts',(0.00238846137611719,-0.0255725853559766,
-0.0139911780923155));
#37013=CARTESIAN_POINT('Ctrl Pts',(0.00239589852966817,-0.0255732424178969,
-0.0139813510361035));
#37014=CARTESIAN_POINT('Ctrl Pts',(0.00241232522660593,-0.0255747150410371,
-0.0139593654460252));
#37015=CARTESIAN_POINT('Ctrl Pts',(0.00242128343066518,-0.0255755325605873,
-0.0139471847492884));
#37016=CARTESIAN_POINT('Ctrl Pts',(0.00244719459557312,-0.025577938527509,
-0.0139113888480944));
#37017=CARTESIAN_POINT('Ctrl Pts',(0.00246389642761711,-0.0255795421838436,
-0.0138875948983747));
#37018=CARTESIAN_POINT('Ctrl Pts',(0.00258167008182509,-0.0255912167304728,
-0.0137145153503037));
#37019=CARTESIAN_POINT('Ctrl Pts',(0.00266944295109022,-0.0256018922760762,
-0.0135566385589283));
#37020=CARTESIAN_POINT('Ctrl Pts',(0.00279629737366019,-0.0256202802424622,
-0.0132705365083005));
#37021=CARTESIAN_POINT('Ctrl Pts',(0.00284198151377146,-0.0256280164503185,
-0.0131457792102502));
#37022=CARTESIAN_POINT('Ctrl Pts',(0.00290213466171848,-0.0256401459853748,
-0.0129402159943772));
#37023=CARTESIAN_POINT('Ctrl Pts',(0.00292182033244563,-0.025644673658923,
-0.0128611295686992));
#37024=CARTESIAN_POINT('Ctrl Pts',(0.00294461775445603,-0.0256508129837517,
-0.012750498823272));
#37025=CARTESIAN_POINT('Ctrl Pts',(0.00295048633783433,-0.0256525091049688,
-0.0127195643178293));
#37026=CARTESIAN_POINT('Ctrl Pts',(0.00295972836828079,-0.0256553963747003,
-0.012666280142606));
#37027=CARTESIAN_POINT('Ctrl Pts',(0.00296333814259151,-0.0256565947877827,
-0.0126439746441169));
#37028=CARTESIAN_POINT('Ctrl Pts',(0.00296977795881066,-0.0256588784301815,
-0.0126011169283942));
#37029=CARTESIAN_POINT('Ctrl Pts',(0.00297264748124694,-0.0256599648234059,
-0.0125805720412986));
#37030=CARTESIAN_POINT('Ctrl Pts',(0.00297964611188767,-0.0256628101403707,
-0.0125263658700173));
#37031=CARTESIAN_POINT('Ctrl Pts',(0.00298341800666489,-0.0256645579799812,
-0.0124926610194363));
#37032=CARTESIAN_POINT('Ctrl Pts',(0.00299550279743585,-0.0256710970114868,
-0.0123651455504515));
#37033=CARTESIAN_POINT('Ctrl Pts',(0.00299996891933946,-0.0256757716585713,
-0.0122710219335788));
#37034=CARTESIAN_POINT('Ctrl Pts',(0.00300005839134703,-0.0256890407294522,
-0.0119984770689181));
#37035=CARTESIAN_POINT('Ctrl Pts',(0.00298421101998347,-0.0256973590325867,
-0.01182046957932));
#37036=CARTESIAN_POINT('Ctrl Pts',(0.00293046389805818,-0.0257118587188384,
-0.0115215674536747));
#37037=CARTESIAN_POINT('Ctrl Pts',(0.00290057606449068,-0.0257179340604047,
-0.0113997338968926));
#37038=CARTESIAN_POINT('Ctrl Pts',(0.00285595038363327,-0.0257256060527422,
-0.0112570873867286));
#37039=CARTESIAN_POINT('Ctrl Pts',(0.00284846105331454,-0.0257268589024376,
-0.0112341245943821));
#37040=CARTESIAN_POINT('Ctrl Pts',(0.00283622121357359,-0.0257288573636554,
-0.0111980788392584));
#37041=CARTESIAN_POINT('Ctrl Pts',(0.0028316553774092,-0.0257295928826786,
-0.0111849337890719));
#37042=CARTESIAN_POINT('Ctrl Pts',(0.00282274332623996,-0.0257310106859931,
-0.0111598406120381));
#37043=CARTESIAN_POINT('Ctrl Pts',(0.00281841236550277,-0.0257316921274252,
-0.0111478876465119));
#37044=CARTESIAN_POINT('Ctrl Pts',(0.00280763254675204,-0.0257333695566859,
-0.0111187168120117));
#37045=CARTESIAN_POINT('Ctrl Pts',(0.00280110116921717,-0.0257343701544008,
-0.0111015301277763));
#37046=CARTESIAN_POINT('Ctrl Pts',(0.00277623917153101,-0.0257381189982614,
-0.0110378764710834));
#37047=CARTESIAN_POINT('Ctrl Pts',(0.00275690765318436,-0.0257409175230551,
-0.0109918115583913));
#37048=CARTESIAN_POINT('Ctrl Pts',(0.00270241336180105,-0.0257484753448215,
-0.0108705362081398));
#37049=CARTESIAN_POINT('Ctrl Pts',(0.00266526390332989,-0.0257533024823443,
-0.0107962672387901));
#37050=CARTESIAN_POINT('Ctrl Pts',(0.00250215346147765,-0.0257730451064716,
-0.0105014219740259));
#37051=CARTESIAN_POINT('Ctrl Pts',(0.00235147810862052,-0.0257880719220853,
-0.010295671813178));
#37052=CARTESIAN_POINT('Ctrl Pts',(0.00214563544523808,-0.0258045804786426,
-0.0100786452832899));
#37053=CARTESIAN_POINT('Ctrl Pts',(0.00211387330061941,-0.0258070390703807,
-0.0100466344531266));
#37054=CARTESIAN_POINT('Ctrl Pts',(0.0020629634525884,-0.0258108451584988,
-0.00999758856376631));
#37055=CARTESIAN_POINT('Ctrl Pts',(0.00204429949412708,-0.0258122134488246,
-0.009980062986314));
#37056=CARTESIAN_POINT('Ctrl Pts',(0.00200915363851221,-0.0258147410317691,
-0.00994789739350922));
#37057=CARTESIAN_POINT('Ctrl Pts',(0.00199273041812558,-0.0258159028462061,
-0.00993319608586866));
#37058=CARTESIAN_POINT('Ctrl Pts',(0.00195567135584683,-0.0258184825632515,
-0.00990075106743063));
#37059=CARTESIAN_POINT('Ctrl Pts',(0.00193495296533104,-0.0258198964657749,
-0.00988310435905266));
#37060=CARTESIAN_POINT('Ctrl Pts',(0.00187191042619904,-0.0258241170346503,
-0.00983087172270445));
#37061=CARTESIAN_POINT('Ctrl Pts',(0.00182887747601515,-0.0258268895016612,
-0.00979715725318942));
#37062=CARTESIAN_POINT('Ctrl Pts',(0.00167250167914293,-0.0258366197536096,
-0.00968139734532663));
#37063=CARTESIAN_POINT('Ctrl Pts',(0.00155436749252544,-0.0258433400581867,
-0.00960612215275029));
#37064=CARTESIAN_POINT('Ctrl Pts',(0.0012798010660304,-0.0258581836513316,
-0.00945705430554906));
#37065=CARTESIAN_POINT('Ctrl Pts',(0.0011213901356715,-0.0258662385396847,
-0.00938798039854426));
#37066=CARTESIAN_POINT('Ctrl Pts',(0.000904484498255154,-0.0258775636091151,
-0.00931489381682784));
#37067=CARTESIAN_POINT('Ctrl Pts',(0.000850539917110885,-0.0258804049318105,
-0.0092983956548905));
#37068=CARTESIAN_POINT('Ctrl Pts',(0.000777092206148273,-0.02588434524141,
-0.00927817851820979));
#37069=CARTESIAN_POINT('Ctrl Pts',(0.000757967793312922,-0.0258853777158257,
-0.00927311731098472));
#37070=CARTESIAN_POINT('Ctrl Pts',(0.000727462656841946,-0.0258870368974471,
-0.00926536624802472));
#37071=CARTESIAN_POINT('Ctrl Pts',(0.000716113542861952,-0.025887656871205,
-0.00926255307835635));
#37072=CARTESIAN_POINT('Ctrl Pts',(0.000692016620857422,-0.0258889794760447,
-0.00925672934873053));
#37073=CARTESIAN_POINT('Ctrl Pts',(0.000679265057995674,-0.0258896830814018,
-0.00925373581236286));
#37074=CARTESIAN_POINT('Ctrl Pts',(0.000646636301346663,-0.0258914922109695,
-0.00924630104767092));
#37075=CARTESIAN_POINT('Ctrl Pts',(0.000626732973111169,-0.0258926040258825,
-0.00924197861950552));
#37076=CARTESIAN_POINT('Ctrl Pts',(0.000541028178600831,-0.025897422411502,
-0.00922427789654304));
#37077=CARTESIAN_POINT('Ctrl Pts',(0.000474835375667756,-0.0259012213897143,
-0.00921290898481249));
#37078=CARTESIAN_POINT('Ctrl Pts',(0.000273376739088949,-0.0259129092387133,
-0.00918523144127569));
#37079=CARTESIAN_POINT('Ctrl Pts',(0.000137329575514236,-0.0259209649263144,
-0.00917590451347279));
#37080=CARTESIAN_POINT('Ctrl Pts',(-0.000176554041602739,-0.0259393958263076,
-0.00917578694708795));
#37081=CARTESIAN_POINT('Ctrl Pts',(-0.000353905770131149,-0.0259496794901596,
-0.00919150501026625));
#37082=CARTESIAN_POINT('Ctrl Pts',(-0.000570080131534526,-0.0259618096690587,
-0.00923021858061489));
#37083=CARTESIAN_POINT('Ctrl Pts',(-0.000611160970754606,-0.0259640980652013,
-0.00923846708717254));
#37084=CARTESIAN_POINT('Ctrl Pts',(-0.000678424191795633,-0.0259678181641809,
-0.00925344497899387));
#37085=CARTESIAN_POINT('Ctrl Pts',(-0.000704711413619019,-0.0259692652466403,
-0.0092596722927942));
#37086=CARTESIAN_POINT('Ctrl Pts',(-0.000752281149067618,-0.0259718723268269,
-0.00927162214038809));
#37087=CARTESIAN_POINT('Ctrl Pts',(-0.000773591333962172,-0.0259730359873158,
-0.00927722568710357));
#37088=CARTESIAN_POINT('Ctrl Pts',(-0.000819685074685722,-0.0259755444342235,
-0.0092898906478453));
#37089=CARTESIAN_POINT('Ctrl Pts',(-0.000844443398024073,-0.0259768863923803,
-0.00929703766635584));
#37090=CARTESIAN_POINT('Ctrl Pts',(-0.000914265194417583,-0.0259806574821131,
-0.00931817149203214));
#37091=CARTESIAN_POINT('Ctrl Pts',(-0.000959095978073966,-0.0259830627481871,
-0.00933290388586636));
#37092=CARTESIAN_POINT('Ctrl Pts',(-0.00106021207072405,-0.025988463978135,
-0.00936879718744386));
#37093=CARTESIAN_POINT('Ctrl Pts',(-0.00111624648618063,-0.0259914398030971,
-0.00939060502486205));
#37094=CARTESIAN_POINT('Ctrl Pts',(-0.00131377751964363,-0.0260019250870548,
-0.00947440103939878));
#37095=CARTESIAN_POINT('Ctrl Pts',(-0.00145109857980862,-0.0260091922277864,
-0.00954561175001733));
#37096=CARTESIAN_POINT('Ctrl Pts',(-0.00170668862246993,-0.0260234664260622,
-0.00970428678456888));
#37097=CARTESIAN_POINT('Ctrl Pts',(-0.00182522328655958,-0.0260304530712585,
-0.0097904855488409));
#37098=CARTESIAN_POINT('Ctrl Pts',(-0.00196064150094307,-0.0260394671347499,
-0.00990498454487402));
#37099=CARTESIAN_POINT('Ctrl Pts',(-0.00198398858325478,-0.0260410620005325,
-0.00992535354261215));
#37100=CARTESIAN_POINT('Ctrl Pts',(-0.0020183975185759,-0.0260434814093708,
-0.0099563249625849));
#37101=CARTESIAN_POINT('Ctrl Pts',(-0.00202970104302239,-0.0260442876217778,
-0.00996665701187283));
#37102=CARTESIAN_POINT('Ctrl Pts',(-0.00205003983561637,-0.0260457601625911,
-0.00998553565174353));
#37103=CARTESIAN_POINT('Ctrl Pts',(-0.00205910175249264,-0.0260464243535992,
-0.00999405251015095));
#37104=CARTESIAN_POINT('Ctrl Pts',(-0.00207971885800195,-0.0260479540977671,
-0.0100136723835053));
#37105=CARTESIAN_POINT('Ctrl Pts',(-0.00209123822985529,-0.0260488222962515,
-0.0100248118111333));
#37106=CARTESIAN_POINT('Ctrl Pts',(-0.00212746526468485,-0.026051594100147,
-0.0100604100142113));
#37107=CARTESIAN_POINT('Ctrl Pts',(-0.00215183651611916,-0.0260535207837809,
-0.010085205516918));
#37108=CARTESIAN_POINT('Ctrl Pts',(-0.00220969227820255,-0.0260582345962579,
-0.0101461519148889));
#37109=CARTESIAN_POINT('Ctrl Pts',(-0.00224272734787067,-0.0260610445306258,
-0.0101827147454583));
#37110=CARTESIAN_POINT('Ctrl Pts',(-0.00237889231780473,-0.0260730839658959,
-0.0103410935989622));
#37111=CARTESIAN_POINT('Ctrl Pts',(-0.0024731143470861,-0.0260825636264007,
-0.0104702223962119));
#37112=CARTESIAN_POINT('Ctrl Pts',(-0.00264146276556717,-0.02610136652058,
-0.0107444302161605));
#37113=CARTESIAN_POINT('Ctrl Pts',(-0.00271497235936262,-0.0261106510162668,
-0.0108892940913171));
#37114=CARTESIAN_POINT('Ctrl Pts',(-0.00279095479310238,-0.0261216422173249,
-0.0110749245195623));
#37115=CARTESIAN_POINT('Ctrl Pts',(-0.00280481021886816,-0.0261237231689978,
-0.0111107182582934));
#37116=CARTESIAN_POINT('Ctrl Pts',(-0.00282619413579598,-0.0261270667385175,
-0.0111692745537152));
#37117=CARTESIAN_POINT('Ctrl Pts',(-0.00283414303494523,-0.0261283429465237,
-0.0111918780119223));
#37118=CARTESIAN_POINT('Ctrl Pts',(-0.00284899790785426,-0.0261307952602463,
-0.0112357933590812));
#37119=CARTESIAN_POINT('Ctrl Pts',(-0.00285593760926345,-0.026131972394603,
-0.0112570920801973));
#37120=CARTESIAN_POINT('Ctrl Pts',(-0.0028716908118266,-0.0261347219926009,
-0.0113073443704551));
#37121=CARTESIAN_POINT('Ctrl Pts',(-0.00288030610176168,-0.0261362880172093,
-0.0113363577821861));
#37122=CARTESIAN_POINT('Ctrl Pts',(-0.00290814704702146,-0.0261415758641783,
-0.0114355957033733));
#37123=CARTESIAN_POINT('Ctrl Pts',(-0.00292525554449036,-0.0261452312859027,
-0.0115063896501784));
#37124=CARTESIAN_POINT('Ctrl Pts',(-0.00296187104492923,-0.0261542941812586,
-0.011686357519684));
#37125=CARTESIAN_POINT('Ctrl Pts',(-0.00297793404631481,-0.0261596099782093,
-0.0117961205545347));
#37126=CARTESIAN_POINT('Ctrl Pts',(-0.00300300929215862,-0.026172885761028,
-0.0120743011820653));
#37127=CARTESIAN_POINT('Ctrl Pts',(-0.00300397348118124,-0.026180752556728,
-0.0122430429054789));
#37128=CARTESIAN_POINT('Ctrl Pts',(-0.00298594305059408,-0.0261920889618934,
-0.0124724044340214));
#37129=CARTESIAN_POINT('Ctrl Pts',(-0.00297922101199773,-0.0261951828448286,
-0.0125336796833466));
#37130=CARTESIAN_POINT('Ctrl Pts',(-0.00296776744903848,-0.0261994210259704,
-0.012614912524563));
#37131=CARTESIAN_POINT('Ctrl Pts',(-0.00296471149164684,-0.0262004852954412,
-0.0126350943706082));
#37132=CARTESIAN_POINT('Ctrl Pts',(-0.00295956235644654,-0.0262021827739815,
-0.0126669033729147));
#37133=CARTESIAN_POINT('Ctrl Pts',(-0.00295760598170671,-0.0262028086832761,
-0.0126785523780043));
#37134=CARTESIAN_POINT('Ctrl Pts',(-0.00295335953302141,-0.0262041293172166,
-0.0127029541729565));
#37135=CARTESIAN_POINT('Ctrl Pts',(-0.00295105556535897,-0.0262048248529811,
-0.0127157041054001));
#37136=CARTESIAN_POINT('Ctrl Pts',(-0.00294503817338269,-0.0262065897259424,
-0.0127478137273511));
#37137=CARTESIAN_POINT('Ctrl Pts',(-0.00294121641468453,-0.0262076647992908,
-0.012767152322083));
#37138=CARTESIAN_POINT('Ctrl Pts',(-0.0029248005745554,-0.0262121005598569,
-0.0128461186396004));
#37139=CARTESIAN_POINT('Ctrl Pts',(-0.00291058216053183,-0.0262155371721572,
-0.0129053905350537));
#37140=CARTESIAN_POINT('Ctrl Pts',(-0.0028644813789978,-0.026225584799816,
-0.013074661966317));
#37141=CARTESIAN_POINT('Ctrl Pts',(-0.00282809387749655,-0.0262323197133492,
-0.0131833222169843));
#37142=CARTESIAN_POINT('Ctrl Pts',(-0.00270814621452849,-0.0262513234098642,
-0.013483314142516));
#37143=CARTESIAN_POINT('Ctrl Pts',(-0.00261070565950489,-0.0262634973326678,
-0.0136684177475832));
#37144=CARTESIAN_POINT('Ctrl Pts',(-0.00246980038471531,-0.0262775004239674,
-0.0138794136081842));
#37145=CARTESIAN_POINT('Ctrl Pts',(-0.00244392541500113,-0.0262799583167868,
-0.0139163303977391));
#37146=CARTESIAN_POINT('Ctrl Pts',(-0.00240207376419642,-0.0262837628750102,
-0.0139732670575144));
#37147=CARTESIAN_POINT('Ctrl Pts',(-0.00238665675298442,-0.0262851303456879,
-0.013993688326132));
#37148=CARTESIAN_POINT('Ctrl Pts',(-0.00235748716780589,-0.0262876561247282,
-0.0140313152896178));
#37149=CARTESIAN_POINT('Ctrl Pts',(-0.00234380281635463,-0.0262888169576663,
-0.0140485714671085));
#37150=CARTESIAN_POINT('Ctrl Pts',(-0.00231280599341356,-0.0262913940876831,
-0.0140867869149724));
#37151=CARTESIAN_POINT('Ctrl Pts',(-0.00229539606198751,-0.0262928063950667,
-0.0141076648397084));
#37152=CARTESIAN_POINT('Ctrl Pts',(-0.00224219520198089,-0.0262970205281855,
-0.0141697283015315));
#37153=CARTESIAN_POINT('Ctrl Pts',(-0.00220556131244758,-0.0262997882604862,
-0.014210177905968));
#37154=CARTESIAN_POINT('Ctrl Pts',(-0.00207225391405662,-0.0263094331570109,
-0.014349533628757));
#37155=CARTESIAN_POINT('Ctrl Pts',(-0.00196986552819778,-0.026316079143308,
-0.0144427357986513));
#37156=CARTESIAN_POINT('Ctrl Pts',(-0.00172838896540962,-0.0263307112070987,
-0.0146337876498034));
#37157=CARTESIAN_POINT('Ctrl Pts',(-0.0015866932847853,-0.0263386308302992,
-0.0147275522000348));
#37158=CARTESIAN_POINT('Ctrl Pts',(-0.00138507930899339,-0.0263499624349665,
-0.0148376515208313));
#37159=CARTESIAN_POINT('Ctrl Pts',(-0.00133146224695846,-0.0263529833646708,
-0.0148648720590887));
#37160=CARTESIAN_POINT('Ctrl Pts',(-0.00125876347347922,-0.0263571353441502,
-0.0148990726469535));
#37161=CARTESIAN_POINT('Ctrl Pts',(-0.00124037374313603,-0.0263581903017766,
-0.0149074978647041));
#37162=CARTESIAN_POINT('Ctrl Pts',(-0.00121115133263792,-0.026359876184706,
-0.0149205301308951));
#37163=CARTESIAN_POINT('Ctrl Pts',(-0.00120037401867651,-0.0263604999658543,
-0.0149252606292993));
#37164=CARTESIAN_POINT('Ctrl Pts',(-0.00117763892437462,-0.0263618206533458,
-0.0149350806155248));
#37165=CARTESIAN_POINT('Ctrl Pts',(-0.00116567548548739,-0.0263625184196523,
-0.0149401560076386));
#37166=CARTESIAN_POINT('Ctrl Pts',(-0.00113532685196329,-0.0263642948901051,
-0.0149527991315181));
#37167=CARTESIAN_POINT('Ctrl Pts',(-0.00111689887680067,-0.0263653794697229,
-0.0149602620466994));
#37168=CARTESIAN_POINT('Ctrl Pts',(-0.00104031175263584,-0.0263699072150745,
-0.0149903954986541));
#37169=CARTESIAN_POINT('Ctrl Pts',(-0.000981529315005994,-0.0263734300705311,
-0.0150114300559489));
#37170=CARTESIAN_POINT('Ctrl Pts',(-0.000808601434267826,-0.0263838472663003,
-0.0150672887774806));
#37171=CARTESIAN_POINT('Ctrl Pts',(-0.000692982526473934,-0.0263908747727479,
-0.0150971558521233));
#37172=CARTESIAN_POINT('Ctrl Pts',(-0.000378079364101146,-0.0264097470162851,
-0.0151587520706844));
#37173=CARTESIAN_POINT('Ctrl Pts',(-0.000176839674301235,-0.0264214896326742,
-0.0151774158198483));
#37174=CARTESIAN_POINT('Ctrl Pts',(7.02431736514861E-5,-0.0264351319563392,
-0.0151753755308247));
#37175=CARTESIAN_POINT('Ctrl Pts',(0.000115701800131155,-0.0264376123034122,
-0.0151739662259297));
#37176=CARTESIAN_POINT('Ctrl Pts',(0.000186767158066899,-0.0264414447803659,
-0.0151701442025625));
#37177=CARTESIAN_POINT('Ctrl Pts',(0.00021240346732146,-0.0264428181529634,
-0.0151684349285025));
#37178=CARTESIAN_POINT('Ctrl Pts',(0.000259992804911569,-0.0264453512504799,
-0.0151646473269047));
#37179=CARTESIAN_POINT('Ctrl Pts',(0.000281950823223422,-0.0264465135630514,
-0.0151626558984039));
#37180=CARTESIAN_POINT('Ctrl Pts',(0.000330875203223684,-0.0264490896074626,
-0.0151576744762023));
#37181=CARTESIAN_POINT('Ctrl Pts',(0.000357827136870877,-0.026450499415262,
-0.0151545603566988));
#37182=CARTESIAN_POINT('Ctrl Pts',(0.000438449604974007,-0.0264546911888428,
-0.0151441348752801));
#37183=CARTESIAN_POINT('Ctrl Pts',(0.00049196938162317,-0.026457439718098,
-0.0151357350788764));
#37184=CARTESIAN_POINT('Ctrl Pts',(0.000750342620371381,-0.0264705865611251,
-0.0150879817748392));
#37185=CARTESIAN_POINT('Ctrl Pts',(0.000950936046794013,-0.0264803698107777,
-0.0150287873051669));
#37186=CARTESIAN_POINT('Ctrl Pts',(0.00127370367310936,-0.026496950193539,
-0.014895675239027));
#37187=CARTESIAN_POINT('Ctrl Pts',(0.0013996948785352,-0.0265036754519913,
-0.0148330322021753));
#37188=CARTESIAN_POINT('Ctrl Pts',(0.0015476722691891,-0.0265123999897581,
-0.0147460052309575));
#37189=CARTESIAN_POINT('Ctrl Pts',(0.00157427643719887,-0.0265140033424187,
-0.0147297961258277));
#37190=CARTESIAN_POINT('Ctrl Pts',(0.00161361118385055,-0.0265164336386123,
-0.0147049825426861));
#37191=CARTESIAN_POINT('Ctrl Pts',(0.00162653661688444,-0.026517242052961,
-0.0146966893504206));
#37192=CARTESIAN_POINT('Ctrl Pts',(0.00164984013887743,-0.0265187184946581,
-0.0146814835453238));
#37193=CARTESIAN_POINT('Ctrl Pts',(0.00166023960202947,-0.0265193843762967,
-0.0146746049602128));
#37194=CARTESIAN_POINT('Ctrl Pts',(0.00168394093277497,-0.0265209180085231,
-0.0146587147549854));
#37195=CARTESIAN_POINT('Ctrl Pts',(0.00169721353488977,-0.0265217884123444,
-0.0146496609449121));
#37196=CARTESIAN_POINT('Ctrl Pts',(0.00173901366532376,-0.0265245648314106,
-0.0146206525558815));
#37197=CARTESIAN_POINT('Ctrl Pts',(0.00176726602409027,-0.0265264938684584,
-0.0146003083992853));
#37198=CARTESIAN_POINT('Ctrl Pts',(0.00183468362650029,-0.0265312129742921,
-0.0145499572950523));
#37199=CARTESIAN_POINT('Ctrl Pts',(0.00187347466118594,-0.0265340257695353,
-0.0145194671895346));
#37200=CARTESIAN_POINT('Ctrl Pts',(0.00203486975796642,-0.0265460922967348,
-0.0143860409479122));
#37201=CARTESIAN_POINT('Ctrl Pts',(0.00214988197452682,-0.026555595180676,
-0.0142743364450816));
#37202=CARTESIAN_POINT('Ctrl Pts',(0.00236110692921097,-0.0265742987755129,
-0.0140335019693678));
#37203=CARTESIAN_POINT('Ctrl Pts',(0.00245696744520741,-0.0265834669232397,
-0.0139047277797845));
#37204=CARTESIAN_POINT('Ctrl Pts',(0.00256244299038546,-0.026594349622514,
-0.0137364157340204));
#37205=CARTESIAN_POINT('Ctrl Pts',(0.00258217329610803,-0.0265964278082052,
-0.0137035477862005));
#37206=CARTESIAN_POINT('Ctrl Pts',(0.00261321642752148,-0.0265997699390877,
-0.0136495137347939));
#37207=CARTESIAN_POINT('Ctrl Pts',(0.00262491432953693,-0.0266010473681421,
-0.0136285748777071));
#37208=CARTESIAN_POINT('Ctrl Pts',(0.0026470791993611,-0.0266035041173972,
-0.0135877584686789));
#37209=CARTESIAN_POINT('Ctrl Pts',(0.00265757644586538,-0.0266046844387135,
-0.0135678992634247));
#37210=CARTESIAN_POINT('Ctrl Pts',(0.00268175869663563,-0.0266074448251034,
-0.013520879361923));
#37211=CARTESIAN_POINT('Ctrl Pts',(0.0026952558125526,-0.0266090183668267,
-0.0134936245269545));
#37212=CARTESIAN_POINT('Ctrl Pts',(0.00273996377325103,-0.0266143505566001,
-0.0133997837356761));
#37213=CARTESIAN_POINT('Ctrl Pts',(0.00276914091869512,-0.0266180414194744,
-0.0133322558320741));
#37214=CARTESIAN_POINT('Ctrl Pts',(0.00283658452337156,-0.0266272156818553,
-0.0131589263758013));
#37215=CARTESIAN_POINT('Ctrl Pts',(0.00287143786491108,-0.0266326043944009,
-0.0130519189387326));
#37216=CARTESIAN_POINT('Ctrl Pts',(0.00295440815394613,-0.0266480164384357,
-0.0127383324975869));
#37217=CARTESIAN_POINT('Ctrl Pts',(0.00298674724158532,-0.0266578551249714,
-0.0125283180125818));
#37218=CARTESIAN_POINT('Ctrl Pts',(0.00299806883616562,-0.0266701414401903,
-0.0122873988315587));
#37219=CARTESIAN_POINT('Ctrl Pts',(0.00299901552943678,-0.0266716528024666,
-0.0122581022274078));
#37220=CARTESIAN_POINT('Ctrl Pts',(0.00299970122819703,-0.0266736852041671,
-0.0122192542508606));
#37221=CARTESIAN_POINT('Ctrl Pts',(0.00299982412743131,-0.0266741867732736,
-0.0122097103670345));
#37222=CARTESIAN_POINT('Ctrl Pts',(0.00299996762782709,-0.0266751217604859,
-0.0121920042481002));
#37223=CARTESIAN_POINT('Ctrl Pts',(0.0030000004394171,-0.0266755539940525,
-0.0121838521580368));
#37224=CARTESIAN_POINT('Ctrl Pts',(0.00299999999556417,-0.0266759885990988,
-0.0121756901455692));
#37225=CARTESIAN_POINT('',(-0.0030008859025812,-0.0271782456277452,-0.0121752776264524));
#37226=CARTESIAN_POINT('Ctrl Pts',(0.00299999999556417,-0.0266759885990988,
-0.0121756901455692));
#37227=CARTESIAN_POINT('Ctrl Pts',(0.00299999959124405,-0.026676384495016,
-0.0121682551020984));
#37228=CARTESIAN_POINT('Ctrl Pts',(0.00299997154769017,-0.0266767819272223,
-0.0121608202951627));
#37229=CARTESIAN_POINT('Ctrl Pts',(0.00299984500965966,-0.0266776885879081,
-0.0121439247657658));
#37230=CARTESIAN_POINT('Ctrl Pts',(0.00299972939971157,-0.0266781987292689,
-0.0121344644467317));
#37231=CARTESIAN_POINT('Ctrl Pts',(0.00299921172118187,-0.026679853116644,
-0.0121039263214186));
#37232=CARTESIAN_POINT('Ctrl Pts',(0.00299863223187566,-0.0266810065230799,
-0.0120828526144914));
#37233=CARTESIAN_POINT('Ctrl Pts',(0.00299496888804635,-0.0266863243563261,
-0.0119865742101401));
#37234=CARTESIAN_POINT('Ctrl Pts',(0.00298927770430945,-0.0266906052947664,
-0.0119115004943302));
#37235=CARTESIAN_POINT('Ctrl Pts',(0.00296196053497696,-0.0267045689040371,
-0.0116713953060827));
#37236=CARTESIAN_POINT('Ctrl Pts',(0.00292942835960164,-0.0267144745978878,
-0.0115079176724795));
#37237=CARTESIAN_POINT('Ctrl Pts',(0.00285504456101083,-0.0267302086016848,
-0.0112488363902317));
#37238=CARTESIAN_POINT('Ctrl Pts',(0.00282148375743838,-0.0267361500012816,
-0.0111512207070386));
#37239=CARTESIAN_POINT('Ctrl Pts',(0.00275705406418017,-0.0267458503987208,
-0.0109911742109662));
#37240=CARTESIAN_POINT('Ctrl Pts',(0.00272892457493658,-0.0267496846736673,
-0.0109277413684892));
#37241=CARTESIAN_POINT('Ctrl Pts',(0.00268570262590721,-0.0267550491816169,
-0.0108387385833227));
#37242=CARTESIAN_POINT('Ctrl Pts',(0.00267239291374361,-0.0267566389265011,
-0.0108123319172534));
#37243=CARTESIAN_POINT('Ctrl Pts',(0.00264844841823185,-0.0267593942448047,
-0.0107665235867418));
#37244=CARTESIAN_POINT('Ctrl Pts',(0.00263798555238983,-0.0267605656713797,
-0.0107470350729112));
#37245=CARTESIAN_POINT('Ctrl Pts',(0.0026157857455541,-0.026762985550449,
-0.010706760147235));
#37246=CARTESIAN_POINT('Ctrl Pts',(0.00260401430233,-0.0267642326766404,
-0.0106859944760083));
#37247=CARTESIAN_POINT('Ctrl Pts',(0.00257251701811284,-0.0267674786159811,
-0.0106319449566617));
#37248=CARTESIAN_POINT('Ctrl Pts',(0.00255239268973123,-0.026769463093696,
-0.0105988978428446));
#37249=CARTESIAN_POINT('Ctrl Pts',(0.00244132880068725,-0.0267799675406711,
-0.0104242132930148));
#37250=CARTESIAN_POINT('Ctrl Pts',(0.0023392251403436,-0.026788066913517,
-0.0102900213220678));
#37251=CARTESIAN_POINT('Ctrl Pts',(0.00212285019202616,-0.0268033919536706,
-0.0100504416343587));
#37252=CARTESIAN_POINT('Ctrl Pts',(0.00201060542073186,-0.0268106183249926,
-0.00994396419309953));
#37253=CARTESIAN_POINT('Ctrl Pts',(0.0018530684175075,-0.0268205491806233,
-0.00981609004527654));
#37254=CARTESIAN_POINT('Ctrl Pts',(0.00181473752270681,-0.0268229517190221,
-0.00978648674939442));
#37255=CARTESIAN_POINT('Ctrl Pts',(0.00174808341450948,-0.0268271370605342,
-0.00973753848139958));
#37256=CARTESIAN_POINT('Ctrl Pts',(0.00172011364542257,-0.0268288955279405,
-0.0097177272580704));
#37257=CARTESIAN_POINT('Ctrl Pts',(0.0016787209442918,-0.0268315105944537,
-0.00968946086469258));
#37258=CARTESIAN_POINT('Ctrl Pts',(0.00166555976050306,-0.0268323439151437,
-0.00968062545194766));
#37259=CARTESIAN_POINT('Ctrl Pts',(0.00164200961327199,-0.0268338394362079,
-0.00966508501680036));
#37260=CARTESIAN_POINT('Ctrl Pts',(0.00163164832784109,-0.0268344989835844,
-0.009658339314924));
#37261=CARTESIAN_POINT('Ctrl Pts',(0.00160837986177967,-0.0268359836978885,
-0.00964339439712793));
#37262=CARTESIAN_POINT('Ctrl Pts',(0.00159545154923154,-0.0268368109485204,
-0.00963522971340862));
#37263=CARTESIAN_POINT('Ctrl Pts',(0.00155617820362321,-0.0268393295759174,
-0.0096108451899833));
#37264=CARTESIAN_POINT('Ctrl Pts',(0.00152964485720779,-0.0268410387475932,
-0.00959493414768093));
#37265=CARTESIAN_POINT('Ctrl Pts',(0.00137893508806576,-0.0268507686562533,
-0.00950769953436586));
#37266=CARTESIAN_POINT('Ctrl Pts',(0.00125003018846361,-0.0268591644455779,
-0.00944493310314055));
#37267=CARTESIAN_POINT('Ctrl Pts',(0.000926365096198284,-0.0268796819872125,
-0.00931506570535079));
#37268=CARTESIAN_POINT('Ctrl Pts',(0.000728194922046586,-0.026891747296662,
-0.00925831835760775));
#37269=CARTESIAN_POINT('Ctrl Pts',(0.000470225348096314,-0.0269063413553884,
-0.00921239751836219));
#37270=CARTESIAN_POINT('Ctrl Pts',(0.000414419374138996,-0.026909438044452,
-0.00920407955211752));
#37271=CARTESIAN_POINT('Ctrl Pts',(0.000331026879324982,-0.0269139772527621,
-0.00919404479803303));
#37272=CARTESIAN_POINT('Ctrl Pts',(0.000303599676465059,-0.0269154561092014,
-0.00919112750983954));
#37273=CARTESIAN_POINT('Ctrl Pts',(0.000254114374587732,-0.026918099834978,
-0.00918655320820368));
#37274=CARTESIAN_POINT('Ctrl Pts',(0.000232071030441415,-0.0269192687671969,
-0.0091847611539763));
#37275=CARTESIAN_POINT('Ctrl Pts',(0.000184629413821385,-0.0269217665198699,
-0.00918143192349406));
#37276=CARTESIAN_POINT('Ctrl Pts',(0.000159227232531907,-0.0269230928346091,
-0.00917997377293681));
#37277=CARTESIAN_POINT('Ctrl Pts',(8.96775204830524E-5,-0.0269266957094395,
-0.00917686855554262));
#37278=CARTESIAN_POINT('Ctrl Pts',(4.55065501382071E-5,-0.0269289524357815,
-0.00917587314000559));
#37279=CARTESIAN_POINT('Ctrl Pts',(-0.000145392922756357,-0.026938589684486,
-0.00917578862158119));
#37280=CARTESIAN_POINT('Ctrl Pts',(-0.000291929094222405,-0.0269456791476955,
-0.00918648718843781));
#37281=CARTESIAN_POINT('Ctrl Pts',(-0.000536536556900168,-0.0269574606377949,
-0.00922251107710548));
#37282=CARTESIAN_POINT('Ctrl Pts',(-0.000635171503360813,-0.026962200415781,
-0.00924214256734746));
#37283=CARTESIAN_POINT('Ctrl Pts',(-0.000856516629671363,-0.0269731046238776,
-0.00929788535138056));
#37284=CARTESIAN_POINT('Ctrl Pts',(-0.000978268969247597,-0.0269792953198636,
-0.00933696195306479));
#37285=CARTESIAN_POINT('Ctrl Pts',(-0.00111974546700643,-0.0269870983043951,
-0.00939255316161758));
#37286=CARTESIAN_POINT('Ctrl Pts',(-0.00114223378297961,-0.0269883576823508,
-0.00940170631664954));
#37287=CARTESIAN_POINT('Ctrl Pts',(-0.00117751931476832,-0.0269903675353013,
-0.0094165699465951));
#37288=CARTESIAN_POINT('Ctrl Pts',(-0.00119039227924913,-0.0269911079519724,
-0.00942209903226777));
#37289=CARTESIAN_POINT('Ctrl Pts',(-0.00121518988955551,-0.0269925490010256,
-0.00943295625757536));
#37290=CARTESIAN_POINT('Ctrl Pts',(-0.00122711936831542,-0.026993248932969,
-0.00943827248974219));
#37291=CARTESIAN_POINT('Ctrl Pts',(-0.0012563792802428,-0.0269949814778576,
-0.00945154150303195));
#37292=CARTESIAN_POINT('Ctrl Pts',(-0.0012736691823936,-0.026996018975379,
-0.00945958187756178));
#37293=CARTESIAN_POINT('Ctrl Pts',(-0.00133879210116586,-0.0269999756208012,
-0.00949062465757286));
#37294=CARTESIAN_POINT('Ctrl Pts',(-0.00138608632814361,-0.0270029495023824,
-0.00951472924700927));
#37295=CARTESIAN_POINT('Ctrl Pts',(-0.00151279953447129,-0.027011145723247,
-0.00958360593190222));
#37296=CARTESIAN_POINT('Ctrl Pts',(-0.00159085659497257,-0.0270164450639113,
-0.0096307633751304));
#37297=CARTESIAN_POINT('Ctrl Pts',(-0.00186485706128705,-0.0270357003400356,
-0.00981383372900022));
#37298=CARTESIAN_POINT('Ctrl Pts',(-0.00204661353808642,-0.0270496586464745,
-0.00996944576964931));
#37299=CARTESIAN_POINT('Ctrl Pts',(-0.00223580051543524,-0.0270650000859256,
-0.0101751340092416));
#37300=CARTESIAN_POINT('Ctrl Pts',(-0.00226293997817949,-0.0270672268682731,
-0.0102058826149279));
#37301=CARTESIAN_POINT('Ctrl Pts',(-0.00230541556461921,-0.0270707556431898,
-0.0102560433711941));
#37302=CARTESIAN_POINT('Ctrl Pts',(-0.00232115623375781,-0.0270720735012948,
-0.0102751047961467));
#37303=CARTESIAN_POINT('Ctrl Pts',(-0.00235081546114359,-0.0270745770331205,
-0.0103119390959857));
#37304=CARTESIAN_POINT('Ctrl Pts',(-0.00236477248109318,-0.0270757641570953,
-0.0103296787034528));
#37305=CARTESIAN_POINT('Ctrl Pts',(-0.00239663477829766,-0.0270784962434833,
-0.0103711304624337));
#37306=CARTESIAN_POINT('Ctrl Pts',(-0.00241439078548372,-0.0270800354614905,
-0.0103949546516549));
#37307=CARTESIAN_POINT('Ctrl Pts',(-0.00247141546155795,-0.0270850381686923,
-0.0104738884797533));
#37308=CARTESIAN_POINT('Ctrl Pts',(-0.00250917509071342,-0.0270884461688752,
-0.0105300647869997));
#37309=CARTESIAN_POINT('Ctrl Pts',(-0.00259316013190938,-0.0270963047104576,
-0.0106646309714038));
#37310=CARTESIAN_POINT('Ctrl Pts',(-0.00263778381183813,-0.0271007055093122,
-0.0107439418955299));
#37311=CARTESIAN_POINT('Ctrl Pts',(-0.00275800636705107,-0.0271134726400279,
-0.0109823711484938));
#37312=CARTESIAN_POINT('Ctrl Pts',(-0.00282327894873937,-0.0271216561485499,
-0.0111462466035163));
#37313=CARTESIAN_POINT('Ctrl Pts',(-0.00289698863239526,-0.0271341494586836,
-0.0113922821795902));
#37314=CARTESIAN_POINT('Ctrl Pts',(-0.00291703674722833,-0.0271381577390677,
-0.0114705720971312));
#37315=CARTESIAN_POINT('Ctrl Pts',(-0.00293853432553869,-0.027143460465929,
-0.0115712800107197));
#37316=CARTESIAN_POINT('Ctrl Pts',(-0.00294292751286983,-0.027144614910176,
-0.0115930407725214));
#37317=CARTESIAN_POINT('Ctrl Pts',(-0.00294959897100789,-0.0271464908778866,
-0.0116280873230505));
#37318=CARTESIAN_POINT('Ctrl Pts',(-0.00295202997664888,-0.0271472042766585,
-0.0116413435639292));
#37319=CARTESIAN_POINT('Ctrl Pts',(-0.00295651709088547,-0.0271485810463615,
-0.0116667764898916));
#37320=CARTESIAN_POINT('Ctrl Pts',(-0.00295858742861884,-0.0271492436209307,
-0.0116789499618797));
#37321=CARTESIAN_POINT('Ctrl Pts',(-0.00296257988336301,-0.0271505782496488,
-0.0117033353077343));
#37322=CARTESIAN_POINT('Ctrl Pts',(-0.00296450169884491,-0.0271512501859289,
-0.0117155463540992));
#37323=CARTESIAN_POINT('Ctrl Pts',(-0.00296898163759094,-0.0271528903073936,
-0.011745203828794));
#37324=CARTESIAN_POINT('Ctrl Pts',(-0.00297146148759825,-0.0271538625870964,
-0.0117626614210104));
#37325=CARTESIAN_POINT('Ctrl Pts',(-0.0029912177740022,-0.0271621833190282,
-0.0119111297951135));
#37326=CARTESIAN_POINT('Ctrl Pts',(-0.00299997282133411,-0.0271699176173088,
-0.0120431172027518));
#37327=CARTESIAN_POINT('Ctrl Pts',(-0.00299999993681902,-0.0271777321248805,
-0.0121752375870697));
#37328=CARTESIAN_POINT('',(-0.00212132034355963,-0.0271787743898723,-0.0100545329429984));
#37329=CARTESIAN_POINT('Origin',(0.,-0.0271787743898623,-0.0121758532865581));
#37330=CARTESIAN_POINT('',(0.00299984018495948,-0.026803478798527,-0.0121744321482416));
#37331=CARTESIAN_POINT('Ctrl Pts',(-0.00212132034355963,-0.0271787743898623,
-0.0100545329429984));
#37332=CARTESIAN_POINT('Ctrl Pts',(-0.0017049049496698,-0.0271475243898623,
-0.00963811754910862));
#37333=CARTESIAN_POINT('Ctrl Pts',(-0.000620685517841953,-0.0270850243898623,
-0.00905869905246725));
#37334=CARTESIAN_POINT('Ctrl Pts',(0.00121551243098668,-0.0269912743898623,
-0.00923888272063218));
#37335=CARTESIAN_POINT('Ctrl Pts',(0.00264200403629968,-0.0268975243898623,
-0.0104090155171674));
#37336=CARTESIAN_POINT('Ctrl Pts',(0.00299965007763634,-0.0268350243898623,
-0.0115851731935525));
#37337=CARTESIAN_POINT('Ctrl Pts',(0.00299999947199319,-0.0268037743898623,
-0.0121740733875246));
#37338=CARTESIAN_POINT('',(0.00299996104327479,-0.0258037247414263,-0.012178123434659));
#37339=CARTESIAN_POINT('Ctrl Pts',(0.00299924423124766,-0.026802372878294,
-0.0121757744092904));
#37340=CARTESIAN_POINT('Ctrl Pts',(0.00299673535939128,-0.0267690941025886,
-0.0127901983170197));
#37341=CARTESIAN_POINT('Ctrl Pts',(0.00280417962540106,-0.0267405918373098,
-0.0134078575495431));
#37342=CARTESIAN_POINT('Ctrl Pts',(0.00245082462041977,-0.0267078460568593,
-0.0139079213177871));
#37343=CARTESIAN_POINT('Ctrl Pts',(0.00235267788581048,-0.0266987506955989,
-0.0140468174003604));
#37344=CARTESIAN_POINT('Ctrl Pts',(0.00224210112526474,-0.0266893279522048,
-0.0141768653338118));
#37345=CARTESIAN_POINT('Ctrl Pts',(0.00212149108837053,-0.026679384540145,
-0.0142973544746626));
#37346=CARTESIAN_POINT('Ctrl Pts',(0.00184406930202044,-0.0266565131506066,
-0.0145744981813672));
#37347=CARTESIAN_POINT('Ctrl Pts',(0.00151025687286574,-0.0266347599993199,
-0.0147954171162992));
#37348=CARTESIAN_POINT('Ctrl Pts',(0.00114761927794851,-0.0266145858206189,
-0.0149461376973214));
#37349=CARTESIAN_POINT('Ctrl Pts',(0.000784981683031277,-0.0265944116419178,
-0.0150968582783436));
#37350=CARTESIAN_POINT('Ctrl Pts',(0.000392670575038502,-0.0265762819668012,
-0.0151766221497208));
#37351=CARTESIAN_POINT('Ctrl Pts',(-8.02388683067743E-8,-0.026555854964913,
-0.015176884072056));
#37352=CARTESIAN_POINT('Ctrl Pts',(-3.48441082191312E-5,-0.0265540468932306,
-0.0151769072557988));
#37353=CARTESIAN_POINT('Ctrl Pts',(-6.95979448631588E-5,-0.0265522128925814,
-0.0151763233275736));
#37354=CARTESIAN_POINT('Ctrl Pts',(-0.000104324389202502,-0.0265503565989124,
-0.0151751169414781));
#37355=CARTESIAN_POINT('Ctrl Pts',(-0.000461925943243557,-0.0265312410944776,
-0.0151626939724487));
#37356=CARTESIAN_POINT('Ctrl Pts',(-0.000817299624760045,-0.0265097615922842,
-0.0150840165707924));
#37357=CARTESIAN_POINT('Ctrl Pts',(-0.0011475009811764,-0.0264898884970649,
-0.0149464508263995));
#37358=CARTESIAN_POINT('Ctrl Pts',(-0.00150976796732726,-0.0264680855390495,
-0.0147955261658843));
#37359=CARTESIAN_POINT('Ctrl Pts',(-0.0018427597207118,-0.0264480613803005,
-0.014573950245931));
#37360=CARTESIAN_POINT('Ctrl Pts',(-0.0021212251561902,-0.0264288151819772,
-0.0142971007571688));
#37361=CARTESIAN_POINT('Ctrl Pts',(-0.0022604578739294,-0.0264191920828156,
-0.0141586760127877));
#37362=CARTESIAN_POINT('Ctrl Pts',(-0.0023860677632882,-0.0264096886133638,
-0.0140064727610748));
#37363=CARTESIAN_POINT('Ctrl Pts',(-0.00249534694135949,-0.0263995873087897,
-0.0138430823230018));
#37364=CARTESIAN_POINT('Ctrl Pts',(-0.00251954374151962,-0.026397350659023,
-0.0138069041063652));
#37365=CARTESIAN_POINT('Ctrl Pts',(-0.00254295703839925,-0.0263950717229805,
-0.0137701933918611));
#37366=CARTESIAN_POINT('Ctrl Pts',(-0.00256553425346917,-0.0263927564010959,
-0.013732978367566));
#37367=CARTESIAN_POINT('Ctrl Pts',(-0.00264492173991561,-0.0263846151142205,
-0.0136021204549458));
#37368=CARTESIAN_POINT('Ctrl Pts',(-0.00271394351715795,-0.0263760239482695,
-0.0134649978038269));
#37369=CARTESIAN_POINT('Ctrl Pts',(-0.00277208227918624,-0.0263672394278163,
-0.0133240399300175));
#37370=CARTESIAN_POINT('Ctrl Pts',(-0.00284675527592791,-0.0263559566545977,
-0.0131429946775136));
#37371=CARTESIAN_POINT('Ctrl Pts',(-0.00290345548498638,-0.0263445811317006,
-0.0129555559153653));
#37372=CARTESIAN_POINT('Ctrl Pts',(-0.00294150162794113,-0.0263336547667514,
-0.0127610417049336));
#37373=CARTESIAN_POINT('Ctrl Pts',(-0.0029605246994185,-0.0263281915842769,
-0.0126637845997177));
#37374=CARTESIAN_POINT('Ctrl Pts',(-0.00297482421323234,-0.0263227359100158,
-0.01256474343909));
#37375=CARTESIAN_POINT('Ctrl Pts',(-0.00298437329047243,-0.0263174422123873,
-0.0124699000564556));
#37376=CARTESIAN_POINT('Ctrl Pts',(-0.00298914782909248,-0.0263147953635731,
-0.0124224783651384));
#37377=CARTESIAN_POINT('Ctrl Pts',(-0.00299277570460114,-0.0263122594784373,
-0.0123761082719682));
#37378=CARTESIAN_POINT('Ctrl Pts',(-0.00299518340335414,-0.0263095726021238,
-0.0123231071556954));
#37379=CARTESIAN_POINT('Ctrl Pts',(-0.00299759110210715,-0.0263068857258102,
-0.0122701060394227));
#37380=CARTESIAN_POINT('Ctrl Pts',(-0.00299862475717886,-0.0263037826870209,
-0.012210477937357));
#37381=CARTESIAN_POINT('Ctrl Pts',(-0.00299887342984987,-0.0263018678103632,
-0.0121759532348433));
#37382=CARTESIAN_POINT('Ctrl Pts',(-0.00299912210252088,-0.0262999529337055,
-0.0121414285323296));
#37383=CARTESIAN_POINT('Ctrl Pts',(-0.00299875934617465,-0.0262995268874553,
-0.0121319906728096));
#37384=CARTESIAN_POINT('Ctrl Pts',(-0.00299832085105743,-0.0262987456299934,
-0.0121154106268001));
#37385=CARTESIAN_POINT('Ctrl Pts',(-0.00299788235594021,-0.0262979643725315,
-0.0120988305807907));
#37386=CARTESIAN_POINT('Ctrl Pts',(-0.00299730472817847,-0.0262967177950422,
-0.0120751157477882));
#37387=CARTESIAN_POINT('Ctrl Pts',(-0.00299645196421981,-0.0262955090939945,
-0.0120521389971071));
#37388=CARTESIAN_POINT('Ctrl Pts',(-0.00299474643630249,-0.0262930916918991,
-0.0120061854957447));
#37389=CARTESIAN_POINT('Ctrl Pts',(-0.00299201076742324,-0.0262909485423947,
-0.0119631737263696));
#37390=CARTESIAN_POINT('Ctrl Pts',(-0.00298806880567537,-0.0262887002297303,
-0.0119175451745365));
#37391=CARTESIAN_POINT('Ctrl Pts',(-0.00298018488217962,-0.0262842036044017,
-0.0118262880708702));
#37392=CARTESIAN_POINT('Ctrl Pts',(-0.00296737558619485,-0.0262791096282125,
-0.0117245846107055));
#37393=CARTESIAN_POINT('Ctrl Pts',(-0.00294746145973241,-0.0262737381999898,
-0.0116175990496526));
#37394=CARTESIAN_POINT('Ctrl Pts',(-0.00292754733326997,-0.0262683667717672,
-0.0115106134885997));
#37395=CARTESIAN_POINT('Ctrl Pts',(-0.00290056950786379,-0.0262627942966804,
-0.011398328512074));
#37396=CARTESIAN_POINT('Ctrl Pts',(-0.00286415384468825,-0.026256749612011,
-0.0112810074516751));
#37397=CARTESIAN_POINT('Ctrl Pts',(-0.00282773818151271,-0.0262507049273417,
-0.0111636863912763));
#37398=CARTESIAN_POINT('Ctrl Pts',(-0.00278187190752082,-0.0262441700152929,
-0.0110413300661203));
#37399=CARTESIAN_POINT('Ctrl Pts',(-0.00272405415663296,-0.0262368816762903,
-0.0109162086707602));
#37400=CARTESIAN_POINT('Ctrl Pts',(-0.00271912016742034,-0.0262362597118336,
-0.0109055311953224));
#37401=CARTESIAN_POINT('Ctrl Pts',(-0.00271410137325846,-0.0262356316298146,
-0.0108948360803448));
#37402=CARTESIAN_POINT('Ctrl Pts',(-0.00270899558262347,-0.0262349976164481,
-0.0108841250848099));
#37403=CARTESIAN_POINT('Ctrl Pts',(-0.00259443944523286,-0.0262207725673808,
-0.0106438076954377));
#37404=CARTESIAN_POINT('Ctrl Pts',(-0.00243528440089842,-0.0262035616951805,
-0.0103944168682738));
#37405=CARTESIAN_POINT('Ctrl Pts',(-0.00221968972734411,-0.0261854682004667,
-0.0101584152731379));
#37406=CARTESIAN_POINT('Ctrl Pts',(-0.00199448595479028,-0.0261665682749675,
-0.0099118950383051));
#37407=CARTESIAN_POINT('Ctrl Pts',(-0.00170740007538045,-0.0261471017547109,
-0.00968017773133318));
#37408=CARTESIAN_POINT('Ctrl Pts',(-0.0013576034578573,-0.0261275404938998,
-0.00950160676104891));
#37409=CARTESIAN_POINT('Ctrl Pts',(-0.00107674666081965,-0.0261118344727944,
-0.00935822952912178));
#37410=CARTESIAN_POINT('Ctrl Pts',(-0.000754970149059731,-0.0260959488223864,
-0.00924931751844913));
#37411=CARTESIAN_POINT('Ctrl Pts',(-0.000405204452938812,-0.0260772559187937,
-0.00920190336704683));
#37412=CARTESIAN_POINT('Ctrl Pts',(-0.000319350079617993,-0.0260726675113504,
-0.00919026496939855));
#37413=CARTESIAN_POINT('Ctrl Pts',(-0.000231832572911134,-0.0260679099616966,
-0.00918236687812477));
#37414=CARTESIAN_POINT('Ctrl Pts',(-0.000142935487738069,-0.0260629444083976,
-0.00917833097991991));
#37415=CARTESIAN_POINT('Ctrl Pts',(0.00030812312370331,-0.0260377494813456,
-0.00915785306844895));
#37416=CARTESIAN_POINT('Ctrl Pts',(0.000795119160569355,-0.026009515306029,
-0.0092408291296658));
#37417=CARTESIAN_POINT('Ctrl Pts',(0.00125831408289657,-0.0259833001929126,
-0.00945421707838627));
#37418=CARTESIAN_POINT('Ctrl Pts',(0.00162458284350649,-0.025962570740737,
-0.0096229523898924));
#37419=CARTESIAN_POINT('Ctrl Pts',(0.00197702463256216,-0.0259426559133689,
-0.00987425298737038));
#37420=CARTESIAN_POINT('Ctrl Pts',(0.00226508694472562,-0.0259194666608343,
-0.0102061852982747));
#37421=CARTESIAN_POINT('Ctrl Pts',(0.00234131723585644,-0.025913330059838,
-0.0102940249622207));
#37422=CARTESIAN_POINT('Ctrl Pts',(0.00241298674888928,-0.0259069641518263,
-0.0103875021935442));
#37423=CARTESIAN_POINT('Ctrl Pts',(0.00247967811919254,-0.0259002931583302,
-0.0104860271747369));
#37424=CARTESIAN_POINT('Ctrl Pts',(0.00276181762680004,-0.0258720713537445,
-0.0109028395682197));
#37425=CARTESIAN_POINT('Ctrl Pts',(0.00294915013904871,-0.0258425202835248,
-0.0114130346997862));
#37426=CARTESIAN_POINT('Ctrl Pts',(0.00299099925998867,-0.0258142681436675,
-0.0119611698913867));
#37427=CARTESIAN_POINT('Ctrl Pts',(0.00299642302465877,-0.0258106065862782,
-0.0120322097655791));
#37428=CARTESIAN_POINT('Ctrl Pts',(0.00299936426805713,-0.0258069668468853,
-0.012103825224218));
#37429=CARTESIAN_POINT('Ctrl Pts',(0.0029996789003323,-0.0258033546468746,
-0.0121758340213435));
#37430=CARTESIAN_POINT('',(0.00299998751882004,-0.0248036932032793,-0.0121758293984721));
#37431=CARTESIAN_POINT('Ctrl Pts',(0.00299999889294253,-0.0258037743898623,
-0.0121784305610133));
#37432=CARTESIAN_POINT('Ctrl Pts',(0.00299952054911593,-0.0257742293029132,
-0.0127352323200688));
#37433=CARTESIAN_POINT('Ctrl Pts',(0.00283972856505783,-0.0257446842159642,
-0.0132920158471201));
#37434=CARTESIAN_POINT('Ctrl Pts',(0.00254499247653757,-0.0257151391290152,
-0.0137642528881594));
#37435=CARTESIAN_POINT('Ctrl Pts',(0.00242406993537792,-0.0257030175492976,
-0.013957999447391));
#37436=CARTESIAN_POINT('Ctrl Pts',(0.00228103500614737,-0.0256908959695799,
-0.014137684814758));
#37437=CARTESIAN_POINT('Ctrl Pts',(0.00211982590390775,-0.0256787743898623,
-0.0142986670176993));
#37438=CARTESIAN_POINT('Ctrl Pts',(0.00173413343228542,-0.0256497735333579,
-0.0146838166331805));
#37439=CARTESIAN_POINT('Ctrl Pts',(0.00123888032829478,-0.0256207726768534,
-0.0149623095815553));
#37440=CARTESIAN_POINT('Ctrl Pts',(0.000707343059994884,-0.025591771820349,
-0.0150912719178145));
#37441=CARTESIAN_POINT('Ctrl Pts',(0.0004751999116223,-0.0255791060101868,
-0.0151475948222394));
#37442=CARTESIAN_POINT('Ctrl Pts',(0.000236507129008994,-0.0255664402000245,
-0.0151759836724882));
#37443=CARTESIAN_POINT('Ctrl Pts',(-1.64815128970163E-6,-0.0255537743898623,
-0.0151758528338243));
#37444=CARTESIAN_POINT('Ctrl Pts',(-0.00054896799349106,-0.0255246662835434,
-0.0151755521451443));
#37445=CARTESIAN_POINT('Ctrl Pts',(-0.00109801327074517,-0.0254955581772245,
-0.0150211395577944));
#37446=CARTESIAN_POINT('Ctrl Pts',(-0.00156617253887826,-0.0254664500709055,
-0.0147345841396303));
#37447=CARTESIAN_POINT('Ctrl Pts',(-0.00176815773010942,-0.0254538915105578,
-0.0146109511051568));
#37448=CARTESIAN_POINT('Ctrl Pts',(-0.00195524218533828,-0.02544133295021,
-0.014463383215985));
#37449=CARTESIAN_POINT('Ctrl Pts',(-0.00212215710272589,-0.0254287743898623,
-0.0142963365407599));
#37450=CARTESIAN_POINT('Ctrl Pts',(-0.00250895807067001,-0.0253996717585666,
-0.0139092302432509));
#37451=CARTESIAN_POINT('Ctrl Pts',(-0.00278805096283689,-0.0253705691272708,
-0.0134119508496134));
#37452=CARTESIAN_POINT('Ctrl Pts',(-0.00291657166754198,-0.0253414664959751,
-0.0128784269183515));
#37453=CARTESIAN_POINT('Ctrl Pts',(-0.00297205595222404,-0.0253289024606041,
-0.0126480967645078));
#37454=CARTESIAN_POINT('Ctrl Pts',(-0.0030000565339502,-0.0253163384252332,
-0.0124113703361084));
#37455=CARTESIAN_POINT('Ctrl Pts',(-0.00299999991383313,-0.0253037743898623,
-0.012175134258592));
#37456=CARTESIAN_POINT('Ctrl Pts',(-0.00299986876214958,-0.0252746717585666,
-0.0116279301748924));
#37457=CARTESIAN_POINT('Ctrl Pts',(-0.00284568929645957,-0.0252455691272708,
-0.0110789342839306));
#37458=CARTESIAN_POINT('Ctrl Pts',(-0.00255937922046653,-0.0252164664959751,
-0.0106107405092017));
#37459=CARTESIAN_POINT('Ctrl Pts',(-0.00243577493584797,-0.0252039024606041,
-0.0104086143479498));
#37460=CARTESIAN_POINT('Ctrl Pts',(-0.00228820817650185,-0.0251913384252332,
-0.0102213924515308));
#37461=CARTESIAN_POINT('Ctrl Pts',(-0.0021211404011013,-0.0251787743898623,
-0.0100543530158026));
#37462=CARTESIAN_POINT('Ctrl Pts',(-0.00173408111439472,-0.0251496662835434,
-0.00966735938588312));
#37463=CARTESIAN_POINT('Ctrl Pts',(-0.00123678155629453,-0.0251205581772245,
-0.00938808525837841));
#37464=CARTESIAN_POINT('Ctrl Pts',(-0.000703183699308903,-0.0250914500709055,
-0.00925942864583339));
#37465=CARTESIAN_POINT('Ctrl Pts',(-0.000472965325947317,-0.0250788915105578,
-0.00920392033433145));
#37466=CARTESIAN_POINT('Ctrl Pts',(-0.000236348792081367,-0.02506633295021,
-0.00917586983113488));
#37467=CARTESIAN_POINT('Ctrl Pts',(-2.10095426478409E-7,-0.0250537743898623,
-0.00917585329391478));
#37468=CARTESIAN_POINT('Ctrl Pts',(0.000545093209029396,-0.0250247735333579,
-0.00917581510533792));
#37469=CARTESIAN_POINT('Ctrl Pts',(0.00109237998997015,-0.0249957726768534,
-0.00932879021741214));
#37470=CARTESIAN_POINT('Ctrl Pts',(0.0015595447804611,-0.024966771820349,
-0.00961307743257935));
#37471=CARTESIAN_POINT('Ctrl Pts',(0.00176357394594232,-0.0249541060101868,
-0.00973723679657291));
#37472=CARTESIAN_POINT('Ctrl Pts',(0.00195247687430197,-0.0249414402000245,
-0.00988576529037574));
#37473=CARTESIAN_POINT('Ctrl Pts',(0.00212084323529318,-0.0249287743898623,
-0.0100540559420148));
#37474=CARTESIAN_POINT('Ctrl Pts',(0.00251358548478697,-0.0248992293029133,
-0.0104466215869831));
#37475=CARTESIAN_POINT('Ctrl Pts',(0.00279523648864188,-0.0248696842159643,
-0.0109522392104689));
#37476=CARTESIAN_POINT('Ctrl Pts',(0.0029217167302512,-0.0248401391290152,
-0.0114949925458995));
#37477=CARTESIAN_POINT('Ctrl Pts',(0.00297360827939497,-0.0248280175492976,
-0.0117176701042286));
#37478=CARTESIAN_POINT('Ctrl Pts',(0.00299991303547187,-0.0248158959695799,
-0.0119462727392586));
#37479=CARTESIAN_POINT('Ctrl Pts',(0.00299999978369675,-0.0248037743898623,
-0.0121747140677592));
#37480=CARTESIAN_POINT('',(0.00299999984621867,-0.0238037386203311,-0.0121751721745847));
#37481=CARTESIAN_POINT('Ctrl Pts',(0.00299999999993919,-0.0248037126098014,
-0.0121758723881634));
#37482=CARTESIAN_POINT('Ctrl Pts',(0.00299999645468512,-0.0247741731508083,
-0.0127326717795756));
#37483=CARTESIAN_POINT('Ctrl Pts',(0.00284068071006489,-0.0247446336918151,
-0.0132895892039848));
#37484=CARTESIAN_POINT('Ctrl Pts',(0.00254634976491414,-0.0247150942328219,
-0.013762076119177));
#37485=CARTESIAN_POINT('Ctrl Pts',(0.00242554000872495,-0.0247029695993176,
-0.0139560109736917));
#37486=CARTESIAN_POINT('Ctrl Pts',(0.00228258638271583,-0.0246908449658133,
-0.0141358911367041));
#37487=CARTESIAN_POINT('Ctrl Pts',(0.00212142859262928,-0.024678720332309,
-0.014297065375524));
#37488=CARTESIAN_POINT('Ctrl Pts',(0.00173603113214065,-0.0246497251285438,
-0.0146825021719953));
#37489=CARTESIAN_POINT('Ctrl Pts',(0.00124099384319939,-0.0246207299247786,
-0.0149613680577734));
#37490=CARTESIAN_POINT('Ctrl Pts',(0.000709559108885839,-0.0245917347210134,
-0.0150907333648799));
#37491=CARTESIAN_POINT('Ctrl Pts',(0.000477359067389681,-0.0245790658322812,
-0.015147257012543));
#37492=CARTESIAN_POINT('Ctrl Pts',(0.000238582482541089,-0.0245663969435489,
-0.0151758274351697));
#37493=CARTESIAN_POINT('Ctrl Pts',(3.25284021884075E-7,-0.0245537280548167,
-0.0151758532689232));
#37494=CARTESIAN_POINT('Ctrl Pts',(-0.00054698931659537,-0.0245246256066227,
-0.015175912613155));
#37495=CARTESIAN_POINT('Ctrl Pts',(-0.00109613181250209,-0.0244955231584287,
-0.0150218640939648));
#37496=CARTESIAN_POINT('Ctrl Pts',(-0.0015644771952416,-0.0244664207102346,
-0.0147356210700824));
#37497=CARTESIAN_POINT('Ctrl Pts',(-0.00176663160060002,-0.0244538590659312,
-0.0146120684731881));
#37498=CARTESIAN_POINT('Ctrl Pts',(-0.0019538881738259,-0.0244412974216278,
-0.0144645503382962));
#37499=CARTESIAN_POINT('Ctrl Pts',(-0.00212096854515054,-0.0244287357773243,
-0.0142975253701945));
#37500=CARTESIAN_POINT('Ctrl Pts',(-0.00250798270998806,-0.0243996387969876,
-0.0139106395377989));
#37501=CARTESIAN_POINT('Ctrl Pts',(-0.00278735326712094,-0.0243705418166509,
-0.0134135214976788));
#37502=CARTESIAN_POINT('Ctrl Pts',(-0.00291617434900536,-0.0243414448363141,
-0.012880074250605));
#37503=CARTESIAN_POINT('Ctrl Pts',(-0.00297181273367537,-0.0243288777241534,
-0.0126496760681051));
#37504=CARTESIAN_POINT('Ctrl Pts',(-0.00299994716922196,-0.0243163106119926,
-0.0124128605335314));
#37505=CARTESIAN_POINT('Ctrl Pts',(-0.00299999992525709,-0.0243037434998319,
-0.0121765229562029));
#37506=CARTESIAN_POINT('Ctrl Pts',(-0.00300012207275585,-0.0242746465194952,
-0.0116293240649705));
#37507=CARTESIAN_POINT('Ctrl Pts',(-0.00284619954974807,-0.0242455495391585,
-0.0110802609922032));
#37508=CARTESIAN_POINT('Ctrl Pts',(-0.00256011048884314,-0.0242164525588217,
-0.0106119369573015));
#37509=CARTESIAN_POINT('Ctrl Pts',(-0.00243654738109967,-0.024203885446661,
-0.0104096657729355));
#37510=CARTESIAN_POINT('Ctrl Pts',(-0.00228899402826749,-0.0241913183345003,
-0.0102223005924817));
#37511=CARTESIAN_POINT('Ctrl Pts',(-0.00212191554668422,-0.0241787512223395,
-0.0100551283131729));
#37512=CARTESIAN_POINT('Ctrl Pts',(-0.0017350014496016,-0.0241496487741455,
-0.00966799700282649));
#37513=CARTESIAN_POINT('Ctrl Pts',(-0.00123780898872271,-0.0241205463259515,
-0.00938854213547383));
#37514=CARTESIAN_POINT('Ctrl Pts',(-0.000704262897402285,-0.0240914438777575,
-0.00925968906427182));
#37515=CARTESIAN_POINT('Ctrl Pts',(-0.000473965563859015,-0.024078882233454,
-0.00920407152869351));
#37516=CARTESIAN_POINT('Ctrl Pts',(-0.000237254351499635,-0.0240663205891505,
-0.00917593331151893));
#37517=CARTESIAN_POINT('Ctrl Pts',(-1.01405525885435E-6,-0.0240537589448471,
-0.00917585345794278));
#37518=CARTESIAN_POINT('Ctrl Pts',(0.000544283627240826,-0.0240247637410819,
-0.00917566913727139));
#37519=CARTESIAN_POINT('Ctrl Pts',(0.00109160692055374,-0.0239957685373167,
-0.00932849457792729));
#37520=CARTESIAN_POINT('Ctrl Pts',(0.00155884545293593,-0.0239667733335515,
-0.0096126519964014));
#37521=CARTESIAN_POINT('Ctrl Pts',(0.00176299621614839,-0.0239541044448192,
-0.0097368090378984));
#37522=CARTESIAN_POINT('Ctrl Pts',(0.00195201430165641,-0.023941435556087,
-0.00988536040928045));
#37523=CARTESIAN_POINT('Ctrl Pts',(0.00212048137367313,-0.0239287666673547,
-0.0100536943047885));
#37524=CARTESIAN_POINT('Ctrl Pts',(0.00251328821496056,-0.0238992272083615,
-0.0104461906246009));
#37525=CARTESIAN_POINT('Ctrl Pts',(0.00279502498094163,-0.0238696877493684,
-0.0109517571981392));
#37526=CARTESIAN_POINT('Ctrl Pts',(0.00292159872971184,-0.0238401482903752,
-0.0114944863791241));
#37527=CARTESIAN_POINT('Ctrl Pts',(0.00297355162145094,-0.0238280236568709,
-0.0117172525581882));
#37528=CARTESIAN_POINT('Ctrl Pts',(0.00299989620579271,-0.0238158990233666,
-0.0119459534947592));
#37529=CARTESIAN_POINT('Ctrl Pts',(0.00299999969243972,-0.0238037743898623,
-0.0121744948456985));
#37530=CARTESIAN_POINT('',(0.00299999948987923,-0.0228038528083122,-0.0121770162025489));
#37531=CARTESIAN_POINT('Ctrl Pts',(0.00299999999999761,-0.0238037028507998,
-0.012175849503471));
#37532=CARTESIAN_POINT('Ctrl Pts',(0.00300000070212657,-0.0237742589851738,
-0.0127326399815581));
#37533=CARTESIAN_POINT('Ctrl Pts',(0.00284069411920419,-0.0237447999402777,
-0.0132895506791278));
#37534=CARTESIAN_POINT('Ctrl Pts',(0.00254637537593904,-0.0237153253373963,
-0.0137620350052812));
#37535=CARTESIAN_POINT('Ctrl Pts',(0.00242551065442886,-0.0237032213183679,
-0.0139560650757582));
#37536=CARTESIAN_POINT('Ctrl Pts',(0.00228248050278621,-0.0236911146756247,
-0.0141360271007935));
#37537=CARTESIAN_POINT('Ctrl Pts',(0.00212123065892674,-0.0236790053829392,
-0.0142972633109591));
#37538=CARTESIAN_POINT('Ctrl Pts',(0.00173579890898887,-0.0236500608223828,
-0.0146826624725959));
#37539=CARTESIAN_POINT('Ctrl Pts',(0.001240737142082,-0.0236211011215851,
-0.014961482382444));
#37540=CARTESIAN_POINT('Ctrl Pts',(0.000709290622295351,-0.0235921273550881,
-0.0150907987085384));
#37541=CARTESIAN_POINT('Ctrl Pts',(0.000476979877153939,-0.0235794620782749,
-0.0151473266392999));
#37542=CARTESIAN_POINT('Ctrl Pts',(0.000238088999641541,-0.0235667941137618,
-0.015175875228355));
#37543=CARTESIAN_POINT('Ctrl Pts',(-2.7631354590831E-7,-0.0235541235513023,
-0.0151758532738332));
#37544=CARTESIAN_POINT('Ctrl Pts',(-0.000547620793514525,-0.0235250288716799,
-0.015175802860935));
#37545=CARTESIAN_POINT('Ctrl Pts',(-0.00109675970552012,-0.0234959204937934,
-0.0150216279019523));
#37546=CARTESIAN_POINT('Ctrl Pts',(-0.00156506467060867,-0.0234667944331137,
-0.0147352619246643));
#37547=CARTESIAN_POINT('Ctrl Pts',(-0.00176725716029671,-0.0234542191431581,
-0.0146116223004317));
#37548=CARTESIAN_POINT('Ctrl Pts',(-0.00195453684989838,-0.0234416405569279,
-0.0144640045171204));
#37549=CARTESIAN_POINT('Ctrl Pts',(-0.00212162140575758,-0.0234290583537329,
-0.0142968725251864));
#37550=CARTESIAN_POINT('Ctrl Pts',(-0.0025083439476894,-0.0233999364425086,
-0.013910040190944));
#37551=CARTESIAN_POINT('Ctrl Pts',(-0.0027874958188367,-0.0233707951549935,
-0.013413089999592));
#37552=CARTESIAN_POINT('Ctrl Pts',(-0.00291622221040971,-0.023341649313097,
-0.0128798760273223));
#37553=CARTESIAN_POINT('Ctrl Pts',(-0.00297192792673784,-0.0233290365925742,
-0.0126491302888728));
#37554=CARTESIAN_POINT('Ctrl Pts',(-0.00300004532424149,-0.0233164230191599,
-0.0124119543162287));
#37555=CARTESIAN_POINT('Ctrl Pts',(-0.00299999994485589,-0.0233038097940137,
-0.012175278078183));
#37556=CARTESIAN_POINT('Ctrl Pts',(-0.00299989497433512,-0.0232746331801249,
-0.0116278042057919));
#37557=CARTESIAN_POINT('Ctrl Pts',(-0.00284559490133652,-0.0232454584297435,
-0.011078576309219));
#37558=CARTESIAN_POINT('Ctrl Pts',(-0.00255907619185309,-0.0232162965318514,
-0.0106102450838807));
#37559=CARTESIAN_POINT('Ctrl Pts',(-0.00243550316989592,-0.0232037192594804,
-0.0104082579086059));
#37560=CARTESIAN_POINT('Ctrl Pts',(-0.00228799832177968,-0.0231911443778289,
-0.0102211626319481));
#37561=CARTESIAN_POINT('Ctrl Pts',(-0.00212101326950556,-0.0231785727684926,
-0.0100542259133888));
#37562=CARTESIAN_POINT('Ctrl Pts',(-0.00173396160267819,-0.0231494332600034,
-0.00966728627841473));
#37563=CARTESIAN_POINT('Ctrl Pts',(-0.00123668829684548,-0.0231203113322811,
-0.00938805142639478));
#37564=CARTESIAN_POINT('Ctrl Pts',(-0.000703125086075461,-0.0230912040398712,
-0.00925941451412838));
#37565=CARTESIAN_POINT('Ctrl Pts',(-0.000472761265818371,-0.0230786370807152,
-0.0092038760325809));
#37566=CARTESIAN_POINT('Ctrl Pts',(-0.000235991961798253,-0.0230660728496497,
-0.00917583020279523));
#37567=CARTESIAN_POINT('Ctrl Pts',(2.93265437673792E-7,-0.0230535111096261,
-0.0091758533008922));
#37568=CARTESIAN_POINT('Ctrl Pts',(0.000545584674455736,-0.0230245215320833,
-0.0091759066059337));
#37569=CARTESIAN_POINT('Ctrl Pts',(0.00109283646594747,-0.0229955452213105,
-0.00932896713018142));
#37570=CARTESIAN_POINT('Ctrl Pts',(0.00155994875593833,-0.0229665829718963,
-0.00961332331037315));
#37571=CARTESIAN_POINT('Ctrl Pts',(0.00176405944180797,-0.0229539275468114,
-0.00973757637802705));
#37572=CARTESIAN_POINT('Ctrl Pts',(0.00195302501859612,-0.0229412748065526,
-0.0098862205247778));
#37573=CARTESIAN_POINT('Ctrl Pts',(0.00212142802901245,-0.0229286248174143,
-0.010054640633918));
#37574=CARTESIAN_POINT('Ctrl Pts',(0.0025140637145109,-0.0228991310622576,
-0.0104473161855042));
#37575=CARTESIAN_POINT('Ctrl Pts',(0.00279557606596665,-0.0228696522622051,
-0.0109530140335188));
#37576=CARTESIAN_POINT('Ctrl Pts',(0.00292190596310267,-0.0228401881371818,
-0.0114958050950414));
#37577=CARTESIAN_POINT('Ctrl Pts',(0.00297375919097428,-0.0228280943254753,
-0.0117185985052942));
#37578=CARTESIAN_POINT('Ctrl Pts',(0.00300000056297038,-0.0228160029861661,
-0.0119473153256647));
#37579=CARTESIAN_POINT('Ctrl Pts',(0.0029999999999909,-0.0228039140998865,
-0.0121758606765069));
#37580=CARTESIAN_POINT('',(0.00299999978565727,-0.0218037310910125,-0.0121750620270919));
#37581=CARTESIAN_POINT('Ctrl Pts',(0.00299999883722565,-0.0228037743898623,
-0.0121784946204567));
#37582=CARTESIAN_POINT('Ctrl Pts',(0.00299950860341255,-0.0227742284435262,
-0.0127352969505315));
#37583=CARTESIAN_POINT('Ctrl Pts',(0.00283970441390225,-0.02274468249719,
-0.0132920775528615));
#37584=CARTESIAN_POINT('Ctrl Pts',(0.00254495771088097,-0.0227151365508539,
-0.0137643085896206));
#37585=CARTESIAN_POINT('Ctrl Pts',(0.00242404290534297,-0.0227030158305234,
-0.0139580333145911));
#37586=CARTESIAN_POINT('Ctrl Pts',(0.00228102041420593,-0.0226908951101928,
-0.0141376991714502));
#37587=CARTESIAN_POINT('Ctrl Pts',(0.00211982731969915,-0.0226787743898623,
-0.0142986656038997));
#37588=CARTESIAN_POINT('Ctrl Pts',(0.001734134198291,-0.0226497726607727,
-0.0146838163819981));
#37589=CARTESIAN_POINT('Ctrl Pts',(0.00123888007405062,-0.0226207709316831,
-0.0149623098929398));
#37590=CARTESIAN_POINT('Ctrl Pts',(0.000707341766562069,-0.0225917692025935,
-0.0150912722316287));
#37591=CARTESIAN_POINT('Ctrl Pts',(0.000475221141499959,-0.0225791042650164,
-0.0151475895623728));
#37592=CARTESIAN_POINT('Ctrl Pts',(0.000236552172571135,-0.0225664393274394,
-0.015175978293945));
#37593=CARTESIAN_POINT('Ctrl Pts',(-1.58009018492896E-6,-0.0225537743898623,
-0.0151758528704439));
#37594=CARTESIAN_POINT('Ctrl Pts',(-0.00054890114122793,-0.0225246654112391,
-0.015175564598197));
#37595=CARTESIAN_POINT('Ctrl Pts',(-0.00109795087836807,-0.0224955564326158,
-0.0150211638189013));
#37596=CARTESIAN_POINT('Ctrl Pts',(-0.00156611716280598,-0.0224664474539926,
-0.0147346180339244));
#37597=CARTESIAN_POINT('Ctrl Pts',(-0.00176808529877214,-0.0224538897659491,
-0.0146110014472874));
#37598=CARTESIAN_POINT('Ctrl Pts',(-0.00195515614604609,-0.0224413320779057,
-0.0144634543840437));
#37599=CARTESIAN_POINT('Ctrl Pts',(-0.00212206229987348,-0.0224287743898623,
-0.0142964314142053));
#37600=CARTESIAN_POINT('Ctrl Pts',(-0.00250888140021627,-0.0223996708878047,
-0.0139093415828963));
#37601=CARTESIAN_POINT('Ctrl Pts',(-0.00278799673686266,-0.0223705673857471,
-0.0134120735635768));
#37602=CARTESIAN_POINT('Ctrl Pts',(-0.0029165409691721,-0.0223414638836895,
-0.0128785543432961));
#37603=CARTESIAN_POINT('Ctrl Pts',(-0.00297202990472548,-0.0223289007190805,
-0.0126482490771728));
#37604=CARTESIAN_POINT('Ctrl Pts',(-0.0030000408079041,-0.0223163375544714,
-0.0124115475875402));
#37605=CARTESIAN_POINT('Ctrl Pts',(-0.00299999995513309,-0.0223037743898623,
-0.0121753344402846));
#37606=CARTESIAN_POINT('Ctrl Pts',(-0.00299990531666084,-0.0222746708878047,
-0.0116281291754413));
#37607=CARTESIAN_POINT('Ctrl Pts',(-0.00284576185212074,-0.0222455673857471,
-0.0110791220651115));
#37608=CARTESIAN_POINT('Ctrl Pts',(-0.00255948205582041,-0.0222164638836896,
-0.010610908685004));
#37609=CARTESIAN_POINT('Ctrl Pts',(-0.00243590310652211,-0.0222039007190805,
-0.0104087941162889));
#37610=CARTESIAN_POINT('Ctrl Pts',(-0.00228836540196688,-0.0221913375544714,
-0.0102215793127615));
#37611=CARTESIAN_POINT('Ctrl Pts',(-0.00212132867023112,-0.0221787743898623,
-0.0100545412697026));
#37612=CARTESIAN_POINT('Ctrl Pts',(-0.00173430288455623,-0.0221496654112391,
-0.00966751244567895));
#37613=CARTESIAN_POINT('Ctrl Pts',(-0.00123702698233215,-0.0221205564326158,
-0.00938819396503985));
#37614=CARTESIAN_POINT('Ctrl Pts',(-0.000703439480540827,-0.0220914474539925,
-0.00925949032951444));
#37615=CARTESIAN_POINT('Ctrl Pts',(-0.000473248463601254,-0.0220788897659491,
-0.00920396725102037));
#37616=CARTESIAN_POINT('Ctrl Pts',(-0.000236658131907783,-0.0220663320779057,
-0.00917589602513529));
#37617=CARTESIAN_POINT('Ctrl Pts',(-5.42397702818636E-7,-0.0220537743898623,
-0.00917585333559064));
#37618=CARTESIAN_POINT('Ctrl Pts',(0.000544762162621619,-0.0220247726607727,
-0.00917575474494208));
#37619=CARTESIAN_POINT('Ctrl Pts',(0.00109206689317226,-0.0219957709316831,
-0.0093286699125783));
#37620=CARTESIAN_POINT('Ctrl Pts',(0.00155926371864595,-0.0219667692025935,
-0.00961290641709037));
#37621=CARTESIAN_POINT('Ctrl Pts',(0.00176328667922693,-0.0219541042650164,
-0.00973703134687119));
#37622=CARTESIAN_POINT('Ctrl Pts',(0.00195218903299633,-0.0219414393274394,
-0.00988552230538304));
#37623=CARTESIAN_POINT('Ctrl Pts',(0.00212056146838152,-0.0219287743898623,
-0.0100537743392011));
#37624=CARTESIAN_POINT('Ctrl Pts',(0.0025133563724309,-0.0218992284435262,
-0.0104462883592574));
#37625=CARTESIAN_POINT('Ctrl Pts',(0.00279507461672607,-0.0218696824971901,
-0.010951869259183));
#37626=CARTESIAN_POINT('Ctrl Pts',(0.00292162671273439,-0.0218401365508539,
-0.0114946063772537));
#37627=CARTESIAN_POINT('Ctrl Pts',(0.00297354255071463,-0.0218280158305234,
-0.0117172550190096));
#37628=CARTESIAN_POINT('Ctrl Pts',(0.00299987747078827,-0.0218158951101928,
-0.0119458309340674));
#37629=CARTESIAN_POINT('Ctrl Pts',(0.0029999995713889,-0.0218037743898623,
-0.0121742496449468));
#37630=CARTESIAN_POINT('',(0.00299999993086331,-0.0208037504150882,-0.0121753965937047));
#37631=CARTESIAN_POINT('Ctrl Pts',(0.00299999999992564,-0.0218036877921627,
-0.012175874409237));
#37632=CARTESIAN_POINT('Ctrl Pts',(0.00299999607956417,-0.0217741497906089,
-0.01273267331044));
#37633=CARTESIAN_POINT('Ctrl Pts',(0.00284068022618476,-0.0217446117890551,
-0.013289590216266));
#37634=CARTESIAN_POINT('Ctrl Pts',(0.00254634941007706,-0.0217150737875013,
-0.0137620766887938));
#37635=CARTESIAN_POINT('Ctrl Pts',(0.00242552952729006,-0.0217029487306259,
-0.0139560277027724));
#37636=CARTESIAN_POINT('Ctrl Pts',(0.00228256206844824,-0.0216908236737505,
-0.0141359216549807));
#37637=CARTESIAN_POINT('Ctrl Pts',(0.00212138778135082,-0.0216786986168751,
-0.0142971061901826));
#37638=CARTESIAN_POINT('Ctrl Pts',(0.00173598366932797,-0.0216497048681671,
-0.0146825348077372));
#37639=CARTESIAN_POINT('Ctrl Pts',(0.0012409420320321,-0.0216207111194592,
-0.01496139097265));
#37640=CARTESIAN_POINT('Ctrl Pts',(0.000709505757877311,-0.0215917173707512,
-0.015090746351413));
#37641=CARTESIAN_POINT('Ctrl Pts',(0.000477285674087594,-0.02157904806103,
-0.015147270375752));
#37642=CARTESIAN_POINT('Ctrl Pts',(0.000238488477075509,-0.0215663787513088,
-0.0151758364513004));
#37643=CARTESIAN_POINT('Ctrl Pts',(2.11868588605447E-7,-0.0215537094415876,
-0.0151758532790767));
#37644=CARTESIAN_POINT('Ctrl Pts',(-0.000547101720137076,-0.0215246084508768,
-0.0151758919319293));
#37645=CARTESIAN_POINT('Ctrl Pts',(-0.00109623758463809,-0.0214955074601659,
-0.015021823198552));
#37646=CARTESIAN_POINT('Ctrl Pts',(-0.00156457171055949,-0.0214664064694551,
-0.0147355633018756));
#37647=CARTESIAN_POINT('Ctrl Pts',(-0.00176673819564929,-0.0214538444017367,
-0.0146119930687235));
#37648=CARTESIAN_POINT('Ctrl Pts',(-0.00195400349499016,-0.0214412823340184,
-0.0144644538808624));
#37649=CARTESIAN_POINT('Ctrl Pts',(-0.0021210881422845,-0.0214287202663,
-0.0142974058059787));
#37650=CARTESIAN_POINT('Ctrl Pts',(-0.00250807980025495,-0.0213996247420099,
-0.0139104988548804));
#37651=CARTESIAN_POINT('Ctrl Pts',(-0.00278742215409447,-0.0213705292177197,
-0.0134133659977121));
#37652=CARTESIAN_POINT('Ctrl Pts',(-0.00291621343819134,-0.0213414336934296,
-0.0128799123628523));
#37653=CARTESIAN_POINT('Ctrl Pts',(-0.00297184360465812,-0.0213288661592906,
-0.0126494921545466));
#37654=CARTESIAN_POINT('Ctrl Pts',(-0.00299996491844838,-0.0213162986251515,
-0.0124126550628953));
#37655=CARTESIAN_POINT('Ctrl Pts',(-0.00299999996701662,-0.0213037310910125,
-0.012176298146413));
#37656=CARTESIAN_POINT('Ctrl Pts',(-0.003000081109145,-0.0212746355667223,
-0.0116291002372155));
#37657=CARTESIAN_POINT('Ctrl Pts',(-0.00284611797447065,-0.0212455400424322,
-0.0110800494869966));
#37658=CARTESIAN_POINT('Ctrl Pts',(-0.00255999463096865,-0.0212164445181421,
-0.0106117473152724));
#37659=CARTESIAN_POINT('Ctrl Pts',(-0.00243640638242635,-0.021203876984003,
-0.010409468659908));
#37660=CARTESIAN_POINT('Ctrl Pts',(-0.00228882502846644,-0.021191309449864,
-0.0102221002517993));
#37661=CARTESIAN_POINT('Ctrl Pts',(-0.00212171724469397,-0.0211787419157249,
-0.0100549299184073));
#37662=CARTESIAN_POINT('Ctrl Pts',(-0.00173476766417422,-0.0211496409250141,
-0.0096678354999363));
#37663=CARTESIAN_POINT('Ctrl Pts',(-0.00123755002938891,-0.0211205399343033,
-0.00938842730832361));
#37664=CARTESIAN_POINT('Ctrl Pts',(-0.000703992790271626,-0.0210914389435924,
-0.00925962384578264));
#37665=CARTESIAN_POINT('Ctrl Pts',(-0.000473671347403565,-0.0210788768758741,
-0.00920402306452828));
#37666=CARTESIAN_POINT('Ctrl Pts',(-0.00023693751233426,-0.0210663148081557,
-0.00917590674609835));
#37667=CARTESIAN_POINT('Ctrl Pts',(-6.77851118439549E-7,-0.0210537527404374,
-0.00917585336313846));
#37668=CARTESIAN_POINT('Ctrl Pts',(0.000544618783218096,-0.0210247589917294,
-0.00917573015315749));
#37669=CARTESIAN_POINT('Ctrl Pts',(0.00109192409600206,-0.0209957652430214,
-0.00932861635859259));
#37670=CARTESIAN_POINT('Ctrl Pts',(0.00155913031831126,-0.0209667714943134,
-0.00961282526280911));
#37671=CARTESIAN_POINT('Ctrl Pts',(0.00176328399273679,-0.0209541021845922,
-0.0097370151586831));
#37672=CARTESIAN_POINT('Ctrl Pts',(0.00195229978348282,-0.020941432874871,
-0.00988560171783371));
#37673=CARTESIAN_POINT('Ctrl Pts',(0.00212075858122446,-0.0209287635651498,
-0.0100539713293883));
#37674=CARTESIAN_POINT('Ctrl Pts',(0.00251351369882283,-0.0208992255635961,
-0.0104465185128695));
#37675=CARTESIAN_POINT('Ctrl Pts',(0.0027951843313585,-0.0208696875620423,
-0.0109521213124772));
#37676=CARTESIAN_POINT('Ctrl Pts',(0.00292168736193154,-0.0208401495604885,
-0.0114948665325536));
#37677=CARTESIAN_POINT('Ctrl Pts',(0.00297361560216193,-0.0208280245036131,
-0.0117176580660399));
#37678=CARTESIAN_POINT('Ctrl Pts',(0.00299993046755241,-0.0208158994467377,
-0.0119463820244118));
#37679=CARTESIAN_POINT('Ctrl Pts',(0.00299999986172769,-0.0208037743898623,
-0.0121749424441802));
#37680=CARTESIAN_POINT('',(0.00299999945013065,-0.0198038454750366,-0.0121771205057471));
#37681=CARTESIAN_POINT('Ctrl Pts',(0.00299999999999892,-0.0208037264403141,
-0.0121758507432291));
#37682=CARTESIAN_POINT('Ctrl Pts',(0.00300000047203861,-0.0207741929253612,
-0.0127326481792972));
#37683=CARTESIAN_POINT('Ctrl Pts',(0.00284068981401535,-0.0207446594104083,
-0.013289565089164));
#37684=CARTESIAN_POINT('Ctrl Pts',(0.00254636407823635,-0.0207151258954554,
-0.013762053141894));
#37685=CARTESIAN_POINT('Ctrl Pts',(0.00242552667548471,-0.0207030007130224,
-0.0139560362775241));
#37686=CARTESIAN_POINT('Ctrl Pts',(0.00228253446287072,-0.0206908755305894,
-0.0141359580207443));
#37687=CARTESIAN_POINT('Ctrl Pts',(0.00212133014721027,-0.0206787503481565,
-0.0142971638264218));
#37688=CARTESIAN_POINT('Ctrl Pts',(0.00173591719310115,-0.0206497610350512,
-0.0146825803429162));
#37689=CARTESIAN_POINT('Ctrl Pts',(0.00124087014846921,-0.0206207717219459,
-0.0149614226384336));
#37690=CARTESIAN_POINT('Ctrl Pts',(0.000709432384186756,-0.0205917824088407,
-0.0150907642101143));
#37691=CARTESIAN_POINT('Ctrl Pts',(0.000477170333426602,-0.0205791127836004,
-0.0151472922566818));
#37692=CARTESIAN_POINT('Ctrl Pts',(0.000238329566291121,-0.0205664431583602,
-0.0151758523684426));
#37693=CARTESIAN_POINT('Ctrl Pts',(1.15571610319707E-8,-0.02055377353312,
-0.0151758532865358));
#37694=CARTESIAN_POINT('Ctrl Pts',(-0.000547299870503991,-0.0205246769881148,
-0.0151758553949913));
#37695=CARTESIAN_POINT('Ctrl Pts',(-0.00109642372481938,-0.0204955804431096,
-0.0150217511609241));
#37696=CARTESIAN_POINT('Ctrl Pts',(-0.00156473780817212,-0.0204664838981044,
-0.014735461770619));
#37697=CARTESIAN_POINT('Ctrl Pts',(-0.00176693177040435,-0.0204539215047641,
-0.0146118567195891));
#37698=CARTESIAN_POINT('Ctrl Pts',(-0.00195421772447099,-0.0204413591114238,
-0.014464275218782));
#37699=CARTESIAN_POINT('Ctrl Pts',(-0.00212131380292897,-0.0204287967180835,
-0.0142971801707283));
#37700=CARTESIAN_POINT('Ctrl Pts',(-0.00250826281589996,-0.0203997056361836,
-0.0139102335438927));
#37701=CARTESIAN_POINT('Ctrl Pts',(-0.00278755190394519,-0.0203706145542837,
-0.0134130729604044));
#37702=CARTESIAN_POINT('Ctrl Pts',(-0.00291628702624431,-0.0203415234723838,
-0.0128796074912057));
#37703=CARTESIAN_POINT('Ctrl Pts',(-0.00297190285181329,-0.0203289556159382,
-0.0126491410734002));
#37704=CARTESIAN_POINT('Ctrl Pts',(-0.00299999945292661,-0.0203163877594927,
-0.0124122583918547));
#37705=CARTESIAN_POINT('Ctrl Pts',(-0.00299999999999197,-0.0203038199030471,
-0.0121758602290658));
#37706=CARTESIAN_POINT('Ctrl Pts',(-0.00300000126629566,-0.0202747288211472,
-0.0116286644248754));
#37707=CARTESIAN_POINT('Ctrl Pts',(-0.00284595912377596,-0.0202456377392472,
-0.0110796378325426));
#37708=CARTESIAN_POINT('Ctrl Pts',(-0.00255976915460028,-0.0202165466573473,
-0.0106113783346471));
#37709=CARTESIAN_POINT('Ctrl Pts',(-0.00243613007987847,-0.0202039788009018,
-0.0104090820374839));
#37710=CARTESIAN_POINT('Ctrl Pts',(-0.00228849159223828,-0.0201914109444562,
-0.0102217047082522));
#37711=CARTESIAN_POINT('Ctrl Pts',(-0.00212132362112505,-0.0201788430880106,
-0.0100545362205689));
#37712=CARTESIAN_POINT('Ctrl Pts',(-0.00173430373304865,-0.0201497465430054,
-0.00966751513655252));
#37713=CARTESIAN_POINT('Ctrl Pts',(-0.00123703629027194,-0.0201206499980002,
-0.00938819961622383));
#37714=CARTESIAN_POINT('Ctrl Pts',(-0.000703457073080728,-0.020091553452995,
-0.00925949457296804));
#37715=CARTESIAN_POINT('Ctrl Pts',(-0.000473084978959003,-0.0200789910596548,
-0.00920392634732584));
#37716=CARTESIAN_POINT('Ctrl Pts',(-0.000236303284987885,-0.0200664286663145,
-0.00917585346991708));
#37717=CARTESIAN_POINT('Ctrl Pts',(-2.32785436811739E-9,-0.0200538662729742,
-0.009175853286559));
#37718=CARTESIAN_POINT('Ctrl Pts',(0.00054529204781636,-0.0200248769598689,
-0.00917585286343704));
#37719=CARTESIAN_POINT('Ctrl Pts',(0.00109256110731081,-0.0199958876467636,
-0.00932886108422719));
#37720=CARTESIAN_POINT('Ctrl Pts',(0.00155970233578898,-0.0199668983336584,
-0.00961317331751507));
#37721=CARTESIAN_POINT('Ctrl Pts',(0.0017638639272547,-0.0199542287084181,
-0.00973743046820657));
#37722=CARTESIAN_POINT('Ctrl Pts',(0.00195287686596327,-0.0199415590831779,
-0.00988608946770726));
#37723=CARTESIAN_POINT('Ctrl Pts',(0.00212132032904437,-0.0199288894579377,
-0.0100545329284832));
#37724=CARTESIAN_POINT('Ctrl Pts',(0.00251397054265975,-0.0198993559220794,
-0.0104471831367251));
#37725=CARTESIAN_POINT('Ctrl Pts',(0.00279550710894889,-0.0198698223862211,
-0.0109528592737185));
#37726=CARTESIAN_POINT('Ctrl Pts',(0.00292186681724648,-0.0198402888503629,
-0.011495636922249));
#37727=CARTESIAN_POINT('Ctrl Pts',(0.00297374554685843,-0.0198281634478756,
-0.011718481808858));
#37728=CARTESIAN_POINT('Ctrl Pts',(0.00300000017425403,-0.0198160380453884,
-0.011947254496424));
#37729=CARTESIAN_POINT('Ctrl Pts',(0.00299999999999913,-0.0198039126429012,
-0.0121758555733571));
#37730=CARTESIAN_POINT('',(0.0029999996678785,-0.0188037207375212,-0.0121748645262654));
#37731=CARTESIAN_POINT('Ctrl Pts',(0.00299999886819319,-0.0198037743898623,
-0.0121784592104961));
#37732=CARTESIAN_POINT('Ctrl Pts',(0.0029995152061575,-0.0197742278626064,
-0.0127352619392769));
#37733=CARTESIAN_POINT('Ctrl Pts',(0.00283971737465793,-0.0197446813353506,
-0.0132920447572879));
#37734=CARTESIAN_POINT('Ctrl Pts',(0.00254497588675829,-0.0197151348080947,
-0.0137642794686071));
#37735=CARTESIAN_POINT('Ctrl Pts',(0.00242407139288802,-0.0197030146686839,
-0.0139579926074221));
#37736=CARTESIAN_POINT('Ctrl Pts',(0.00228106202287421,-0.0196908945292731,
-0.0141376490287441));
#37737=CARTESIAN_POINT('Ctrl Pts',(0.00211988397161103,-0.0196787743898623,
-0.0142986090301392));
#37738=CARTESIAN_POINT('Ctrl Pts',(0.00173420051625722,-0.0196497720709318,
-0.0146837707132921));
#37739=CARTESIAN_POINT('Ctrl Pts',(0.00123895300934861,-0.0196207697520013,
-0.0149622775982709));
#37740=CARTESIAN_POINT('Ctrl Pts',(0.000707417383176034,-0.0195917674330708,
-0.0150912538844143));
#37741=CARTESIAN_POINT('Ctrl Pts',(0.000475313460033195,-0.0195791030853346,
-0.0151475735373825));
#37742=CARTESIAN_POINT('Ctrl Pts',(0.000236661332504474,-0.0195664387375985,
-0.0151759684499085));
#37743=CARTESIAN_POINT('Ctrl Pts',(-1.45537485542859E-6,-0.0195537743898623,
-0.0151758529335388));
#37744=CARTESIAN_POINT('Ctrl Pts',(-0.000548777249974811,-0.0195246648215881,
-0.0151755874140092));
#37745=CARTESIAN_POINT('Ctrl Pts',(-0.00109783405214176,-0.0194955552533139,
-0.0150212090217193));
#37746=CARTESIAN_POINT('Ctrl Pts',(-0.00156601259674953,-0.0194664456850397,
-0.0147346820316721));
#37747=CARTESIAN_POINT('Ctrl Pts',(-0.00176797244701259,-0.0194538885866472,
-0.0146110818610263));
#37748=CARTESIAN_POINT('Ctrl Pts',(-0.00195503796625831,-0.0194413314882548,
-0.0144635537821148));
#37749=CARTESIAN_POINT('Ctrl Pts',(-0.00212194257711093,-0.0194287743898623,
-0.014296551213997));
#37750=CARTESIAN_POINT('Ctrl Pts',(-0.00250878408897936,-0.0193996702991963,
-0.0139094826626457));
#37751=CARTESIAN_POINT('Ctrl Pts',(-0.00278792764284432,-0.0193705662085304,
-0.0134122296558984));
#37752=CARTESIAN_POINT('Ctrl Pts',(-0.00291650177595357,-0.0193414621178644,
-0.0128787169937302));
#37753=CARTESIAN_POINT('Ctrl Pts',(-0.00297199989604426,-0.0193288995418637,
-0.0126484300061464));
#37754=CARTESIAN_POINT('Ctrl Pts',(-0.00300002398420702,-0.019316336965863,
-0.0124117461089284));
#37755=CARTESIAN_POINT('Ctrl Pts',(-0.00299999998451356,-0.0193037743898623,
-0.0121755484609993));
#37756=CARTESIAN_POINT('Ctrl Pts',(-0.00299994438371526,-0.0192746702991963,
-0.0116283423975273));
#37757=CARTESIAN_POINT('Ctrl Pts',(-0.00284583965861221,-0.0192455662085304,
-0.0110793236615489));
#37758=CARTESIAN_POINT('Ctrl Pts',(-0.00255959261512691,-0.0192164621178644,
-0.0106110895201743));
#37759=CARTESIAN_POINT('Ctrl Pts',(-0.00243603609243631,-0.0192038995418637,
-0.0104089795468838));
#37760=CARTESIAN_POINT('Ctrl Pts',(-0.00228852293779553,-0.019191336965863,
-0.0102217656692403));
#37761=CARTESIAN_POINT('Ctrl Pts',(-0.00212151157134427,-0.0191787743898623,
-0.010054724188023));
#37762=CARTESIAN_POINT('Ctrl Pts',(-0.00173451858726122,-0.0191496648215881,
-0.00966766142304171));
#37763=CARTESIAN_POINT('Ctrl Pts',(-0.00123726600657303,-0.0191205552533139,
-0.00938829991716738));
#37764=CARTESIAN_POINT('Ctrl Pts',(-0.000703688884394736,-0.0190914456850397,
-0.00925955049809815));
#37765=CARTESIAN_POINT('Ctrl Pts',(-0.000473517816241132,-0.0190788885866472,
-0.0092040114015373));
#37766=CARTESIAN_POINT('Ctrl Pts',(-0.000236945933484557,-0.0190663314882548,
-0.00917591996428969));
#37767=CARTESIAN_POINT('Ctrl Pts',(-8.45723782757253E-7,-0.0190537743898623,
-0.00917585340576622));
#37768=CARTESIAN_POINT('Ctrl Pts',(0.000544459677777046,-0.0190247720709318,
-0.00917569967984446));
#37769=CARTESIAN_POINT('Ctrl Pts',(0.0010917805481729,-0.0189957697520013,
-0.00932855996767236));
#37770=CARTESIAN_POINT('Ctrl Pts',(0.00155900648058052,-0.0189667674330708,
-0.00961274993446557));
#37771=CARTESIAN_POINT('Ctrl Pts',(0.00176302850011425,-0.0189541030853346,
-0.00973684623763436));
#37772=CARTESIAN_POINT('Ctrl Pts',(0.00195193435715708,-0.0189414387375985,
-0.00988530686974216));
#37773=CARTESIAN_POINT('Ctrl Pts',(0.00212031530797329,-0.0189287743898623,
-0.0100535283833507));
#37774=CARTESIAN_POINT('Ctrl Pts',(0.00251315609664262,-0.0188992278626065,
-0.0104459971974108));
#37775=CARTESIAN_POINT('Ctrl Pts',(0.00279493305266735,-0.0188696813353506,
-0.0109515458766621));
#37776=CARTESIAN_POINT('Ctrl Pts',(0.00292154795597086,-0.0188401348080948,
-0.0114942687056274));
#37777=CARTESIAN_POINT('Ctrl Pts',(0.00297348604893989,-0.018828014668684,
-0.0117168964375275));
#37778=CARTESIAN_POINT('Ctrl Pts',(0.00299984735059131,-0.0188158945292731,
-0.0119454535977987));
#37779=CARTESIAN_POINT('Ctrl Pts',(0.00299999933581561,-0.0188037743898623,
-0.0121738570135582));
#37780=CARTESIAN_POINT('',(0.00299995600267922,-0.0178036976750793,-0.0121755209840925));
#37781=CARTESIAN_POINT('Ctrl Pts',(0.00299999999994139,-0.0188036670851801,
-0.0121758720389726));
#37782=CARTESIAN_POINT('Ctrl Pts',(0.00299999651950407,-0.0187741306257539,
-0.0127326703103992));
#37783=CARTESIAN_POINT('Ctrl Pts',(0.00284068144842702,-0.0187445941663278,
-0.0132895868137558));
#37784=CARTESIAN_POINT('Ctrl Pts',(0.00254635158034459,-0.0187150577069016,
-0.0137620732048786));
#37785=CARTESIAN_POINT('Ctrl Pts',(0.00242551900903975,-0.0187029319706895,
-0.0139560451789696));
#37786=CARTESIAN_POINT('Ctrl Pts',(0.00228253407654152,-0.0186908062344774,
-0.0141359570825797));
#37787=CARTESIAN_POINT('Ctrl Pts',(0.00212133886195709,-0.0186786804982654,
-0.0142971551115586));
#37788=CARTESIAN_POINT('Ctrl Pts',(0.00173592684308017,-0.018649688294707,
-0.0146825738595526));
#37789=CARTESIAN_POINT('Ctrl Pts',(0.0012408800814106,-0.0186206960911486,
-0.0149614183555681));
#37790=CARTESIAN_POINT('Ctrl Pts',(0.00070944204344864,-0.0185917038875902,
-0.0150907618592216));
#37791=CARTESIAN_POINT('Ctrl Pts',(0.000477196304749861,-0.0185790338955104,
-0.0151472867509421));
#37792=CARTESIAN_POINT('Ctrl Pts',(0.000238372674535684,-0.0185663639034305,
-0.0151758476355391));
#37793=CARTESIAN_POINT('Ctrl Pts',(7.11305807639468E-8,-0.0185536939113506,
-0.0151758532857148));
#37794=CARTESIAN_POINT('Ctrl Pts',(-0.000547241156960315,-0.0185245944677076,
-0.0151758662625951));
#37795=CARTESIAN_POINT('Ctrl Pts',(-0.00109636875609812,-0.0184954950240646,
-0.0150217724696189));
#37796=CARTESIAN_POINT('Ctrl Pts',(-0.00156468889345413,-0.0184663955804216,
-0.0147354916724832));
#37797=CARTESIAN_POINT('Ctrl Pts',(-0.00176687110051442,-0.0184538328284263,
-0.0146118991151982));
#37798=CARTESIAN_POINT('Ctrl Pts',(-0.00195414785241674,-0.0184412700764311,
-0.0144643331888976));
#37799=CARTESIAN_POINT('Ctrl Pts',(-0.00212123826661812,-0.0184287073244359,
-0.0142972557038837));
#37800=CARTESIAN_POINT('Ctrl Pts',(-0.00250820164891467,-0.018399613345429,
-0.0139103222641914));
#37801=CARTESIAN_POINT('Ctrl Pts',(-0.00278750859192168,-0.0183705193664222,
-0.013413170836358));
#37802=CARTESIAN_POINT('Ctrl Pts',(-0.00291626247755638,-0.0183414253874153,
-0.0128797092107334));
#37803=CARTESIAN_POINT('Ctrl Pts',(-0.00297188246430367,-0.0183288571707839,
-0.0126492607982357));
#37804=CARTESIAN_POINT('Ctrl Pts',(-0.00299998730878829,-0.0183162889541526,
-0.0124123960596514));
#37805=CARTESIAN_POINT('Ctrl Pts',(-0.0029999999956791,-0.0183037207375212,
-0.0121760143001341));
#37806=CARTESIAN_POINT('Ctrl Pts',(-0.00300002936437523,-0.0182746267585143,
-0.0116288176571484));
#37807=CARTESIAN_POINT('Ctrl Pts',(-0.00284601496634515,-0.0182455327795075,
-0.0110797824871448));
#37808=CARTESIAN_POINT('Ctrl Pts',(-0.00255984835774281,-0.0182164388005006,
-0.010611507932948));
#37809=CARTESIAN_POINT('Ctrl Pts',(-0.00243622814310224,-0.0182038705838692,
-0.0104092194787386));
#37810=CARTESIAN_POINT('Ctrl Pts',(-0.00228861112392049,-0.0181913023672379,
-0.0102218466845278));
#37811=CARTESIAN_POINT('Ctrl Pts',(-0.0021214659707898,-0.0181787341506065,
-0.0100546785802265));
#37812=CARTESIAN_POINT('Ctrl Pts',(-0.00173447145069292,-0.0181496347069635,
-0.00966763092082484));
#37813=CARTESIAN_POINT('Ctrl Pts',(-0.00123722194394823,-0.0181205352633204,
-0.00938828187359959));
#37814=CARTESIAN_POINT('Ctrl Pts',(-0.000703650603191536,-0.0180914358196774,
-0.00925954126130631));
#37815=CARTESIAN_POINT('Ctrl Pts',(-0.000473298280723861,-0.0180788730676822,
-0.0092039616287953));
#37816=CARTESIAN_POINT('Ctrl Pts',(-0.000236535431579815,-0.0180663103156869,
-0.00917587305804289));
#37817=CARTESIAN_POINT('Ctrl Pts',(-2.50896571037858E-7,-0.0180537475636917,
-0.00917585329704962));
#37818=CARTESIAN_POINT('Ctrl Pts',(0.000545044381030049,-0.0180247553601333,
-0.009175807692811));
#37819=CARTESIAN_POINT('Ctrl Pts',(0.0010923268375626,-0.017995763156575,
-0.00932877105354029));
#37820=CARTESIAN_POINT('Ctrl Pts',(0.00155949201344859,-0.0179667709530166,
-0.00961304532262673));
#37821=CARTESIAN_POINT('Ctrl Pts',(0.00176364962659962,-0.0179541009609367,
-0.00973727709171541));
#37822=CARTESIAN_POINT('Ctrl Pts',(0.00195266270700665,-0.0179414309688569,
-0.00988590854610536));
#37823=CARTESIAN_POINT('Ctrl Pts',(0.00212111114414092,-0.017928760976777,
-0.0100543237642084));
#37824=CARTESIAN_POINT('Ctrl Pts',(0.00251380045266248,-0.0178992245173508,
-0.0104469356320686));
#37825=CARTESIAN_POINT('Ctrl Pts',(0.00279538695390489,-0.0178696880579247,
-0.0109525844923845));
#37826=CARTESIAN_POINT('Ctrl Pts',(0.00292180002846733,-0.0178401515984985,
-0.0114953500950532));
#37827=CARTESIAN_POINT('Ctrl Pts',(0.0029736969594361,-0.0178280258622864,
-0.0117181741115675));
#37828=CARTESIAN_POINT('Ctrl Pts',(0.00299997401495591,-0.0178159001260744,
-0.0119469275970063));
#37829=CARTESIAN_POINT('Ctrl Pts',(0.00299999998064488,-0.0178037743898623,
-0.0121755125069922));
#37830=CARTESIAN_POINT('',(-0.00267238707576395,-0.0173796339931718,-0.0135401565297772));
#37831=CARTESIAN_POINT('Ctrl Pts',(0.00299880969160871,-0.0178016980599612,
-0.0121757419446065));
#37832=CARTESIAN_POINT('Ctrl Pts',(0.00299841265092597,-0.0177739447125569,
-0.0126975268287903));
#37833=CARTESIAN_POINT('Ctrl Pts',(0.00286181894313852,-0.01774972903045,
-0.0132226923897836));
#37834=CARTESIAN_POINT('Ctrl Pts',(0.00260148942570033,-0.0177223184482828,
-0.0136736443513037));
#37835=CARTESIAN_POINT('Ctrl Pts',(0.00252897879046934,-0.0177146836677764,
-0.0137992498282018));
#37836=CARTESIAN_POINT('Ctrl Pts',(0.00244688739981009,-0.0177068010230323,
-0.0139192469917063));
#37837=CARTESIAN_POINT('Ctrl Pts',(0.00235675099364363,-0.0176985250299721,
-0.0140330646766062));
#37838=CARTESIAN_POINT('Ctrl Pts',(0.00194300311890452,-0.0176605362229444,
-0.0145555153404158));
#37839=CARTESIAN_POINT('Ctrl Pts',(0.00134957914778,-0.0176246399761912,
-0.0149356135552591));
#37840=CARTESIAN_POINT('Ctrl Pts',(0.000701575655805405,-0.0175919594685167,
-0.0150930770227462));
#37841=CARTESIAN_POINT('Ctrl Pts',(0.00052847864049833,-0.0175832297341754,
-0.0151351392285514));
#37842=CARTESIAN_POINT('Ctrl Pts',(0.000351920136921582,-0.0175739186146666,
-0.015162498550165));
#37843=CARTESIAN_POINT('Ctrl Pts',(0.000174231884956872,-0.0175642883153518,
-0.0151731005712262));
#37844=CARTESIAN_POINT('Ctrl Pts',(-0.000313271042439478,-0.0175378667649355,
-0.0152021881234221));
#37845=CARTESIAN_POINT('Ctrl Pts',(-0.000810188572686238,-0.0175090426645311,
-0.015104128674824));
#37846=CARTESIAN_POINT('Ctrl Pts',(-0.00125381412214389,-0.0174832309972516,
-0.0149001412679313));
#37847=CARTESIAN_POINT('Ctrl Pts',(-0.00170800994607117,-0.0174568043148811,
-0.0146912934491848));
#37848=CARTESIAN_POINT('Ctrl Pts',(-0.00211381185151582,-0.0174333575875628,
-0.0143671701585034));
#37849=CARTESIAN_POINT('Ctrl Pts',(-0.00241105511171453,-0.0174070539795054,
-0.013965019431062));
#37850=CARTESIAN_POINT('Ctrl Pts',(-0.00250995731168941,-0.0173983019401744,
-0.0138312112106877));
#37851=CARTESIAN_POINT('Ctrl Pts',(-0.00259702259284883,-0.0173892336148329,
-0.0136887408954094));
#37852=CARTESIAN_POINT('Ctrl Pts',(-0.00267238707576395,-0.0173796339931718,
-0.0135401565297772));
#37853=CARTESIAN_POINT('',(-0.000927050983124835,-0.0173787743898723,-0.0150290228354436));
#37854=CARTESIAN_POINT('Origin',(0.,-0.0173787743898623,-0.0121758532865581));
#37855=CARTESIAN_POINT('',(-0.00299905564929069,-0.0191797287809082,-0.012156770087783));
#37856=CARTESIAN_POINT('Ctrl Pts',(-0.000927050983124817,-0.0173787743898723,
-0.0150290228354436));
#37857=CARTESIAN_POINT('Ctrl Pts',(-0.000918484919008519,-0.0173792522203775,
-0.0150318061183941));
#37858=CARTESIAN_POINT('Ctrl Pts',(-0.0009099159702334,-0.0173797313630426,
-0.015034547752181));
#37859=CARTESIAN_POINT('Ctrl Pts',(-0.000891568346580233,-0.0173807595853773,
-0.015040327152537));
#37860=CARTESIAN_POINT('Ctrl Pts',(-0.000881795771413628,-0.0173813086359318,
-0.0150433506027228));
#37861=CARTESIAN_POINT('Ctrl Pts',(-0.000843717427209008,-0.017383452924518,
-0.0150549182603554));
#37862=CARTESIAN_POINT('Ctrl Pts',(-0.000815302129173545,-0.0173850636494666,
-0.015063093587522));
#37863=CARTESIAN_POINT('Ctrl Pts',(-0.000658439221454871,-0.0173939988708078,
-0.0151057241640584));
#37864=CARTESIAN_POINT('Ctrl Pts',(-0.000527936836835853,-0.0174015864401309,
-0.0151320272181851));
#37865=CARTESIAN_POINT('Ctrl Pts',(-0.000260662284274568,-0.0174170165196915,
-0.0151676306870811));
#37866=CARTESIAN_POINT('Ctrl Pts',(-0.000124114522098636,-0.0174248403265584,
-0.0151763991948485));
#37867=CARTESIAN_POINT('Ctrl Pts',(8.99157383655247E-5,-0.0174368109280743,
-0.0151755031371412));
#37868=CARTESIAN_POINT('Ctrl Pts',(0.000167233758914984,-0.0174410774295902,
-0.0151721873989718));
#37869=CARTESIAN_POINT('Ctrl Pts',(0.000277013241401311,-0.0174470435289978,
-0.0151632163817411));
#37870=CARTESIAN_POINT('Ctrl Pts',(0.000309640161404375,-0.0174488052436293,
-0.0151600110686811));
#37871=CARTESIAN_POINT('Ctrl Pts',(0.000366934073234336,-0.0174518790810126,
-0.0151534326366392));
#37872=CARTESIAN_POINT('Ctrl Pts',(0.000391623516384989,-0.0174531971911412,
-0.0151502860839234));
#37873=CARTESIAN_POINT('Ctrl Pts',(0.000443388102909554,-0.0174559476592967,
-0.0151430332172639));
#37874=CARTESIAN_POINT('Ctrl Pts',(0.000470452027768219,-0.0174573781020459,
-0.0151388626857293));
#37875=CARTESIAN_POINT('Ctrl Pts',(0.000542772580701761,-0.01746118163024,
-0.0151267022518846));
#37876=CARTESIAN_POINT('Ctrl Pts',(0.000587909812379087,-0.0174635354913767,
-0.0151180419295527));
#37877=CARTESIAN_POINT('Ctrl Pts',(0.00088264247281882,-0.0174787983870967,
-0.0150544386762684));
#37878=CARTESIAN_POINT('Ctrl Pts',(0.00112453661194926,-0.0174907069809869,
-0.0149688335306828));
#37879=CARTESIAN_POINT('Ctrl Pts',(0.00145117848234948,-0.017508005925314,
-0.0148038302623325));
#37880=CARTESIAN_POINT('Ctrl Pts',(0.00154686784903474,-0.017513259869844,
-0.014748668705615));
#37881=CARTESIAN_POINT('Ctrl Pts',(0.00169003181277015,-0.0175217048364162,
-0.014655260991457));
#37882=CARTESIAN_POINT('Ctrl Pts',(0.00173975149240897,-0.0175247559550493,
-0.0146206301572248));
#37883=CARTESIAN_POINT('Ctrl Pts',(0.00180432459532359,-0.0175289228850042,
-0.0145726859583269));
#37884=CARTESIAN_POINT('Ctrl Pts',(0.00182014527386188,-0.0175299607042177,
-0.0145606940030742));
#37885=CARTESIAN_POINT('Ctrl Pts',(0.00184617982711892,-0.017531698742836,
-0.014540550050632));
#37886=CARTESIAN_POINT('Ctrl Pts',(0.00185646174728182,-0.0175323931044592,
-0.014532486586037));
#37887=CARTESIAN_POINT('Ctrl Pts',(0.0018768074825597,-0.0175337836657031,
-0.0145163149273462));
#37888=CARTESIAN_POINT('Ctrl Pts',(0.00188687188825807,-0.017534479814909,
-0.01450820863589));
#37889=CARTESIAN_POINT('Ctrl Pts',(0.00191302623527904,-0.0175363103203988,
-0.0144868627602179));
#37890=CARTESIAN_POINT('Ctrl Pts',(0.00192903078585154,-0.0175374517634064,
-0.0144735204386002));
#37891=CARTESIAN_POINT('Ctrl Pts',(0.00199935852172301,-0.0175425574631231,
-0.014413638443835));
#37892=CARTESIAN_POINT('Ctrl Pts',(0.0020521426919352,-0.0175466303085446,
-0.0143653340052529));
#37893=CARTESIAN_POINT('Ctrl Pts',(0.00223175912897695,-0.0175612048398428,
-0.0141887563597442));
#37894=CARTESIAN_POINT('Ctrl Pts',(0.00234870794347416,-0.0175720046632656,
-0.0140509800559048));
#37895=CARTESIAN_POINT('Ctrl Pts',(0.00252958870975051,-0.0175903407089791,
-0.013794205611741));
#37896=CARTESIAN_POINT('Ctrl Pts',(0.00259921253975879,-0.0175979852034743,
-0.0136798428414295));
#37897=CARTESIAN_POINT('Ctrl Pts',(0.0026803422836706,-0.0176076617832214,
-0.0135240089192594));
#37898=CARTESIAN_POINT('Ctrl Pts',(0.00269892488473315,-0.0176099439778581,
-0.0134864115983019));
#37899=CARTESIAN_POINT('Ctrl Pts',(0.00272684224164531,-0.0176134812343224,
-0.0134268135134082));
#37900=CARTESIAN_POINT('Ctrl Pts',(0.00273671233177929,-0.0176147552824252,
-0.0134050708263808));
#37901=CARTESIAN_POINT('Ctrl Pts',(0.00275473905673241,-0.0176171279366588,
-0.013364066289527));
#37902=CARTESIAN_POINT('Ctrl Pts',(0.00276295581151654,-0.0176182286280351,
-0.0133448325960253));
#37903=CARTESIAN_POINT('Ctrl Pts',(0.00278102587221311,-0.0176206942546393,
-0.0133012792212089));
#37904=CARTESIAN_POINT('Ctrl Pts',(0.00279076266919065,-0.0176220550317912,
-0.0132769128764347));
#37905=CARTESIAN_POINT('Ctrl Pts',(0.00281516304515299,-0.0176255532327253,
-0.013213446928504));
#37906=CARTESIAN_POINT('Ctrl Pts',(0.00282933243217529,-0.0176276736171813,
-0.0131741627323976));
#37907=CARTESIAN_POINT('Ctrl Pts',(0.00289604662473854,-0.0176381471346402,
-0.0129763544027179));
#37908=CARTESIAN_POINT('Ctrl Pts',(0.00293611296146069,-0.0176460798742083,
-0.0128139252942959));
#37909=CARTESIAN_POINT('Ctrl Pts',(0.00298701088980831,-0.0176612196264104,
-0.0124952424427378));
#37910=CARTESIAN_POINT('Ctrl Pts',(0.00299955892181305,-0.0176684227891603,
-0.0123398182771641));
#37911=CARTESIAN_POINT('Ctrl Pts',(0.00300018665214758,-0.017679487081178,
-0.0121123592065175));
#37912=CARTESIAN_POINT('Ctrl Pts',(0.00299780893032342,-0.0176830553993994,
-0.0120406069738473));
#37913=CARTESIAN_POINT('Ctrl Pts',(0.00299147775181801,-0.0176877884040497,
-0.0119489977157236));
#37914=CARTESIAN_POINT('Ctrl Pts',(0.00298989362807892,-0.0176888326710539,
-0.0119289957613114));
#37915=CARTESIAN_POINT('Ctrl Pts',(0.00298698161741509,-0.0176905550568207,
-0.0118963868733524));
#37916=CARTESIAN_POINT('Ctrl Pts',(0.00298577427053765,-0.0176912264214951,
-0.0118837699860754));
#37917=CARTESIAN_POINT('Ctrl Pts',(0.00298331897577259,-0.0176925157476851,
-0.0118597201809043));
#37918=CARTESIAN_POINT('Ctrl Pts',(0.00298208522555795,-0.0176931327890869,
-0.0118482865752693));
#37919=CARTESIAN_POINT('Ctrl Pts',(0.0029786681784155,-0.0176947645310459,
-0.0118182402523259));
#37920=CARTESIAN_POINT('Ctrl Pts',(0.00297637619270419,-0.0176957849567514,
-0.0117996406827138));
#37921=CARTESIAN_POINT('Ctrl Pts',(0.002967501834458,-0.0176994867668378,
-0.011732790937164));
#37922=CARTESIAN_POINT('Ctrl Pts',(0.00295991940624405,-0.0177022149922086,
-0.0116846832711209));
#37923=CARTESIAN_POINT('Ctrl Pts',(0.00291460480321268,-0.0177165460313655,
-0.0114366054381575));
#37924=CARTESIAN_POINT('Ctrl Pts',(0.00285776866025242,-0.017728711700786,
-0.0112406708531797));
#37925=CARTESIAN_POINT('Ctrl Pts',(0.00272471409561269,-0.0177494102852254,
-0.0109113607472286));
#37926=CARTESIAN_POINT('Ctrl Pts',(0.00265730059788534,-0.0177580593755,
-0.0107752206813554));
#37927=CARTESIAN_POINT('Ctrl Pts',(0.00256047818768718,-0.0177684462594944,
-0.0106120774157992));
#37928=CARTESIAN_POINT('Ctrl Pts',(0.00254046792852701,-0.0177705050518907,
-0.0105797748407188));
#37929=CARTESIAN_POINT('Ctrl Pts',(0.00250674917800025,-0.0177738363525339,
-0.0105275841115992));
#37930=CARTESIAN_POINT('Ctrl Pts',(0.00249340504967478,-0.0177751216897858,
-0.0105074666353051));
#37931=CARTESIAN_POINT('Ctrl Pts',(0.00246694636720748,-0.0177776078628876,
-0.010468604379082));
#37932=CARTESIAN_POINT('Ctrl Pts',(0.00245385739440067,-0.017778809511288,
-0.0104498442667652));
#37933=CARTESIAN_POINT('Ctrl Pts',(0.00242228106103653,-0.0177816434925442,
-0.010405671973726));
#37934=CARTESIAN_POINT('Ctrl Pts',(0.00240360630183731,-0.0177832687574654,
-0.0103803967267592));
#37935=CARTESIAN_POINT('Ctrl Pts',(0.00233991100216624,-0.0177886509606342,
-0.0102969639869986));
#37936=CARTESIAN_POINT('Ctrl Pts',(0.00229314845641496,-0.0177923427698239,
-0.0102401674479122));
#37937=CARTESIAN_POINT('Ctrl Pts',(0.00209020256090864,-0.0178074448423757,
-0.010011364431285));
#37938=CARTESIAN_POINT('Ctrl Pts',(0.00191641050047461,-0.0178181970206191,
-0.00985608512780436));
#37939=CARTESIAN_POINT('Ctrl Pts',(0.00167661075217465,-0.0178324458720628,
-0.00968734163058456));
#37940=CARTESIAN_POINT('Ctrl Pts',(0.00162571692605577,-0.0178354452406854,
-0.00965379902379728));
#37941=CARTESIAN_POINT('Ctrl Pts',(0.00153927769305174,-0.0178405569903873,
-0.00960053344546228));
#37942=CARTESIAN_POINT('Ctrl Pts',(0.00150428872153922,-0.0178426307737637,
-0.0095799404885922));
#37943=CARTESIAN_POINT('Ctrl Pts',(0.00145382074309139,-0.0178456437713906,
-0.00955160022974656));
#37944=CARTESIAN_POINT('Ctrl Pts',(0.00143867467761251,-0.0178465507506309,
-0.00954326634511958));
#37945=CARTESIAN_POINT('Ctrl Pts',(0.00141219763905639,-0.017848142451736,
-0.00952899449583122));
#37946=CARTESIAN_POINT('Ctrl Pts',(0.00140089895638865,-0.0178488236499623,
-0.00952299713868346));
#37947=CARTESIAN_POINT('Ctrl Pts',(0.00137630459106438,-0.0178503112711572,
-0.00951014335386279));
#37948=CARTESIAN_POINT('Ctrl Pts',(0.00136299562904553,-0.0178511192026931,
-0.00950331391936947));
#37949=CARTESIAN_POINT('Ctrl Pts',(0.00132473402221249,-0.0178534490412603,
-0.00948404028108089));
#37950=CARTESIAN_POINT('Ctrl Pts',(0.00129965878469903,-0.0178549845503533,
-0.00947184433286688));
#37951=CARTESIAN_POINT('Ctrl Pts',(0.00109688320724374,-0.017867449195163,
-0.0093766915954745));
#37952=CARTESIAN_POINT('Ctrl Pts',(0.000911617884956722,-0.0178790952266145,
-0.00931099659349189));
#37953=CARTESIAN_POINT('Ctrl Pts',(0.000566779390770429,-0.0178999135766266,
-0.0092255827629516));
#37954=CARTESIAN_POINT('Ctrl Pts',(0.00040946355650682,-0.0179091110500029,
-0.00919966701156135));
#37955=CARTESIAN_POINT('Ctrl Pts',(0.000198575408085529,-0.0179208578909511,
-0.00918197345430626));
#37956=CARTESIAN_POINT('Ctrl Pts',(0.000146223533100969,-0.0179237288079131,
-0.00917896026468511));
#37957=CARTESIAN_POINT('Ctrl Pts',(6.69574811337146E-5,-0.017928008601673,
-0.00917648021046679));
#37958=CARTESIAN_POINT('Ctrl Pts',(4.00870642307179E-5,-0.0179294478222835,
-0.00917600074943157));
#37959=CARTESIAN_POINT('Ctrl Pts',(-6.76178468817044E-6,-0.0179319376254472,
-0.00917579440596316));
#37960=CARTESIAN_POINT('Ctrl Pts',(-2.67374854965956E-5,-0.0179329930704657,
-0.0091759059301255));
#37961=CARTESIAN_POINT('Ctrl Pts',(-7.20073707692166E-5,-0.0179353715193671,
-0.00917661088145549));
#37962=CARTESIAN_POINT('Ctrl Pts',(-9.72983143109419E-5,-0.0179366907629061,
-0.00917732478827978));
#37963=CARTESIAN_POINT('Ctrl Pts',(-0.000165862173926824,-0.0179402430927888,
-0.00918012859687431));
#37964=CARTESIAN_POINT('Ctrl Pts',(-0.000209104473442932,-0.017942457314688,
-0.00918283604053157));
#37965=CARTESIAN_POINT('Ctrl Pts',(-0.000516292156398082,-0.017958030295056,
-0.00920875972505409));
#37966=CARTESIAN_POINT('Ctrl Pts',(-0.000776179042377204,-0.0179702501749041,
-0.00926591360868667));
#37967=CARTESIAN_POINT('Ctrl Pts',(-0.001099977292886,-0.0179867437199379,
-0.00938365285892597));
#37968=CARTESIAN_POINT('Ctrl Pts',(-0.00117365291519255,-0.01799059922073,
-0.00941381222105218));
#37969=CARTESIAN_POINT('Ctrl Pts',(-0.0012902773268246,-0.0179969924597811,
-0.00946706213416999));
#37970=CARTESIAN_POINT('Ctrl Pts',(-0.00133401628003306,-0.0179994588246775,
-0.00948833302358071));
#37971=CARTESIAN_POINT('Ctrl Pts',(-0.00139340407198984,-0.0180029281642065,
-0.00951902113233563));
#37972=CARTESIAN_POINT('Ctrl Pts',(-0.00140951462523009,-0.018003881788604,
-0.00952753297119871));
#37973=CARTESIAN_POINT('Ctrl Pts',(-0.0014367034093368,-0.018005514062931,
-0.00954221623841134));
#37974=CARTESIAN_POINT('Ctrl Pts',(-0.00144782214192675,-0.0180061881575623,
-0.00954831226309777));
#37975=CARTESIAN_POINT('Ctrl Pts',(-0.00147104787132347,-0.0180076107277387,
-0.00956123832848776));
#37976=CARTESIAN_POINT('Ctrl Pts',(-0.00148314647888632,-0.0180083600106268,
-0.00956808226029));
#37977=CARTESIAN_POINT('Ctrl Pts',(-0.00151627684546927,-0.0180104336312767,
-0.00958712855101086));
#37978=CARTESIAN_POINT('Ctrl Pts',(-0.00153720807933166,-0.0180117680844417,
-0.00959950267479505));
#37979=CARTESIAN_POINT('Ctrl Pts',(-0.00168250846336647,-0.0180211906087799,
-0.0096878023381588));
#37980=CARTESIAN_POINT('Ctrl Pts',(-0.00180134236042741,-0.0180297104872719,
-0.00977244094249443));
#37981=CARTESIAN_POINT('Ctrl Pts',(-0.00200269531583522,-0.0180450840700167,
-0.0099392016808822));
#37982=CARTESIAN_POINT('Ctrl Pts',(-0.00208749953127519,-0.0180519094353813,
-0.010018135434828));
#37983=CARTESIAN_POINT('Ctrl Pts',(-0.00222794506239104,-0.0180636805546593,
-0.010164909089136));
#37984=CARTESIAN_POINT('Ctrl Pts',(-0.00228557395368082,-0.0180686726461414,
-0.0102306568271619));
#37985=CARTESIAN_POINT('Ctrl Pts',(-0.00237898341557835,-0.0180770229545888,
-0.0103471188508274));
#37986=CARTESIAN_POINT('Ctrl Pts',(-0.00241621117623581,-0.0180804314683752,
-0.0103965961251811));
#37987=CARTESIAN_POINT('Ctrl Pts',(-0.00246824428271427,-0.0180853183753977,
-0.0104703984040806));
#37988=CARTESIAN_POINT('Ctrl Pts',(-0.00248427532931604,-0.0180868425666843,
-0.0104938359384863));
#37989=CARTESIAN_POINT('Ctrl Pts',(-0.00251213837088896,-0.0180895261514575,
-0.0105358394932248));
#37990=CARTESIAN_POINT('Ctrl Pts',(-0.00252410312446807,-0.0180906904276781,
-0.0105543145454972));
#37991=CARTESIAN_POINT('Ctrl Pts',(-0.00254896817512699,-0.0180931362891017,
-0.0105936514145953));
#37992=CARTESIAN_POINT('Ctrl Pts',(-0.00256181817710261,-0.0180944159790963,
-0.0106145431969307));
#37993=CARTESIAN_POINT('Ctrl Pts',(-0.00259579213524361,-0.0180978440542813,
-0.010671327618906));
#37994=CARTESIAN_POINT('Ctrl Pts',(-0.00261642763928695,-0.01809997493894,
-0.0107075069656226));
#37995=CARTESIAN_POINT('Ctrl Pts',(-0.00275305708827867,-0.018114456124006,
-0.0109590852973342));
#37996=CARTESIAN_POINT('Ctrl Pts',(-0.00284307444529361,-0.0181258397605986,
-0.0111875306139982));
#37997=CARTESIAN_POINT('Ctrl Pts',(-0.00292821460363338,-0.0181419929030586,
-0.0115165882016262));
#37998=CARTESIAN_POINT('Ctrl Pts',(-0.00294766632742895,-0.0181465596277272,
-0.0116098739897278));
#37999=CARTESIAN_POINT('Ctrl Pts',(-0.002968497591926,-0.0181531232725227,
-0.0117406464368854));
#38000=CARTESIAN_POINT('Ctrl Pts',(-0.00297366409534073,-0.0181549895615279,
-0.0117774758223127));
#38001=CARTESIAN_POINT('Ctrl Pts',(-0.00298153752097113,-0.0181583223382188,
-0.011842346093858));
#38002=CARTESIAN_POINT('Ctrl Pts',(-0.00298453664821187,-0.0181597757640042,
-0.0118703472753936));
#38003=CARTESIAN_POINT('Ctrl Pts',(-0.00298849917548977,-0.0181620180776826,
-0.0119130067490887));
#38004=CARTESIAN_POINT('Ctrl Pts',(-0.00298974990498657,-0.0181627921163158,
-0.0119276374287722));
#38005=CARTESIAN_POINT('Ctrl Pts',(-0.00299186212529958,-0.0181642332051021,
-0.0119546838771571));
#38006=CARTESIAN_POINT('Ctrl Pts',(-0.00299275383806924,-0.0181648986253354,
-0.0119670966584653));
#38007=CARTESIAN_POINT('Ctrl Pts',(-0.00299464040581733,-0.018166449678184,
-0.0119958610623202));
#38008=CARTESIAN_POINT('Ctrl Pts',(-0.00299557859394014,-0.018167338284819,
-0.0120122158085731));
#38009=CARTESIAN_POINT('Ctrl Pts',(-0.00299823964601961,-0.0181703002598389,
-0.012066355772898));
#38010=CARTESIAN_POINT('Ctrl Pts',(-0.00299938179577923,-0.0181724015559035,
-0.0121041645983236));
#38011=CARTESIAN_POINT('Ctrl Pts',(-0.00300194485721393,-0.0181851748148728,
-0.0123311696858455));
#38012=CARTESIAN_POINT('Ctrl Pts',(-0.00298617943132953,-0.0181964320611897,
-0.0125201253721847));
#38013=CARTESIAN_POINT('Ctrl Pts',(-0.00293174299641538,-0.0182144740442399,
-0.0128231287328789));
#38014=CARTESIAN_POINT('Ctrl Pts',(-0.00290384614350085,-0.0182213533136839,
-0.012938587749154));
#38015=CARTESIAN_POINT('Ctrl Pts',(-0.0028469503417549,-0.0182323489592065,
-0.013124887673167));
#38016=CARTESIAN_POINT('Ctrl Pts',(-0.00282195737281311,-0.0182365687132353,
-0.0131968089616204));
#38017=CARTESIAN_POINT('Ctrl Pts',(-0.00278304908522534,-0.0182423732966641,
-0.0132963824760266));
#38018=CARTESIAN_POINT('Ctrl Pts',(-0.00277140287654923,-0.0182440305509258,
-0.0133248850819308));
#38019=CARTESIAN_POINT('Ctrl Pts',(-0.00275048100433672,-0.0182468750177217,
-0.0133739190084775));
#38020=CARTESIAN_POINT('Ctrl Pts',(-0.00274140919465408,-0.0182480688692432,
-0.0133945340871935));
#38021=CARTESIAN_POINT('Ctrl Pts',(-0.00272225480458288,-0.0182505109746674,
-0.0134367646827539));
#38022=CARTESIAN_POINT('Ctrl Pts',(-0.00271214486293597,-0.0182517582015689,
-0.0134583660762039));
#38023=CARTESIAN_POINT('Ctrl Pts',(-0.00268539964238647,-0.0182549540149564,
-0.0135137802720378));
#38024=CARTESIAN_POINT('Ctrl Pts',(-0.0026683827406809,-0.0182568895438479,
-0.0135474048048597));
#38025=CARTESIAN_POINT('Ctrl Pts',(-0.00258622891749262,-0.0182658076912017,
-0.0137024167360325));
#38026=CARTESIAN_POINT('Ctrl Pts',(-0.00251341106963634,-0.0182725228024711,
-0.0138195520979423));
#38027=CARTESIAN_POINT('Ctrl Pts',(-0.00239866513169428,-0.0182819081415633,
-0.0139785756081425));
#38028=CARTESIAN_POINT('Ctrl Pts',(-0.00236316238006915,-0.0182846775256849,
-0.0140248708305322));
#38029=CARTESIAN_POINT('Ctrl Pts',(-0.00221034248989368,-0.0182961565445621,
-0.0142125493788301));
#38030=CARTESIAN_POINT('Ctrl Pts',(-0.00208152600560481,-0.0183047973022683,
-0.0143440277435928));
#38031=CARTESIAN_POINT('Ctrl Pts',(-0.00191953404008343,-0.0183156265334936,
-0.0144815463149926));
#38032=CARTESIAN_POINT('Ctrl Pts',(-0.00189728718186802,-0.0183171134459348,
-0.0144998869582831));
#38033=CARTESIAN_POINT('Ctrl Pts',(-0.00186298687060158,-0.0183194114098442,
-0.0145273439042255));
#38034=CARTESIAN_POINT('Ctrl Pts',(-0.00185112261875409,-0.0183202072290333,
-0.0145366949238486));
#38035=CARTESIAN_POINT('Ctrl Pts',(-0.00182942020530571,-0.0183216657294489,
-0.0145535358958784));
#38036=CARTESIAN_POINT('Ctrl Pts',(-0.00181960566740642,-0.0183223264004514,
-0.0145610551813913));
#38037=CARTESIAN_POINT('Ctrl Pts',(-0.00179673602647957,-0.0183238683407411,
-0.0145783531715706));
#38038=CARTESIAN_POINT('Ctrl Pts',(-0.0017836474516084,-0.0183247525469609,
-0.0145880862335798));
#38039=CARTESIAN_POINT('Ctrl Pts',(-0.00174113920935269,-0.0183276280162323,
-0.0146191615462217));
#38040=CARTESIAN_POINT('Ctrl Pts',(-0.00171141181936689,-0.0183296447157395,
-0.0146400753451428));
#38041=CARTESIAN_POINT('Ctrl Pts',(-0.00163794353273847,-0.0183346284267124,
-0.0146897910780535));
#38042=CARTESIAN_POINT('Ctrl Pts',(-0.00159381474987995,-0.018337621505514,
-0.0147179973207889));
#38043=CARTESIAN_POINT('Ctrl Pts',(-0.00139266748649034,-0.0183511898749482,
-0.014839270112602));
#38044=CARTESIAN_POINT('Ctrl Pts',(-0.00122808894718745,-0.0183620645681737,
-0.0149190470496841));
#38045=CARTESIAN_POINT('Ctrl Pts',(-0.0009305144165387,-0.0183805181620509,
-0.015031109936399));
#38046=CARTESIAN_POINT('Ctrl Pts',(-0.00080065356400895,-0.0183882094964906,
-0.0150702113621561));
#38047=CARTESIAN_POINT('Ctrl Pts',(-0.000631988362923594,-0.0183976818669959,
-0.0151087698735885));
#38048=CARTESIAN_POINT('Ctrl Pts',(-0.000595240948658097,-0.0183997158351181,
-0.015116448019551));
#38049=CARTESIAN_POINT('Ctrl Pts',(-0.00053498935202105,-0.0184030034155253,
-0.0151278614301218));
#38050=CARTESIAN_POINT('Ctrl Pts',(-0.000511568514481902,-0.0184042697793336,
-0.0151320101473221));
#38051=CARTESIAN_POINT('Ctrl Pts',(-0.000465924026948051,-0.0184067159678558,
-0.0151395367991225));
#38052=CARTESIAN_POINT('Ctrl Pts',(-0.000443706927339776,-0.0184078966405567,
-0.015142944346944));
#38053=CARTESIAN_POINT('Ctrl Pts',(-0.000391012965124657,-0.0184106742353693,
-0.0151504211754909));
#38054=CARTESIAN_POINT('Ctrl Pts',(-0.000360507431336982,-0.0184122643203087,
-0.0151542722876984));
#38055=CARTESIAN_POINT('Ctrl Pts',(-0.000254320012048163,-0.0184177416490344,
-0.0151660223210573));
#38056=CARTESIAN_POINT('Ctrl Pts',(-0.000178398508522549,-0.0184215555378976,
-0.015171510919069));
#38057=CARTESIAN_POINT('Ctrl Pts',(1.62942335709118E-5,-0.0184311480379168,
-0.0151781568144488));
#38058=CARTESIAN_POINT('Ctrl Pts',(0.000135074762959189,-0.01843681900494,
-0.0151751613586717));
#38059=CARTESIAN_POINT('Ctrl Pts',(0.000442051908924212,-0.0184514360728539,
-0.0151491422132447));
#38060=CARTESIAN_POINT('Ctrl Pts',(0.000628778946377897,-0.0184602780448767,
-0.0151153227570962));
#38061=CARTESIAN_POINT('Ctrl Pts',(0.00084387579589751,-0.0184715422153384,
-0.0150549218703496));
#38062=CARTESIAN_POINT('Ctrl Pts',(0.000876537602384341,-0.0184732836978446,
-0.015045146565961));
#38063=CARTESIAN_POINT('Ctrl Pts',(0.000926185898403631,-0.018475988275298,
-0.0150293605970681));
#38064=CARTESIAN_POINT('Ctrl Pts',(0.000943297455501972,-0.01847693096182,
-0.0150237497328701));
#38065=CARTESIAN_POINT('Ctrl Pts',(0.000972338360798834,-0.0184785504433161,
-0.0150139368043969));
#38066=CARTESIAN_POINT('Ctrl Pts',(0.000984293785566394,-0.0184792228610794,
-0.0150098126517288));
#38067=CARTESIAN_POINT('Ctrl Pts',(0.00100948320279297,-0.0184806522551055,
-0.0150009446644592));
#38068=CARTESIAN_POINT('Ctrl Pts',(0.00102271031074457,-0.0184814101595314,
-0.0149961832733967));
#38069=CARTESIAN_POINT('Ctrl Pts',(0.00105923093844334,-0.0184835221054458,
-0.0149827461720772));
#38070=CARTESIAN_POINT('Ctrl Pts',(0.00108245037191541,-0.0184848867535847,
-0.01497387383062));
#38071=CARTESIAN_POINT('Ctrl Pts',(0.00113486118805761,-0.0184880125837716,
-0.0149530972130958));
#38072=CARTESIAN_POINT('Ctrl Pts',(0.0011639803617351,-0.0184897817333343,
-0.0149410193441623));
#38073=CARTESIAN_POINT('Ctrl Pts',(0.00125967264898238,-0.0184956912102496,
-0.0148995493637679));
#38074=CARTESIAN_POINT('Ctrl Pts',(0.00132536451254645,-0.0184999026308407,
-0.014868194905075));
#38075=CARTESIAN_POINT('Ctrl Pts',(0.00158795291398626,-0.018517207635624,
-0.0147309220473911));
#38076=CARTESIAN_POINT('Ctrl Pts',(0.00177388865768702,-0.0185305055021675,
-0.0146055260507263));
#38077=CARTESIAN_POINT('Ctrl Pts',(0.00200123488529625,-0.0185473586178457,
-0.0144120717906233));
#38078=CARTESIAN_POINT('Ctrl Pts',(0.0020564635410866,-0.0185515147533242,
-0.0143613905878732));
#38079=CARTESIAN_POINT('Ctrl Pts',(0.00213196541663141,-0.0185572852832821,
-0.0142867063771941));
#38080=CARTESIAN_POINT('Ctrl Pts',(0.00215384649450964,-0.0185589690811248,
-0.0142643749375242));
#38081=CARTESIAN_POINT('Ctrl Pts',(0.00219074231952359,-0.018561829142666,
-0.0142255230393797));
#38082=CARTESIAN_POINT('Ctrl Pts',(0.00220592876916227,-0.0185630126606279,
-0.0142091698649165));
#38083=CARTESIAN_POINT('Ctrl Pts',(0.00223674179715954,-0.0185654277426806,
-0.0141752379965831));
#38084=CARTESIAN_POINT('Ctrl Pts',(0.00225234698640823,-0.0185666583781259,
-0.0141576419181095));
#38085=CARTESIAN_POINT('Ctrl Pts',(0.00229153807264962,-0.0185697696352363,
-0.0141123899465485));
#38086=CARTESIAN_POINT('Ctrl Pts',(0.00231483156736769,-0.0185716384107584,
-0.0140844852400283));
#38087=CARTESIAN_POINT('Ctrl Pts',(0.00241967713240745,-0.0185801526549903,
-0.0139541405956519));
#38088=CARTESIAN_POINT('Ctrl Pts',(0.00249497823526368,-0.0185865557142784,
-0.0138468504000259));
#38089=CARTESIAN_POINT('Ctrl Pts',(0.00262320306556077,-0.0185983866296428,
-0.0136360620766611));
#38090=CARTESIAN_POINT('Ctrl Pts',(0.0026775968038788,-0.0186038335245203,
-0.0135337485845328));
#38091=CARTESIAN_POINT('Ctrl Pts',(0.00278676418642777,-0.0186162568771403,
-0.0132961936593528));
#38092=CARTESIAN_POINT('Ctrl Pts',(0.00283786115975335,-0.0186232481531158,
-0.0131595975329385));
#38093=CARTESIAN_POINT('Ctrl Pts',(0.0028856883177898,-0.0186319709246532,
-0.0129964609092769));
#38094=CARTESIAN_POINT('Ctrl Pts',(0.00289225916303313,-0.0186332346704168,
-0.0129729924207941));
#38095=CARTESIAN_POINT('Ctrl Pts',(0.00290214124299736,-0.018635246142386,
-0.0129359657142127));
#38096=CARTESIAN_POINT('Ctrl Pts',(0.00290564515702325,-0.0186359835285071,
-0.0129224595436406));
#38097=CARTESIAN_POINT('Ctrl Pts',(0.00291215593926266,-0.0186374019374999,
-0.0128966229168957));
#38098=CARTESIAN_POINT('Ctrl Pts',(0.00291517896912859,-0.018638082072318,
-0.0128842970960091));
#38099=CARTESIAN_POINT('Ctrl Pts',(0.0029223603674028,-0.0186397511791331,
-0.0128541919052441));
#38100=CARTESIAN_POINT('Ctrl Pts',(0.00292643476657426,-0.0186407446570823,
-0.0128363931585568));
#38101=CARTESIAN_POINT('Ctrl Pts',(0.00294084312829566,-0.0186444331823331,
-0.01277069978802));
#38102=CARTESIAN_POINT('Ctrl Pts',(0.00295016532942999,-0.018647176504052,
-0.0127225933296855));
#38103=CARTESIAN_POINT('Ctrl Pts',(0.00297169507633421,-0.0186545373187582,
-0.0125948088881133));
#38104=CARTESIAN_POINT('Ctrl Pts',(0.00298187662224434,-0.0186592188106461,
-0.0125148311418218));
#38105=CARTESIAN_POINT('Ctrl Pts',(0.0030112364308428,-0.0186791542371746,
-0.012175618893272));
#38106=CARTESIAN_POINT('Ctrl Pts',(0.00299990864153989,-0.018694548752928,
-0.0119148251489048));
#38107=CARTESIAN_POINT('Ctrl Pts',(0.00294753764037032,-0.0187112975705394,
-0.0116155455238202));
#38108=CARTESIAN_POINT('Ctrl Pts',(0.00293903254977725,-0.0187136866274807,
-0.0115725201473627));
#38109=CARTESIAN_POINT('Ctrl Pts',(0.00292412827011347,-0.0187174102377501,
-0.0115049463195372));
#38110=CARTESIAN_POINT('Ctrl Pts',(0.00291835610990155,-0.0187187641205232,
-0.0114802672259961));
#38111=CARTESIAN_POINT('Ctrl Pts',(0.00290697187285675,-0.0187212789467455,
-0.0114342321352796));
#38112=CARTESIAN_POINT('Ctrl Pts',(0.00290143545285589,-0.0187224421853027,
-0.0114128593486722));
#38113=CARTESIAN_POINT('Ctrl Pts',(0.00288844917822966,-0.0187250427038151,
-0.0113649138084039));
#38114=CARTESIAN_POINT('Ctrl Pts',(0.00288086754053546,-0.0187264756892957,
-0.0113383786469758));
#38115=CARTESIAN_POINT('Ctrl Pts',(0.00285659772999105,-0.0187308177926663,
-0.0112576689825859));
#38116=CARTESIAN_POINT('Ctrl Pts',(0.00283873902202718,-0.018733689646804,
-0.0112038582843998));
#38117=CARTESIAN_POINT('Ctrl Pts',(0.00279302483538531,-0.018740368606869,
-0.0110781498884607));
#38118=CARTESIAN_POINT('Ctrl Pts',(0.00276390157584005,-0.0187441375966111,
-0.0110067555537347));
#38119=CARTESIAN_POINT('Ctrl Pts',(0.00267922964590745,-0.0187540270429248,
-0.0108200938288052));
#38120=CARTESIAN_POINT('Ctrl Pts',(0.00261900554806964,-0.0187600454289708,
-0.0107071239595497));
#38121=CARTESIAN_POINT('Ctrl Pts',(0.00247794000393196,-0.0187727852683669,
-0.0104789386038199));
#38122=CARTESIAN_POINT('Ctrl Pts',(0.00239584016960181,-0.0187795034837786,
-0.0103648731580879));
#38123=CARTESIAN_POINT('Ctrl Pts',(0.00228623916622762,-0.0187882134594537,
-0.0102331563447409));
#38124=CARTESIAN_POINT('Ctrl Pts',(0.00226604413571959,-0.0187898091581789,
-0.0102096374371148));
#38125=CARTESIAN_POINT('Ctrl Pts',(0.00223532869343492,-0.0187922298034257,
-0.0101749683862035));
#38126=CARTESIAN_POINT('Ctrl Pts',(0.00222508083600044,-0.0187930364100857,
-0.010163578453037));
#38127=CARTESIAN_POINT('Ctrl Pts',(0.00220635798974131,-0.0187945093161124,
-0.010143086926589));
#38128=CARTESIAN_POINT('Ctrl Pts',(0.0021979130327767,-0.0187951734715535,
-0.0101339588377981));
#38129=CARTESIAN_POINT('Ctrl Pts',(0.00217846153041869,-0.0187967027674732,
-0.0101131943481031));
#38130=CARTESIAN_POINT('Ctrl Pts',(0.00216741838784637,-0.0187975705464111,
-0.0101015934076861));
#38131=CARTESIAN_POINT('Ctrl Pts',(0.00213212446576222,-0.018800340932359,
-0.0100651063398975));
#38132=CARTESIAN_POINT('Ctrl Pts',(0.0021075346904506,-0.0188022666079202,
-0.0100405536034004));
#38133=CARTESIAN_POINT('Ctrl Pts',(0.00204708265341822,-0.0188069776428102,
-0.00998225417201123));
#38134=CARTESIAN_POINT('Ctrl Pts',(0.00201080556407585,-0.0188097857947129,
-0.00994895296830683));
#38135=CARTESIAN_POINT('Ctrl Pts',(0.00185370416222843,-0.0188218106573141,
-0.00981170852525162));
#38136=CARTESIAN_POINT('Ctrl Pts',(0.00172551869541643,-0.0188312773247858,
-0.00971658829210029));
#38137=CARTESIAN_POINT('Ctrl Pts',(0.00145250779188687,-0.0188500958157585,
-0.00954589848615459));
#38138=CARTESIAN_POINT('Ctrl Pts',(0.00130783607067975,-0.0188594072479526,
-0.00947103943413225));
#38139=CARTESIAN_POINT('Ctrl Pts',(0.00112237747470937,-0.0188704236631417,
-0.00939345459053829));
#38140=CARTESIAN_POINT('Ctrl Pts',(0.00108668060028056,-0.0188725052929899,
-0.00937931986860307));
#38141=CARTESIAN_POINT('Ctrl Pts',(0.00102828336085335,-0.0188758493200226,
-0.00935748369149285));
#38142=CARTESIAN_POINT('Ctrl Pts',(0.00100574551628953,-0.0188771253297842,
-0.00934936255668477));
#38143=CARTESIAN_POINT('Ctrl Pts',(0.000961960825911773,-0.018879576829045,
-0.00933417551063117));
#38144=CARTESIAN_POINT('Ctrl Pts',(0.000940727461419175,-0.0188807533529384,
-0.00932707581329203));
#38145=CARTESIAN_POINT('Ctrl Pts',(0.000890637345740944,-0.0188835008336519,
-0.00931094854172757));
#38146=CARTESIAN_POINT('Ctrl Pts',(0.000861719411946828,-0.0188850653682551,
-0.00930211811798917));
#38147=CARTESIAN_POINT('Ctrl Pts',(0.000762870334084337,-0.0188903442350807,
-0.0092735597379996));
#38148=CARTESIAN_POINT('Ctrl Pts',(0.000692355999364761,-0.018893992442587,
-0.00925593493532533));
#38149=CARTESIAN_POINT('Ctrl Pts',(0.000513155010783287,-0.0189030321890254,
-0.00921800204322305));
#38150=CARTESIAN_POINT('Ctrl Pts',(0.000403856658224679,-0.0189083326624521,
-0.00920110728498425));
#38151=CARTESIAN_POINT('Ctrl Pts',(0.0001270887854547,-0.0189215519504282,
-0.00917386488608472));
#38152=CARTESIAN_POINT('Ctrl Pts',(-4.07659455317399E-5,-0.0189293781093705,
-0.00917145355426854));
#38153=CARTESIAN_POINT('Ctrl Pts',(-0.000270584063945929,-0.0189407192226307,
-0.0091874208534722));
#38154=CARTESIAN_POINT('Ctrl Pts',(-0.000333079584316126,-0.0189438694486538,
-0.0091937397458152));
#38155=CARTESIAN_POINT('Ctrl Pts',(-0.000415685638258841,-0.0189481735699036,
-0.00920472096704819));
#38156=CARTESIAN_POINT('Ctrl Pts',(-0.000436015680736784,-0.0189492442070633,
-0.00920763629799436));
#38157=CARTESIAN_POINT('Ctrl Pts',(-0.00046801067381927,-0.0189509492867855,
-0.00921256017412424));
#38158=CARTESIAN_POINT('Ctrl Pts',(-0.000479696754563788,-0.0189515763108307,
-0.00921442946089919));
#38159=CARTESIAN_POINT('Ctrl Pts',(-0.000504139411264349,-0.0189528972621672,
-0.00921848774041169));
#38160=CARTESIAN_POINT('Ctrl Pts',(-0.000516893311202831,-0.0189535919756741,
-0.00922069021066716));
#38161=CARTESIAN_POINT('Ctrl Pts',(-0.000548935157146933,-0.0189553503885891,
-0.00922643727933196));
#38162=CARTESIAN_POINT('Ctrl Pts',(-0.000568203185416867,-0.0189564197285708,
-0.00923008858277464));
#38163=CARTESIAN_POINT('Ctrl Pts',(-0.000646208974282892,-0.0189607935692511,
-0.00924566451245364));
#38164=CARTESIAN_POINT('Ctrl Pts',(-0.000704616025598163,-0.0189641713644821,
-0.00925915864126414));
#38165=CARTESIAN_POINT('Ctrl Pts',(-0.000870190856513358,-0.0189739695716574,
-0.00930267580600117));
#38166=CARTESIAN_POINT('Ctrl Pts',(-0.000976144742771533,-0.0189805075363449,
-0.00933692383123003));
#38167=CARTESIAN_POINT('Ctrl Pts',(-0.00127914553528562,-0.0189996083383301,
-0.00945383667015244));
#38168=CARTESIAN_POINT('Ctrl Pts',(-0.00146959805965129,-0.0190120839588966,
-0.00955175462680121));
#38169=CARTESIAN_POINT('Ctrl Pts',(-0.00168543698521664,-0.0190263354624648,
-0.00969365596630042));
#38170=CARTESIAN_POINT('Ctrl Pts',(-0.00172226538993981,-0.0190287743245499,
-0.00971906603763104));
#38171=CARTESIAN_POINT('Ctrl Pts',(-0.00177919376477361,-0.019032556896985,
-0.00976025375169827));
#38172=CARTESIAN_POINT('Ctrl Pts',(-0.00179968303464,-0.0190339209860502,
-0.0097754798583545));
#38173=CARTESIAN_POINT('Ctrl Pts',(-0.00183750224205979,-0.0190364445993303,
-0.00980434078001927));
#38174=CARTESIAN_POINT('Ctrl Pts',(-0.0018548808948331,-0.0190376065826385,
-0.00981790863944317));
#38175=CARTESIAN_POINT('Ctrl Pts',(-0.00189344946752091,-0.0190401914225397,
-0.00984871018639379));
#38176=CARTESIAN_POINT('Ctrl Pts',(-0.00191455691922286,-0.0190416102010078,
-0.0098660442551721));
#38177=CARTESIAN_POINT('Ctrl Pts',(-0.0019775878686017,-0.0190458622552884,
-0.0099192648663602));
#38178=CARTESIAN_POINT('Ctrl Pts',(-0.00201876174228229,-0.0190486605388356,
-0.00995602298230598));
#38179=CARTESIAN_POINT('Ctrl Pts',(-0.00216649610805912,-0.0190588145612551,
-0.0100954255653499));
#38180=CARTESIAN_POINT('Ctrl Pts',(-0.00226644036631344,-0.0190658996174339,
-0.0102047780845042));
#38181=CARTESIAN_POINT('Ctrl Pts',(-0.0024739548282348,-0.0190818273861348,
-0.0104685820346359));
#38182=CARTESIAN_POINT('Ctrl Pts',(-0.00257588632720747,-0.0190905920918294,
-0.0106266519879419));
#38183=CARTESIAN_POINT('Ctrl Pts',(-0.0026800459744835,-0.0191019664444451,
-0.0108272155986657));
#38184=CARTESIAN_POINT('Ctrl Pts',(-0.00269706224485031,-0.0191039242798969,
-0.0108615759057136));
#38185=CARTESIAN_POINT('Ctrl Pts',(-0.00272002108258788,-0.0191067237943501,
-0.0109102604567793));
#38186=CARTESIAN_POINT('Ctrl Pts',(-0.0027265188216796,-0.0191075352134371,
-0.0109243202283929));
#38187=CARTESIAN_POINT('Ctrl Pts',(-0.00273810155966704,-0.019109017945812,
-0.0109499012349391));
#38188=CARTESIAN_POINT('Ctrl Pts',(-0.00274322351575125,-0.0191096871003701,
-0.0109614055421165));
#38189=CARTESIAN_POINT('Ctrl Pts',(-0.00275383034873737,-0.0191111021260923,
-0.0109856388059851));
#38190=CARTESIAN_POINT('Ctrl Pts',(-0.00275929963053183,-0.0191118488245443,
-0.0109983739308514));
#38191=CARTESIAN_POINT('Ctrl Pts',(-0.00277395699684311,-0.0191138962234051,
-0.0110331663131432));
#38192=CARTESIAN_POINT('Ctrl Pts',(-0.00278296994112422,-0.0191152065238506,
-0.0110552957576228));
#38193=CARTESIAN_POINT('Ctrl Pts',(-0.00283795498855828,-0.0191235216434375,
-0.0111950566839909));
#38194=CARTESIAN_POINT('Ctrl Pts',(-0.00287672125310937,-0.0191308512173997,
-0.0113153767157011));
#38195=CARTESIAN_POINT('Ctrl Pts',(-0.00296744218820184,-0.0191524718374996,
-0.0116727849040339));
#38196=CARTESIAN_POINT('Ctrl Pts',(-0.00299839357336558,-0.0191668035180019,
-0.01191420638761));
#38197=CARTESIAN_POINT('Ctrl Pts',(-0.00299993908917108,-0.019180238095247,
-0.0121567362453802));
#38198=CARTESIAN_POINT('Ctrl Pts',(-0.0029990259773704,-0.0191797116746683,
-0.012156771224441));
#38199=CARTESIAN_POINT('Ctrl Pts',(-0.00299900717703148,-0.0191799305018243,
-0.0121612117764821));
#38200=CARTESIAN_POINT('Ctrl Pts',(-0.00299898627533192,-0.0191801491278106,
-0.0121655716153771));
#38201=CARTESIAN_POINT('Ctrl Pts',(-0.00299896195254882,-0.0191803670938455,
-0.012169853924649));
#38202=CARTESIAN_POINT('',(-0.00299993908917192,-0.0191802380952497,-0.0121567362453771));
#38203=CARTESIAN_POINT('Ctrl Pts',(-0.00299999393119832,-0.0191809619683288,
-0.0121698189717546));
#38204=CARTESIAN_POINT('Ctrl Pts',(-0.00299998955652076,-0.0191808417663619,
-0.0121676440543882));
#38205=CARTESIAN_POINT('Ctrl Pts',(-0.00299998281669984,-0.0191807214956478,
-0.0121654691307674));
#38206=CARTESIAN_POINT('Ctrl Pts',(-0.00299996455983385,-0.0191804802010913,
-0.0121611081457004));
#38207=CARTESIAN_POINT('Ctrl Pts',(-0.00299995301874857,-0.0191803591796904,
-0.0121589221414168));
#38208=CARTESIAN_POINT('Ctrl Pts',(-0.00299993908917192,-0.0191802380952497,
-0.0121567362453771));
#38209=CARTESIAN_POINT('Origin',(0.,-0.0357900992552775,-0.0121758532865581));
#38210=CARTESIAN_POINT('',(-0.00249999995746914,-0.0332901205213028,-0.0121755333059438));
#38211=CARTESIAN_POINT('',(-0.00249999938712155,-0.0322901101338213,-0.0121771834348536));
#38212=CARTESIAN_POINT('Ctrl Pts',(-0.00249999991496748,-0.0332900992552675,
-0.012175201241613));
#38213=CARTESIAN_POINT('Ctrl Pts',(-0.00249987325125826,-0.0332591766194273,
-0.0116895610036931));
#38214=CARTESIAN_POINT('Ctrl Pts',(-0.00235395428532161,-0.0332282539835869,
-0.0112039832265026));
#38215=CARTESIAN_POINT('Ctrl Pts',(-0.00208658183779019,-0.0331973313477467,
-0.0107988361355378));
#38216=CARTESIAN_POINT('Ctrl Pts',(-0.00199368361807678,-0.0331865873169203,
-0.01065806828971));
#38217=CARTESIAN_POINT('Ctrl Pts',(-0.00188657164099081,-0.0331758432860939,
-0.010526864134928));
#38218=CARTESIAN_POINT('Ctrl Pts',(-0.0017675670555371,-0.0331650992552675,
-0.0104078864587641));
#38219=CARTESIAN_POINT('Ctrl Pts',(-0.00143136654560736,-0.0331347462345938,
-0.0100717619704172));
#38220=CARTESIAN_POINT('Ctrl Pts',(-0.00099492120557128,-0.0331043932139202,
-0.00983328515454348));
#38221=CARTESIAN_POINT('Ctrl Pts',(-0.000528748028399615,-0.0330740401932465,
-0.00973240786616019));
#38222=CARTESIAN_POINT('Ctrl Pts',(-0.000354988772124477,-0.0330627265472535,
-0.00969480732742718));
#38223=CARTESIAN_POINT('Ctrl Pts',(-0.000177363740756044,-0.0330514129012605,
-0.00967585943472476));
#38224=CARTESIAN_POINT('Ctrl Pts',(-8.66816036824776E-8,-0.0330400992552675,
-0.00967585328806084));
#38225=CARTESIAN_POINT('Ctrl Pts',(0.000477283201102462,-0.0330096339830744,
-0.00967583673638604));
#38226=CARTESIAN_POINT('Ctrl Pts',(0.000956188035358496,-0.0329791687108814,
-0.00981686733479447));
#38227=CARTESIAN_POINT('Ctrl Pts',(0.0013580605767814,-0.0329487034386883,
-0.0100768841420035));
#38228=CARTESIAN_POINT('Ctrl Pts',(0.0015058200596463,-0.0329375020442147,
-0.0101724864661468));
#38229=CARTESIAN_POINT('Ctrl Pts',(0.00164330762013163,-0.0329263006497411,
-0.0102836723408953));
#38230=CARTESIAN_POINT('Ctrl Pts',(0.00176744445112735,-0.0329150992552675,
-0.0104077638905775));
#38231=CARTESIAN_POINT('Ctrl Pts',(0.00210500519603208,-0.0328846397129049,
-0.0107452015036623));
#38232=CARTESIAN_POINT('Ctrl Pts',(0.00234395658822882,-0.0328541801705422,
-0.0111834403202244));
#38233=CARTESIAN_POINT('Ctrl Pts',(0.00244435914715829,-0.0328237206281795,
-0.0116513455557251));
#38234=CARTESIAN_POINT('Ctrl Pts',(0.0024813007382356,-0.0328125135038755,
-0.0118235041546403));
#38235=CARTESIAN_POINT('Ctrl Pts',(0.00249994188581591,-0.0328013063795715,
-0.0119994240830024));
#38236=CARTESIAN_POINT('Ctrl Pts',(0.00249999986374028,-0.0327900992552675,
-0.0121750278784132));
#38237=CARTESIAN_POINT('Ctrl Pts',(0.00250015744038486,-0.0327596397129048,
-0.0126522967210052));
#38238=CARTESIAN_POINT('Ctrl Pts',(0.00235932583811129,-0.0327291801705421,
-0.0131311592784346));
#38239=CARTESIAN_POINT('Ctrl Pts',(0.00209951830117244,-0.0326987206281795,
-0.0135330647303066));
#38240=CARTESIAN_POINT('Ctrl Pts',(0.00200392607831762,-0.0326875135038754,
-0.0136809397148994));
#38241=CARTESIAN_POINT('Ctrl Pts',(0.0018927299026143,-0.0326763063795715,
-0.0138185381949725));
#38242=CARTESIAN_POINT('Ctrl Pts',(0.00176861158204399,-0.0326650992552675,
-0.0139427752066949));
#38243=CARTESIAN_POINT('Ctrl Pts',(0.00143121027214934,-0.0326346339830744,
-0.014280499164769));
#38244=CARTESIAN_POINT('Ctrl Pts',(0.000992947727101739,-0.0326041687108814,
-0.0145196020115855));
#38245=CARTESIAN_POINT('Ctrl Pts',(0.000524972426846048,-0.0325737034386883,
-0.0146201126735814));
#38246=CARTESIAN_POINT('Ctrl Pts',(0.000352908448265819,-0.0325625020442147,
-0.0146570681803854));
#38247=CARTESIAN_POINT('Ctrl Pts',(0.000177082255337662,-0.0325513006497411,
-0.0146757429836459));
#38248=CARTESIAN_POINT('Ctrl Pts',(1.56413461402208E-6,-0.0325400992552675,
-0.0146758527972546));
#38249=CARTESIAN_POINT('Ctrl Pts',(-0.000474046751108256,-0.0325097462345939,
-0.0146761503650925));
#38250=CARTESIAN_POINT('Ctrl Pts',(-0.000951423590060535,-0.0324793932139203,
-0.0145364034942133));
#38251=CARTESIAN_POINT('Ctrl Pts',(-0.00135248331656414,-0.0324490401932467,
-0.0142784204979489));
#38252=CARTESIAN_POINT('Ctrl Pts',(-0.00150197248327778,-0.0324377265472536,
-0.0141822610967693));
#38253=CARTESIAN_POINT('Ctrl Pts',(-0.00164100269364965,-0.0324264129012606,
-0.0140701896281456));
#38254=CARTESIAN_POINT('Ctrl Pts',(-0.00176639923486798,-0.0324150992552675,
-0.0139449869002396));
#38255=CARTESIAN_POINT('Ctrl Pts',(-0.00210913504099933,-0.0323841766194273,
-0.0136027808277133));
#38256=CARTESIAN_POINT('Ctrl Pts',(-0.00235017420041792,-0.0323532539835871,
-0.013157143854241));
#38257=CARTESIAN_POINT('Ctrl Pts',(-0.00244840903005507,-0.0323223313477468,
-0.0126811187826538));
#38258=CARTESIAN_POINT('Ctrl Pts',(-0.00248254059772946,-0.0323115873169204,
-0.0125157244718416));
#38259=CARTESIAN_POINT('Ctrl Pts',(-0.00249984350998278,-0.0323008432860939,
-0.012346891169886));
#38260=CARTESIAN_POINT('Ctrl Pts',(-0.00249999893936607,-0.0322900992552675,
-0.0121781561475047));
#38261=CARTESIAN_POINT('',(-0.00249999997357178,-0.0312909865556403,-0.0121755454777103));
#38262=CARTESIAN_POINT('Ctrl Pts',(-0.00249999999999967,-0.0322901250241527,
-0.0121758520066069));
#38263=CARTESIAN_POINT('Ctrl Pts',(-0.00249999975397871,-0.0322616273783385,
-0.0116953239977705));
#38264=CARTESIAN_POINT('Ctrl Pts',(-0.00235838357544941,-0.0322315631162502,
-0.0112391117930363));
#38265=CARTESIAN_POINT('Ctrl Pts',(-0.00213070189368216,-0.0322030988071068,
-0.0108681417586364));
#38266=CARTESIAN_POINT('Ctrl Pts',(-0.00204892585140747,-0.0321928753296195,
-0.0107349010825299));
#38267=CARTESIAN_POINT('Ctrl Pts',(-0.00195630643732137,-0.0321828582490487,
-0.010612003978176));
#38268=CARTESIAN_POINT('Ctrl Pts',(-0.00185518017705755,-0.0321731942832527,
-0.0105000530267859));
#38269=CARTESIAN_POINT('Ctrl Pts',(-0.00184583808252193,-0.0321723015212558,
-0.0104897109418664));
#38270=CARTESIAN_POINT('Ctrl Pts',(-0.00183642818598577,-0.0321714118294668,
-0.010479467651635));
#38271=CARTESIAN_POINT('Ctrl Pts',(-0.0018269522946202,-0.0321705251244434,
-0.0104693230895847));
#38272=CARTESIAN_POINT('Ctrl Pts',(-0.0014935199541142,-0.0321393242463525,
-0.0101123619407762));
#38273=CARTESIAN_POINT('Ctrl Pts',(-0.00107750042637275,-0.0321118214492774,
-0.00987938050070426));
#38274=CARTESIAN_POINT('Ctrl Pts',(-0.000663016412915333,-0.0320843813491235,
-0.009765374239521));
#38275=CARTESIAN_POINT('Ctrl Pts',(-0.00060675889316707,-0.0320806569305062,
-0.00974990027844722));
#38276=CARTESIAN_POINT('Ctrl Pts',(-0.00055051895230167,-0.032076933666915,
-0.00973655052044115));
#38277=CARTESIAN_POINT('Ctrl Pts',(-0.000494472428651543,-0.0320732024682493,
-0.00972524172670137));
#38278=CARTESIAN_POINT('Ctrl Pts',(-0.000166245003803277,-0.032051351305146,
-0.0096590136003947));
#38279=CARTESIAN_POINT('Ctrl Pts',(0.000155346586532059,-0.0320307859803488,
-0.00966315997919557));
#38280=CARTESIAN_POINT('Ctrl Pts',(0.000446820137915882,-0.0320118112729673,
-0.00971610700607452));
#38281=CARTESIAN_POINT('Ctrl Pts',(0.000582229204164707,-0.0320029962453373,
-0.00974070446075365));
#38282=CARTESIAN_POINT('Ctrl Pts',(0.000711629629261853,-0.0319945245091002,
-0.00977576702176651));
#38283=CARTESIAN_POINT('Ctrl Pts',(0.00083393264289702,-0.031986426622681,
-0.00981904265625477));
#38284=CARTESIAN_POINT('Ctrl Pts',(0.00121949789381606,-0.0319608977046573,
-0.00995547086333002));
#38285=CARTESIAN_POINT('Ctrl Pts',(0.00152880138072454,-0.031938621727944,
-0.0101708635989568));
#38286=CARTESIAN_POINT('Ctrl Pts',(0.00176119446046587,-0.0319172141729503,
-0.0104015381870269));
#38287=CARTESIAN_POINT('Ctrl Pts',(0.0019935875402072,-0.0318958066179567,
-0.0106322127750971));
#38288=CARTESIAN_POINT('Ctrl Pts',(0.00215013969655286,-0.0318767874994582,
-0.0108768456008528));
#38289=CARTESIAN_POINT('Ctrl Pts',(0.0022561209758157,-0.0318610351411786,
-0.0110988583271992));
#38290=CARTESIAN_POINT('Ctrl Pts',(0.00227592622398728,-0.0318580914197291,
-0.0111403469483324));
#38291=CARTESIAN_POINT('Ctrl Pts',(0.00229396174659566,-0.0318552393346794,
-0.0111810688164089));
#38292=CARTESIAN_POINT('Ctrl Pts',(0.00231042100019264,-0.031852479018487,
-0.0112208900402136));
#38293=CARTESIAN_POINT('Ctrl Pts',(0.002382038035103,-0.0318404684093821,
-0.0113941590137179));
#38294=CARTESIAN_POINT('Ctrl Pts',(0.00242408001468336,-0.0318301952319051,
-0.0115499894070535));
#38295=CARTESIAN_POINT('Ctrl Pts',(0.00245053904127961,-0.031821670397811,
-0.011681021590762));
#38296=CARTESIAN_POINT('Ctrl Pts',(0.00246680900318903,-0.0318164283785896,
-0.0117615947981735));
#38297=CARTESIAN_POINT('Ctrl Pts',(0.00247711855042881,-0.0318121280969749,
-0.0118327269911542));
#38298=CARTESIAN_POINT('Ctrl Pts',(0.00248410590563771,-0.0318084305852773,
-0.0118943966299023));
#38299=CARTESIAN_POINT('Ctrl Pts',(0.0024910932608466,-0.0318047330735796,
-0.0119560662686504));
#38300=CARTESIAN_POINT('Ctrl Pts',(0.00249470831019364,-0.0318015854479095,
-0.0120082878373164));
#38301=CARTESIAN_POINT('Ctrl Pts',(0.00249677081350409,-0.0317991659468958,
-0.0120488276795565));
#38302=CARTESIAN_POINT('Ctrl Pts',(0.00249883331681454,-0.0317967464458821,
-0.0120893675217966));
#38303=CARTESIAN_POINT('Ctrl Pts',(0.00249945501450155,-0.0317950110462313,
-0.0121182150104752));
#38304=CARTESIAN_POINT('Ctrl Pts',(0.00249977959816441,-0.0317934891261923,
-0.0121426574946412));
#38305=CARTESIAN_POINT('Ctrl Pts',(0.00249994188999584,-0.0317927281661728,
-0.0121548787367242));
#38306=CARTESIAN_POINT('Ctrl Pts',(0.00249998123728428,-0.0317920411315702,
-0.0121660007433696));
#38307=CARTESIAN_POINT('Ctrl Pts',(0.00249998704855481,-0.0317919445319498,
-0.0121678061095248));
#38308=CARTESIAN_POINT('Ctrl Pts',(0.00249999285982534,-0.0317918479323293,
-0.0121696114756799));
#38309=CARTESIAN_POINT('Ctrl Pts',(0.00250001929907833,-0.0317916697812854,
-0.0121725320504109));
#38310=CARTESIAN_POINT('Ctrl Pts',(0.00249999006451306,-0.0317910018346423,
-0.0121829015016505));
#38311=CARTESIAN_POINT('Ctrl Pts',(0.00249996082994778,-0.0317903338879991,
-0.0121932709528901));
#38312=CARTESIAN_POINT('Ctrl Pts',(0.00249956436397612,-0.0317875590268506,
-0.0122386669065317));
#38313=CARTESIAN_POINT('Ctrl Pts',(0.00249780162821883,-0.0317850627778348,
-0.01228067230233));
#38314=CARTESIAN_POINT('Ctrl Pts',(0.00249603889246154,-0.0317825665288191,
-0.0123226776981282));
#38315=CARTESIAN_POINT('Ctrl Pts',(0.00249348223220822,-0.0317801299102132,
-0.0123613011644103));
#38316=CARTESIAN_POINT('Ctrl Pts',(0.00248956162025467,-0.0317773729958845,
-0.0124040701548105));
#38317=CARTESIAN_POINT('Ctrl Pts',(0.00248172039634758,-0.0317718591672271,
-0.012489608135611));
#38318=CARTESIAN_POINT('Ctrl Pts',(0.00246784924379192,-0.0317652992968616,
-0.012591678790119));
#38319=CARTESIAN_POINT('Ctrl Pts',(0.00244358882404981,-0.0317578665642037,
-0.0127039381840688));
#38320=CARTESIAN_POINT('Ctrl Pts',(0.00239506798456559,-0.0317430010988878,
-0.0129284569719683));
#38321=CARTESIAN_POINT('Ctrl Pts',(0.00230651280877661,-0.0317242331886206,
-0.0131939916838651));
#38322=CARTESIAN_POINT('Ctrl Pts',(0.00213708827204978,-0.0317033296526518,
-0.0134731018045635));
#38323=CARTESIAN_POINT('Ctrl Pts',(0.00211106753075451,-0.0317001192233237,
-0.0135159683951052));
#38324=CARTESIAN_POINT('Ctrl Pts',(0.00208311322091434,-0.0316968275939304,
-0.0135591125370878));
#38325=CARTESIAN_POINT('Ctrl Pts',(0.00205310009985602,-0.0316934583601711,
-0.0136023104292621));
#38326=CARTESIAN_POINT('Ctrl Pts',(0.00198540349248402,-0.0316858588274699,
-0.0136997461721207));
#38327=CARTESIAN_POINT('Ctrl Pts',(0.00190718091663154,-0.0316778644761325,
-0.0137975154075378));
#38328=CARTESIAN_POINT('Ctrl Pts',(0.00181730979982462,-0.0316695165681902,
-0.0138926482922188));
#38329=CARTESIAN_POINT('Ctrl Pts',(0.00168759454882717,-0.0316574676362027,
-0.0140299581026779));
#38330=CARTESIAN_POINT('Ctrl Pts',(0.001533340118632,-0.0316455973192644,
-0.0141618818978339));
#38331=CARTESIAN_POINT('Ctrl Pts',(0.00135414966748958,-0.031632707315196,
-0.0142773476781847));
#38332=CARTESIAN_POINT('Ctrl Pts',(0.00117495921634717,-0.0316198173111276,
-0.0143928134585354));
#38333=CARTESIAN_POINT('Ctrl Pts',(0.000971210794888545,-0.0316056919371159,
-0.0144920322181475));
#38334=CARTESIAN_POINT('Ctrl Pts',(0.000741339520769619,-0.0315892324856351,
-0.0145634076241482));
#38335=CARTESIAN_POINT('Ctrl Pts',(0.000626403883710157,-0.0315810027598947,
-0.0145990953271485));
#38336=CARTESIAN_POINT('Ctrl Pts',(0.000504724124808493,-0.0315725740963865,
-0.0146274233264182));
#38337=CARTESIAN_POINT('Ctrl Pts',(0.000383936331685177,-0.0315647779266216,
-0.0146461959537223));
#38338=CARTESIAN_POINT('Ctrl Pts',(0.000320100625507402,-0.0315606576923698,
-0.0146561171873982));
#38339=CARTESIAN_POINT('Ctrl Pts',(0.000256473434805746,-0.0315565689173678,
-0.01466375980847));
#38340=CARTESIAN_POINT('Ctrl Pts',(0.000182796389150301,-0.0315518446614979,
-0.0146691614263823));
#38341=CARTESIAN_POINT('Ctrl Pts',(0.000115743617557936,-0.0315475451616066,
-0.0146740773869625));
#38342=CARTESIAN_POINT('Ctrl Pts',(4.24952442558038E-5,-0.0315428561028207,
-0.0146759101548113));
#38343=CARTESIAN_POINT('Ctrl Pts',(-3.22331663466373E-6,-0.0315399279035967,
-0.0146758512086032));
#38344=CARTESIAN_POINT('Ctrl Pts',(-4.56379105660485E-5,-0.0315372113180652,
-0.0146757965222913));
#38345=CARTESIAN_POINT('Ctrl Pts',(-6.54327116774078E-5,-0.0315359428186249,
-0.0146751074190157));
#38346=CARTESIAN_POINT('Ctrl Pts',(-8.89265215644094E-5,-0.0315344368225749,
-0.0146742712007115));
#38347=CARTESIAN_POINT('Ctrl Pts',(-0.000131230291107909,-0.0315317250738147,
-0.014672765477008));
#38348=CARTESIAN_POINT('Ctrl Pts',(-0.000192002285322905,-0.0315278261260052,
-0.0146690484249402));
#38349=CARTESIAN_POINT('Ctrl Pts',(-0.000245472305589629,-0.0315243863391031,
-0.0146637727682111));
#38350=CARTESIAN_POINT('Ctrl Pts',(-0.000294773357939573,-0.031521214746624,
-0.0146589084456003));
#38351=CARTESIAN_POINT('Ctrl Pts',(-0.0003425309527002,-0.0315181352822846,
-0.0146527679862795));
#38352=CARTESIAN_POINT('Ctrl Pts',(-0.00039125743125139,-0.0315149815570885,
-0.0146450470056678));
#38353=CARTESIAN_POINT('Ctrl Pts',(-0.000522802826387516,-0.0315064675409025,
-0.0146242029086674));
#38354=CARTESIAN_POINT('Ctrl Pts',(-0.000661229924873668,-0.0314974254324378,
-0.0145912048720715));
#38355=CARTESIAN_POINT('Ctrl Pts',(-0.00079902678801783,-0.0314888161832273,
-0.0145447256326397));
#38356=CARTESIAN_POINT('Ctrl Pts',(-0.000936823651161993,-0.0314802069340167,
-0.0144982463932078));
#38357=CARTESIAN_POINT('Ctrl Pts',(-0.00107414563365613,-0.0314711370981314,
-0.0144385815328944));
#38358=CARTESIAN_POINT('Ctrl Pts',(-0.00120897499076699,-0.0314614481142302,
-0.0143640898989243));
#38359=CARTESIAN_POINT('Ctrl Pts',(-0.00134380434787785,-0.0314517591303289,
-0.0142895982649543));
#38360=CARTESIAN_POINT('Ctrl Pts',(-0.00147605971849819,-0.0314414785072542,
-0.0142002174268997));
#38361=CARTESIAN_POINT('Ctrl Pts',(-0.00160175792260515,-0.031430573368138,
-0.0140953249736042));
#38362=CARTESIAN_POINT('Ctrl Pts',(-0.00180920400811086,-0.0314125760670816,
-0.0139222156679475));
#38363=CARTESIAN_POINT('Ctrl Pts',(-0.00199855550421331,-0.031394357005186,
-0.013706509475676));
#38364=CARTESIAN_POINT('Ctrl Pts',(-0.00214932033285382,-0.0313754212399793,
-0.0134527331191113));
#38365=CARTESIAN_POINT('Ctrl Pts',(-0.00218126194725279,-0.0313714094361917,
-0.0133989670876167));
#38366=CARTESIAN_POINT('Ctrl Pts',(-0.00221148838932676,-0.031367365462256,
-0.0133434938430907));
#38367=CARTESIAN_POINT('Ctrl Pts',(-0.00223981109177484,-0.0313632846113783,
-0.0132863695057834));
#38368=CARTESIAN_POINT('Ctrl Pts',(-0.00240181625098881,-0.0313399422450423,
-0.0129596197057801));
#38369=CARTESIAN_POINT('Ctrl Pts',(-0.00250001841270888,-0.0313177033710342,
-0.0125780611358331));
#38370=CARTESIAN_POINT('Ctrl Pts',(-0.00249999999738109,-0.031291873856013,
-0.0121757388551144));
#38371=CARTESIAN_POINT('',(-0.00249999942061914,-0.0302901454774401,-0.0121744765208516));
#38372=CARTESIAN_POINT('Ctrl Pts',(-0.00249999994976247,-0.0312900992552675,
-0.0121753521003062));
#38373=CARTESIAN_POINT('Ctrl Pts',(-0.00249990259183997,-0.0312591857748376,
-0.0116897146742599));
#38374=CARTESIAN_POINT('Ctrl Pts',(-0.00235401452783209,-0.0312282722944076,
-0.0112041304353443));
#38375=CARTESIAN_POINT('Ctrl Pts',(-0.00208666920114698,-0.0311973588139777,
-0.0107989685255906));
#38376=CARTESIAN_POINT('Ctrl Pts',(-0.00199372216379006,-0.0311866112297353,
-0.010658107267126));
#38377=CARTESIAN_POINT('Ctrl Pts',(-0.00188654303827572,-0.031175863645493,
-0.0105268207704096));
#38378=CARTESIAN_POINT('Ctrl Pts',(-0.00176745734384853,-0.0311651160612506,
-0.0104077767786898));
#38379=CARTESIAN_POINT('Ctrl Pts',(-0.00143124037051339,-0.0311347721961708,
-0.0100716775454251));
#38380=CARTESIAN_POINT('Ctrl Pts',(-0.000994786137417781,-0.031104428331091,
-0.00983322878898758));
#38381=CARTESIAN_POINT('Ctrl Pts',(-0.000528612127681506,-0.0310740844660112,
-0.00973237846195523));
#38382=CARTESIAN_POINT('Ctrl Pts',(-0.000354745538862485,-0.0310627672664187,
-0.00969476481988986));
#38383=CARTESIAN_POINT('Ctrl Pts',(-0.000177009517374391,-0.0310514500668262,
-0.00967582674646241));
#38384=CARTESIAN_POINT('Ctrl Pts',(3.7444390193485E-7,-0.0310401328672337,
-0.00967585331459975));
#38385=CARTESIAN_POINT('Ctrl Pts',(0.000477738492770387,-0.0310096767640976,
-0.00967592481302339));
#38386=CARTESIAN_POINT('Ctrl Pts',(0.000956612727593189,-0.0309792206609616,
-0.00981704046168377));
#38387=CARTESIAN_POINT('Ctrl Pts',(0.00135843499603846,-0.0309487645578255,
-0.0100771264435559));
#38388=CARTESIAN_POINT('Ctrl Pts',(0.00150626753529031,-0.0309375595962893,
-0.0101728134528218));
#38389=CARTESIAN_POINT('Ctrl Pts',(0.00164381276844332,-0.0309263546347531,
-0.0102841012708437));
#38390=CARTESIAN_POINT('Ctrl Pts',(0.00176798690091599,-0.0309151496732169,
-0.010408306308911));
#38391=CARTESIAN_POINT('Ctrl Pts',(0.00210544008061321,-0.0308846992901661,
-0.010745843477044));
#38392=CARTESIAN_POINT('Ctrl Pts',(0.00234425609545278,-0.0308542489071155,
-0.0111841501902191));
#38393=CARTESIAN_POINT('Ctrl Pts',(0.00244451688867356,-0.0308237985240648,
-0.0116520812168658));
#38394=CARTESIAN_POINT('Ctrl Pts',(0.00248142912817006,-0.0308125878424432,
-0.0118243557577763));
#38395=CARTESIAN_POINT('Ctrl Pts',(0.00250001739721303,-0.0308013771608217,
-0.0120003907020759));
#38396=CARTESIAN_POINT('Ctrl Pts',(0.00249999998772879,-0.0307901664792,
-0.0121761009881092));
#38397=CARTESIAN_POINT('Ctrl Pts',(0.00249995270019697,-0.0307597160961492,
-0.012653364164095));
#38398=CARTESIAN_POINT('Ctrl Pts',(0.00235891876369913,-0.0307292657130982,
-0.0131321617656519));
#38399=CARTESIAN_POINT('Ctrl Pts',(0.00209894355269856,-0.0306988153300473,
-0.0135339534163663));
#38400=CARTESIAN_POINT('Ctrl Pts',(0.00200323049335481,-0.0306876046484259,
-0.0136818779356336));
#38401=CARTESIAN_POINT('Ctrl Pts',(0.00189189875249167,-0.0306763939668046,
-0.0138195067532682));
#38402=CARTESIAN_POINT('Ctrl Pts',(0.0017676366069028,-0.0306651832851831,
-0.0139437505759777));
#38403=CARTESIAN_POINT('Ctrl Pts',(0.00143005314411421,-0.0306347271820469,
-0.0142812842609272));
#38404=CARTESIAN_POINT('Ctrl Pts',(0.0009916643058973,-0.0306042710789107,
-0.0145201443823691));
#38405=CARTESIAN_POINT('Ctrl Pts',(0.000523638769525182,-0.0305738149757745,
-0.014620398732863));
#38406=CARTESIAN_POINT('Ctrl Pts',(0.0003514496976169,-0.0305626100142384,
-0.014657282839017));
#38407=CARTESIAN_POINT('Ctrl Pts',(0.000175503802646239,-0.0305514050527023,
-0.0146758617810041));
#38408=CARTESIAN_POINT('Ctrl Pts',(-1.20959199542376E-7,-0.0305402000911662,
-0.0146758532836319));
#38409=CARTESIAN_POINT('Ctrl Pts',(-0.000475725811651964,-0.0305098562260865,
-0.0146758302721189));
#38410=CARTESIAN_POINT('Ctrl Pts',(-0.000953003524480613,-0.0304795123610067,
-0.0145357650987292));
#38411=CARTESIAN_POINT('Ctrl Pts',(-0.00135388681630664,-0.030449168495927,
-0.0142775170295558));
#38412=CARTESIAN_POINT('Ctrl Pts',(-0.00150340225262242,-0.0304378512963344,
-0.014181199538836));
#38413=CARTESIAN_POINT('Ctrl Pts',(-0.00164243535305725,-0.0304265340967419,
-0.0140689576145839));
#38414=CARTESIAN_POINT('Ctrl Pts',(-0.0017678076733794,-0.0304152168971493,
-0.0139435795181734));
#38415=CARTESIAN_POINT('Ctrl Pts',(-0.00211026825641089,-0.0303843034167193,
-0.013601103157476));
#38416=CARTESIAN_POINT('Ctrl Pts',(-0.00235095201767094,-0.0303533899362893,
-0.0131552776793517));
#38417=CARTESIAN_POINT('Ctrl Pts',(-0.00244880888004733,-0.0303224764558593,
-0.0126791773064512));
#38418=CARTESIAN_POINT('Ctrl Pts',(-0.00248283044143243,-0.030311728871617,
-0.0125136531145984));
#38419=CARTESIAN_POINT('Ctrl Pts',(-0.00249999960942255,-0.0303009812873747,
-0.0123446989796761));
#38420=CARTESIAN_POINT('Ctrl Pts',(-0.00249999999999331,-0.0302902337031324,
-0.0121758590697104));
#38421=CARTESIAN_POINT('',(-0.00249999943912681,-0.0292900991654731,-0.0121775325936968));
#38422=CARTESIAN_POINT('Ctrl Pts',(-0.0024999991170802,-0.0302900992552675,
-0.0121737521920283));
#38423=CARTESIAN_POINT('Ctrl Pts',(-0.00249959096584859,-0.0302591749334474,
-0.0116881111586653));
#38424=CARTESIAN_POINT('Ctrl Pts',(-0.00235339003378415,-0.0302282506116274,
-0.0112026172509638));
#38425=CARTESIAN_POINT('Ctrl Pts',(-0.00199282144836561,-0.0301865839449607,
-0.0106569403810191));
#38426=CARTESIAN_POINT('Ctrl Pts',(-0.00188565876843709,-0.0301758416001141,
-0.0105258239057141));
#38427=CARTESIAN_POINT('Ctrl Pts',(-0.00143023212870617,-0.0301347445227216,
-0.0100709902258644));
#38428=CARTESIAN_POINT('Ctrl Pts',(-0.00099365647799636,-0.0301043897901757,
-0.00983274807457304));
#38429=CARTESIAN_POINT('Ctrl Pts',(-0.000353683170743005,-0.030062723123509,
-0.00969462347352273));
#38430=CARTESIAN_POINT('Ctrl Pts',(-0.000176084995757376,-0.0300514111893883,
-0.00967577159798382));
#38431=CARTESIAN_POINT('Ctrl Pts',(0.000478527791617883,-0.0300096322717532,
-0.00967607428947804));
#38432=CARTESIAN_POINT('Ctrl Pts',(0.00095736400795089,-0.029979165288239,
-0.00981734402679618));
#38433=CARTESIAN_POINT('Ctrl Pts',(0.00150678939658889,-0.0299374986215723,
-0.0101732186109999));
#38434=CARTESIAN_POINT('Ctrl Pts',(0.00164419531455132,-0.0299262989384199,
-0.0102844469810999));
#38435=CARTESIAN_POINT('Ctrl Pts',(0.00210565841324517,-0.0298846380046097,
-0.0107461624561916));
#38436=CARTESIAN_POINT('Ctrl Pts',(0.00234441033443847,-0.029854176753952,
-0.0111845119625509));
#38437=CARTESIAN_POINT('Ctrl Pts',(0.00248145420869358,-0.0298125100872853,
-0.0118246047362775));
#38438=CARTESIAN_POINT('Ctrl Pts',(0.00250001480158532,-0.0298013046712764,
-0.0120004962840195));
#38439=CARTESIAN_POINT('Ctrl Pts',(0.00249995972970253,-0.0297596380046098,
-0.0126533349660584));
#38440=CARTESIAN_POINT('Ctrl Pts',(0.00235892856150225,-0.029729176753952,
-0.0131321406088429));
#38441=CARTESIAN_POINT('Ctrl Pts',(0.00200331865873349,-0.0296875100872853,
-0.0136817438883177));
#38442=CARTESIAN_POINT('Ctrl Pts',(0.00189209125366563,-0.0296763046712764,
-0.0138192699312786));
#38443=CARTESIAN_POINT('Ctrl Pts',(0.00143042324015757,-0.0296346322717532,
-0.0142810345935773));
#38444=CARTESIAN_POINT('Ctrl Pts',(0.000992069613805846,-0.029604165288239,
-0.0145199741564081));
#38445=CARTESIAN_POINT('Ctrl Pts',(0.000352012654775048,-0.0295624986215723,
-0.014657192859098));
#38446=CARTESIAN_POINT('Ctrl Pts',(0.000176216403953808,-0.0295512989384199,
-0.0146758016426758));
#38447=CARTESIAN_POINT('Ctrl Pts',(-0.000474878817339744,-0.0295097445227216,
-0.0146759928580223));
#38448=CARTESIAN_POINT('Ctrl Pts',(-0.000952210864759681,-0.0294793897901757,
-0.0145360863615342));
#38449=CARTESIAN_POINT('Ctrl Pts',(-0.00150261225706842,-0.029437723123509,
-0.014181778794066));
#38450=CARTESIAN_POINT('Ctrl Pts',(-0.00164157878599002,-0.0294264111893883,
-0.0140696870542259));
#38451=CARTESIAN_POINT('Ctrl Pts',(-0.00210955062163189,-0.0293841749334474,
-0.0136021667831768));
#38452=CARTESIAN_POINT('Ctrl Pts',(-0.00235046036159436,-0.0293532506116274,
-0.0131564586379207));
#38453=CARTESIAN_POINT('Ctrl Pts',(-0.00248263255009951,-0.0293115839449607,
-0.012515034510425));
#38454=CARTESIAN_POINT('Ctrl Pts',(-0.00249988611653098,-0.0293008416001141,
-0.0123462323031989));
#38455=CARTESIAN_POINT('Ctrl Pts',(-0.00249999943598566,-0.0292900992552675,
-0.0121775325933754));
#38456=CARTESIAN_POINT('',(-0.00249382779728175,-0.0292787744408383,-0.0120002887186913));
#38457=CARTESIAN_POINT('Origin',(1.04421208127001E-5,-0.0292843824914073,
-0.012176220437913));
#38458=CARTESIAN_POINT('',(0.000565648716052718,-0.0292787743898723,-0.0146110209460896));
#38459=CARTESIAN_POINT('Origin',(0.,-0.0292787743898623,-0.0121758532865581));
#38460=CARTESIAN_POINT('',(-0.00249999998652498,-0.0299924495244571,-0.0121755937194362));
#38461=CARTESIAN_POINT('Ctrl Pts',(0.000565648716059988,-0.0292787743898623,
-0.0146110209460879));
#38462=CARTESIAN_POINT('Ctrl Pts',(0.0010206242086387,-0.0293085108538038,
-0.0145053377492005));
#38463=CARTESIAN_POINT('Ctrl Pts',(0.0014447229436206,-0.0293382473177453,
-0.0142688517650026));
#38464=CARTESIAN_POINT('Ctrl Pts',(0.00177366822203208,-0.0293679837816867,
-0.0139376992043822));
#38465=CARTESIAN_POINT('Ctrl Pts',(0.00210261350044357,-0.0293977202456281,
-0.0136065466437619));
#38466=CARTESIAN_POINT('Ctrl Pts',(0.00233631458587225,-0.0294274567095696,
-0.0131806244778636));
#38467=CARTESIAN_POINT('Ctrl Pts',(0.00243889607330461,-0.029457193173511,
-0.0127252037608633));
#38468=CARTESIAN_POINT('Ctrl Pts',(0.00254147756073697,-0.0294869296374525,
-0.012269783043863));
#38469=CARTESIAN_POINT('Ctrl Pts',(0.00251297505440625,-0.0295166661013939,
-0.0117848538514163));
#38470=CARTESIAN_POINT('Ctrl Pts',(0.00235775410251832,-0.0295464025653354,
-0.0113445918402862));
#38471=CARTESIAN_POINT('Ctrl Pts',(0.00220253315063038,-0.0295761390292768,
-0.0109043298291561));
#38472=CARTESIAN_POINT('Ctrl Pts',(0.00192059182778953,-0.0296058754932183,
-0.0105087453803813));
#38473=CARTESIAN_POINT('Ctrl Pts',(0.00155507400256916,-0.0296356119571598,
-0.0102183689707758));
#38474=CARTESIAN_POINT('Ctrl Pts',(0.00118955617734879,-0.0296653484211012,
-0.0099279925611704));
#38475=CARTESIAN_POINT('Ctrl Pts',(0.000740457719301776,-0.0296950848850426,
-0.0097428209094049));
#38476=CARTESIAN_POINT('Ctrl Pts',(0.000276498140069873,-0.029724821348984,
-0.00969119057734828));
#38477=CARTESIAN_POINT('Ctrl Pts',(-0.000187461439162031,-0.0297545578129255,
-0.00963956024529165));
#38478=CARTESIAN_POINT('Ctrl Pts',(-0.000666272462951498,-0.029784294276867,
-0.00972146700967555));
#38479=CARTESIAN_POINT('Ctrl Pts',(-0.00108669381979509,-0.0298140307408084,
-0.00992438786554468));
#38480=CARTESIAN_POINT('Ctrl Pts',(-0.00150711517663868,-0.0298437672047499,
-0.0101273087214138));
#38481=CARTESIAN_POINT('Ctrl Pts',(-0.00186914848155188,-0.0298735036686913,
-0.0104512805949887));
#38482=CARTESIAN_POINT('Ctrl Pts',(-0.00211732733988455,-0.0299032401326328,
-0.0108465959992817));
#38483=CARTESIAN_POINT('Ctrl Pts',(-0.00236550619821721,-0.0299329765965742,
-0.0112419114035747));
#38484=CARTESIAN_POINT('Ctrl Pts',(-0.00249995149020126,-0.0299627130605157,
-0.0117085052539399));
#38485=CARTESIAN_POINT('Ctrl Pts',(-0.00249999998652498,-0.0299924495244571,
-0.0121755937194362));
#38486=CARTESIAN_POINT('',(-0.00249999945595836,-0.0309923794005721,-0.012177043828097));
#38487=CARTESIAN_POINT('Ctrl Pts',(-0.00249999999999978,-0.029992465890772,
-0.012175852244816));
#38488=CARTESIAN_POINT('Ctrl Pts',(-0.00250000020236312,-0.0300233774710986,
-0.0126614890819379));
#38489=CARTESIAN_POINT('Ctrl Pts',(-0.00235421003106896,-0.0300542890514251,
-0.0131471021162331));
#38490=CARTESIAN_POINT('Ctrl Pts',(-0.00208694667699899,-0.0300852006317517,
-0.0135523174406002));
#38491=CARTESIAN_POINT('Ctrl Pts',(-0.00199401628883952,-0.0300959489259515,
-0.0136932152360075));
#38492=CARTESIAN_POINT('Ctrl Pts',(-0.00188684827597316,-0.0301066972201514,
-0.0138245387021237));
#38493=CARTESIAN_POINT('Ctrl Pts',(-0.00176776854431825,-0.0301174455143512,
-0.0139436186481712));
#38494=CARTESIAN_POINT('Ctrl Pts',(-0.00143161166736268,-0.0301477874790213,
-0.0142797761303475));
#38495=CARTESIAN_POINT('Ctrl Pts',(-0.000995200662721201,-0.0301781294436916,
-0.0145183015038843));
#38496=CARTESIAN_POINT('Ctrl Pts',(-0.000529045559956314,-0.0302084714083617,
-0.0146192343038148));
#38497=CARTESIAN_POINT('Ctrl Pts',(-0.000355163394862593,-0.0302197893720153,
-0.0146568836048238));
#38498=CARTESIAN_POINT('Ctrl Pts',(-0.000177407490434834,-0.030231107335669,
-0.0146758532210078));
#38499=CARTESIAN_POINT('Ctrl Pts',(-9.23727244943536E-10,-0.0302424252993226,
-0.0146758532865579));
#38500=CARTESIAN_POINT('Ctrl Pts',(0.000477361897951327,-0.0302728794993312,
-0.0146758534629391));
#38501=CARTESIAN_POINT('Ctrl Pts',(0.000956256347303985,-0.0303033336993398,
-0.0145348104111621));
#38502=CARTESIAN_POINT('Ctrl Pts',(0.00135811717461238,-0.0303337878993484,
-0.0142747858104909));
#38503=CARTESIAN_POINT('Ctrl Pts',(0.0015059832571254,-0.0303449936276636,
-0.0141791088585576));
#38504=CARTESIAN_POINT('Ctrl Pts',(0.00164356173072387,-0.0303561993559788,
-0.0140678255018165));
#38505=CARTESIAN_POINT('Ctrl Pts',(0.00176776723797135,-0.030367405084294,
-0.0139436199545194));
#38506=CARTESIAN_POINT('Ctrl Pts',(0.00210526151255424,-0.0303978535662714,
-0.0136061255711127));
#38507=CARTESIAN_POINT('Ctrl Pts',(0.00234413180385817,-0.0304283020482487,
-0.0131678496812006));
#38508=CARTESIAN_POINT('Ctrl Pts',(0.00244445112861001,-0.0304587505302261,
-0.0126999321735945));
#38509=CARTESIAN_POINT('Ctrl Pts',(0.00248138974275191,-0.0304699619765725,
-0.0125276401021869));
#38510=CARTESIAN_POINT('Ctrl Pts',(0.00250000012159547,-0.0304811734229191,
-0.0123515843578053));
#38511=CARTESIAN_POINT('Ctrl Pts',(0.0024999999999994,-0.0304923848692655,
-0.012175851556715));
#38512=CARTESIAN_POINT('Ctrl Pts',(0.00249999966976407,-0.0305228333512428,
-0.0116985895816349));
#38513=CARTESIAN_POINT('Ctrl Pts',(0.00235901351912043,-0.03055328183322,
-0.0112197790495299));
#38514=CARTESIAN_POINT('Ctrl Pts',(0.00209907885972606,-0.0305837303151973,
-0.0108179622965846));
#38515=CARTESIAN_POINT('Ctrl Pts',(0.00200336822661217,-0.0305949417615438,
-0.01067000920749));
#38516=CARTESIAN_POINT('Ctrl Pts',(0.00189203385010139,-0.0306061532078904,
-0.0105323529268543));
#38517=CARTESIAN_POINT('Ctrl Pts',(0.00176776479160246,-0.0306173646542369,
-0.0104080841722305));
#38518=CARTESIAN_POINT('Ctrl Pts',(0.00143020667060413,-0.0306478188542455,
-0.0100705268766629));
#38519=CARTESIAN_POINT('Ctrl Pts',(0.000991836324402045,-0.0306782730542541,
-0.00983163516427871));
#38520=CARTESIAN_POINT('Ctrl Pts',(0.000523819145203904,-0.0307087272542627,
-0.00973134648494804));
#38521=CARTESIAN_POINT('Ctrl Pts',(0.000351610604002277,-0.0307199329825779,
-0.00969444491822315));
#38522=CARTESIAN_POINT('Ctrl Pts',(0.000175642919289985,-0.0307311387108931,
-0.00967585297858804));
#38523=CARTESIAN_POINT('Ctrl Pts',(-4.38341345831789E-9,-0.0307423444392083,
-0.00967585328656194));
#38524=CARTESIAN_POINT('Ctrl Pts',(-0.000475607941086921,-0.0307726864038785,
-0.00967585412046876));
#38525=CARTESIAN_POINT('Ctrl Pts',(-0.000952891164814528,-0.0308030283685486,
-0.00981589631166478));
#38526=CARTESIAN_POINT('Ctrl Pts',(-0.00135378597959753,-0.0308333703332188,
-0.0100741245882135));
#38527=CARTESIAN_POINT('Ctrl Pts',(-0.00150332517364712,-0.0308446882968725,
-0.0101704472317898));
#38528=CARTESIAN_POINT('Ctrl Pts',(-0.0016423800975229,-0.0308560062605261,
-0.0102826989053507));
#38529=CARTESIAN_POINT('Ctrl Pts',(-0.00176777099068193,-0.0308673242241798,
-0.0104080903713165));
#38530=CARTESIAN_POINT('Ctrl Pts',(-0.0021102381370025,-0.0308982358048934,
-0.010750559082085));
#38531=CARTESIAN_POINT('Ctrl Pts',(-0.002350931064765,-0.0309291473856069,
-0.0111963788623779));
#38532=CARTESIAN_POINT('Ctrl Pts',(-0.00244879805764301,-0.0309600589663204,
-0.0116724766155812));
#38533=CARTESIAN_POINT('Ctrl Pts',(-0.00248282764897228,-0.0309708073139307,
-0.0118380218264623));
#38534=CARTESIAN_POINT('Ctrl Pts',(-0.00250000047530196,-0.030981555661541,
-0.0120069982515906));
#38535=CARTESIAN_POINT('Ctrl Pts',(-0.0024999999999901,-0.0309923040091512,
-0.0121758603235419));
#38536=CARTESIAN_POINT('',(-0.00249989090829521,-0.0319922844637892,-0.0121752665328745));
#38537=CARTESIAN_POINT('Ctrl Pts',(-0.00249999894993767,-0.0309924495244571,
-0.0121781446421717));
#38538=CARTESIAN_POINT('Ctrl Pts',(-0.00249955383980213,-0.0310233727917168,
-0.0126637850485941));
#38539=CARTESIAN_POINT('Ctrl Pts',(-0.00235331629776196,-0.0310542960589767,
-0.0131492673344889));
#38540=CARTESIAN_POINT('Ctrl Pts',(-0.00208567790527778,-0.0310852193262364,
-0.0135542391815222));
#38541=CARTESIAN_POINT('Ctrl Pts',(-0.0019926946469783,-0.0310959627256433,
-0.0136949349968991));
#38542=CARTESIAN_POINT('Ctrl Pts',(-0.00188550614587116,-0.0311067061250502,
-0.0138260593105748));
#38543=CARTESIAN_POINT('Ctrl Pts',(-0.00176643472427443,-0.0311174495244571,
-0.0139449514649749));
#38544=CARTESIAN_POINT('Ctrl Pts',(-0.00143001851901507,-0.0311478031862475,
-0.0142808611810261));
#38545=CARTESIAN_POINT('Ctrl Pts',(-0.000993419834120211,-0.031178156848038,
-0.0145190586297705));
#38546=CARTESIAN_POINT('Ctrl Pts',(-0.000527181479049827,-0.0312085105098284,
-0.0146196371739235));
#38547=CARTESIAN_POINT('Ctrl Pts',(-0.000353411446926351,-0.0312198235147046,
-0.0146571234438932));
#38548=CARTESIAN_POINT('Ctrl Pts',(-0.000175788189397624,-0.0312311365195809,
-0.0146759574606499));
#38549=CARTESIAN_POINT('Ctrl Pts',(1.47533730703213E-6,-0.0312424495244571,
-0.014675852851234));
#38550=CARTESIAN_POINT('Ctrl Pts',(0.000478845873260156,-0.0312729154375606,
-0.0146755711381606));
#38551=CARTESIAN_POINT('Ctrl Pts',(0.000957663075037329,-0.0313033813506641,
-0.0145342409292666));
#38552=CARTESIAN_POINT('Ctrl Pts',(0.00135937336850242,-0.0313338472637676,
-0.0142739724550055));
#38553=CARTESIAN_POINT('Ctrl Pts',(0.00150706163852454,-0.0313450480173308,
-0.0141782850869439));
#38554=CARTESIAN_POINT('Ctrl Pts',(0.0016444698318857,-0.0313562487708939,
-0.0140670230067143));
#38555=CARTESIAN_POINT('Ctrl Pts',(0.00176852150679043,-0.0313674495244571,
-0.013942865363489));
#38556=CARTESIAN_POINT('Ctrl Pts',(0.00210587707764771,-0.0313979097065968,
-0.0136052216143116));
#38557=CARTESIAN_POINT('Ctrl Pts',(0.00234456149770483,-0.0314283698887366,
-0.0131668365917466));
#38558=CARTESIAN_POINT('Ctrl Pts',(0.00244467869100603,-0.0314588300708764,
-0.0126988696321354));
#38559=CARTESIAN_POINT('Ctrl Pts',(0.00248151240961152,-0.0314700365554033,
-0.0125267017682688));
#38560=CARTESIAN_POINT('Ctrl Pts',(0.00250004622107205,-0.0314812430399301,
-0.0123507843182147));
#38561=CARTESIAN_POINT('Ctrl Pts',(0.00249999991305973,-0.0314924495244571,
-0.0121751939677149));
#38562=CARTESIAN_POINT('Ctrl Pts',(0.00249987404392688,-0.0315229097065968,
-0.0116979243971061));
#38563=CARTESIAN_POINT('Ctrl Pts',(0.00235875767002164,-0.0315533698887364,
-0.0112191449994495));
#38564=CARTESIAN_POINT('Ctrl Pts',(0.00209871088251693,-0.0315838300708761,
-0.0108173936325363));
#38565=CARTESIAN_POINT('Ctrl Pts',(0.00200303810265292,-0.0315950365554031,
-0.0106695868841601));
#38566=CARTESIAN_POINT('Ctrl Pts',(0.00189176989217815,-0.0316062430399301,
-0.0105320643269465));
#38567=CARTESIAN_POINT('Ctrl Pts',(0.00176758924132678,-0.0316174495244571,
-0.0104079086398155));
#38568=CARTESIAN_POINT('Ctrl Pts',(0.00142999211986863,-0.0316479154375606,
-0.010070379384648));
#38569=CARTESIAN_POINT('Ctrl Pts',(0.000991590643801229,-0.0316783813506642,
-0.00983152996620587));
#38570=CARTESIAN_POINT('Ctrl Pts',(0.000523556634283034,-0.0317088472637678,
-0.00973129024775173));
#38571=CARTESIAN_POINT('Ctrl Pts',(0.00035148453580507,-0.0317200480173309,
-0.00969443724486205));
#38572=CARTESIAN_POINT('Ctrl Pts',(0.000175661390257492,-0.031731248770894,
-0.00967586429208138));
#38573=CARTESIAN_POINT('Ctrl Pts',(1.56699690761575E-7,-0.0317424495244571,
-0.00967585329146906));
#38574=CARTESIAN_POINT('Ctrl Pts',(-0.00047545505179257,-0.0317728031862475,
-0.00967582348018325));
#38575=CARTESIAN_POINT('Ctrl Pts',(-0.0009527537503948,-0.0318031568480379,
-0.00981583951346853));
#38576=CARTESIAN_POINT('Ctrl Pts',(-0.00135366848554465,-0.0318335105098283,
-0.0100740489114453));
#38577=CARTESIAN_POINT('Ctrl Pts',(-0.00150309198459525,-0.0318448235147045,
-0.0101702852139574));
#38578=CARTESIAN_POINT('Ctrl Pts',(-0.00164204916855227,-0.0318561365195809,
-0.0102824252413429));
#38579=CARTESIAN_POINT('Ctrl Pts',(-0.0017673675983348,-0.0318674495244571,
-0.0104076870691576));
#38580=CARTESIAN_POINT('Ctrl Pts',(-0.0021099163145363,-0.031898372791717,
-0.0107500810680407));
#38581=CARTESIAN_POINT('Ctrl Pts',(-0.00235071149540477,-0.0319292960589769,
-0.0111958503674165));
#38582=CARTESIAN_POINT('Ctrl Pts',(-0.00244868552940724,-0.0319602193262366,
-0.0116719295045517));
#38583=CARTESIAN_POINT('Ctrl Pts',(-0.00248272378836424,-0.0319709627256435,
-0.0118373295017941));
#38584=CARTESIAN_POINT('Ctrl Pts',(-0.00249993416323528,-0.0319817061250503,
-0.0120061587251184));
#38585=CARTESIAN_POINT('Ctrl Pts',(-0.00249999981076385,-0.0319924495244571,
-0.01217488056835));
#38586=CARTESIAN_POINT('',(-0.00249999968239255,-0.0329925058241451,-0.0121749586412689));
#38587=CARTESIAN_POINT('Ctrl Pts',(-0.00249999999995083,-0.0319925127996754,
-0.0121758689662745));
#38588=CARTESIAN_POINT('Ctrl Pts',(-0.0024999969540786,-0.0320234311161074,
-0.0126615078884318));
#38589=CARTESIAN_POINT('Ctrl Pts',(-0.0023542023509467,-0.0320543494325394,
-0.0131471216855443));
#38590=CARTESIAN_POINT('Ctrl Pts',(-0.0020869343037223,-0.0320852677489715,
-0.0135523362003449));
#38591=CARTESIAN_POINT('Ctrl Pts',(-0.00199404483670037,-0.0320960134627387,
-0.0136931691981547));
#38592=CARTESIAN_POINT('Ctrl Pts',(-0.0018869307868893,-0.0321067591765059,
-0.0138244364875498));
#38593=CARTESIAN_POINT('Ctrl Pts',(-0.00176791476587925,-0.0321175048902731,
-0.0139434724142511));
#38594=CARTESIAN_POINT('Ctrl Pts',(-0.00143178245151699,-0.0321478535912915,
-0.0142796609474821));
#38595=CARTESIAN_POINT('Ctrl Pts',(-0.000995386817022444,-0.03217820229231,
-0.0145182231418634));
#38596=CARTESIAN_POINT('Ctrl Pts',(-0.000529236055691413,-0.0322085509933284,
-0.0146191930495375));
#38597=CARTESIAN_POINT('Ctrl Pts',(-0.00035543457044395,-0.0322198663225092,
-0.0146568390674673));
#38598=CARTESIAN_POINT('Ctrl Pts',(-0.000177761363019128,-0.03223118165169,
-0.0146758224807982));
#38599=CARTESIAN_POINT('Ctrl Pts',(-4.33775247199217E-7,-0.0322424969808708,
-0.0146758532489259));
#38600=CARTESIAN_POINT('Ctrl Pts',(0.000476933345555184,-0.0322729579270768,
-0.0146759360769435));
#38601=CARTESIAN_POINT('Ctrl Pts',(0.000955855591101025,-0.0323034188732828,
-0.0145349735201245));
#38602=CARTESIAN_POINT('Ctrl Pts',(0.00135776313800081,-0.0323338798194889,
-0.0142750148480121));
#38603=CARTESIAN_POINT('Ctrl Pts',(0.0015055787696942,-0.0323450829034821,
-0.0141794059060332));
#38604=CARTESIAN_POINT('Ctrl Pts',(0.00164311873360453,-0.0323562859874753,
-0.0140682029338377));
#38605=CARTESIAN_POINT('Ctrl Pts',(0.00176730125990038,-0.0323674890714685,
-0.0139440858099426));
#38606=CARTESIAN_POINT('Ctrl Pts',(0.00210488743550194,-0.0323979442924487,
-0.0136066774286491));
#38607=CARTESIAN_POINT('Ctrl Pts',(0.00234387389339254,-0.0324283995134288,
-0.0131684605187964));
#38608=CARTESIAN_POINT('Ctrl Pts',(0.00244431520109232,-0.0324588547344089,
-0.0127005657770793));
#38609=CARTESIAN_POINT('Ctrl Pts',(0.00248128184981438,-0.0324700635436281,
-0.0125283607256711));
#38610=CARTESIAN_POINT('Ctrl Pts',(0.00249993778676581,-0.0324812723528472,
-0.0123523906424397));
#38611=CARTESIAN_POINT('Ctrl Pts',(0.00249999984398088,-0.0324924811620663,
-0.0121767365167549));
#38612=CARTESIAN_POINT('Ctrl Pts',(0.00250016845834137,-0.0325229363830465,
-0.0116994703674921));
#38613=CARTESIAN_POINT('Ctrl Pts',(0.0023593494439565,-0.0325533916040268,
-0.0112206066619966));
#38614=CARTESIAN_POINT('Ctrl Pts',(0.0020995534792578,-0.0325838468250071,
-0.0108186962625788));
#38615=CARTESIAN_POINT('Ctrl Pts',(0.00200393757792991,-0.032595055634226,
-0.0106707762395023));
#38616=CARTESIAN_POINT('Ctrl Pts',(0.00189270843726949,-0.032606264443445,
-0.0105331382635439));
#38617=CARTESIAN_POINT('Ctrl Pts',(0.00176855022373763,-0.032617473252664,
-0.0104088699515723));
#38618=CARTESIAN_POINT('Ctrl Pts',(0.00143113912238476,-0.03264793419887,
-0.0100711596478167));
#38619=CARTESIAN_POINT('Ctrl Pts',(0.000992870892482344,-0.032678395145076,
-0.00983207245885684));
#38620=CARTESIAN_POINT('Ctrl Pts',(0.000524894531450418,-0.0327088560912821,
-0.00973157717063882));
#38621=CARTESIAN_POINT('Ctrl Pts',(0.000352779770338811,-0.0327200591752753,
-0.00969461649491933));
#38622=CARTESIAN_POINT('Ctrl Pts',(0.000176901206017232,-0.0327312622592685,
-0.00967594723280333));
#38623=CARTESIAN_POINT('Ctrl Pts',(1.33268511776818E-6,-0.0327424653432617,
-0.00967585364176805));
#38624=CARTESIAN_POINT('Ctrl Pts',(-0.000474275330698369,-0.0327728140442801,
-0.0096756001074422));
#38625=CARTESIAN_POINT('Ctrl Pts',(-0.000951636949235143,-0.0328031627452987,
-0.00981538955061219));
#38626=CARTESIAN_POINT('Ctrl Pts',(-0.00135267162894355,-0.0328335114463172,
-0.0100734072196515));
#38627=CARTESIAN_POINT('Ctrl Pts',(-0.00150219497793399,-0.0328448267754979,
-0.0101696075432781));
#38628=CARTESIAN_POINT('Ctrl Pts',(-0.00164125192130111,-0.0328561421046787,
-0.010281728147083));
#38629=CARTESIAN_POINT('Ctrl Pts',(-0.0017666653529596,-0.0328674574338594,
-0.0104069854196296));
#38630=CARTESIAN_POINT('Ctrl Pts',(-0.0021093484603536,-0.0328983757502914,
-0.0107492418335746));
#38631=CARTESIAN_POINT('Ctrl Pts',(-0.00235032038741192,-0.0329292940667234,
-0.0111949134906389));
#38632=CARTESIAN_POINT('Ctrl Pts',(-0.00244848416552665,-0.0329602123831554,
-0.011670952017828));
#38633=CARTESIAN_POINT('Ctrl Pts',(-0.00248260115453699,-0.0329709580969226,
-0.011836400022301));
#38634=CARTESIAN_POINT('Ctrl Pts',(-0.00249987904565359,-0.0329817038106899,
-0.012005286551277));
#38635=CARTESIAN_POINT('Ctrl Pts',(-0.00249999936479533,-0.0329924495244571,
-0.0121740711465624));
#38636=CARTESIAN_POINT('',(-0.00249999969181303,-0.0339923940613826,-0.0121767345639794));
#38637=CARTESIAN_POINT('Ctrl Pts',(-0.00249999999998977,-0.0329925621238332,
-0.0121758461359755));
#38638=CARTESIAN_POINT('Ctrl Pts',(-0.00250000139097379,-0.0330234456018171,
-0.0126621645583693));
#38639=CARTESIAN_POINT('Ctrl Pts',(-0.00235381656149027,-0.0330543454390897,
-0.0131484007170305));
#38640=CARTESIAN_POINT('Ctrl Pts',(-0.00208584926554848,-0.0330852540039819,
-0.0135539798560033));
#38641=CARTESIAN_POINT('Ctrl Pts',(-0.00199318331240229,-0.0330959425158619,
-0.0136942334543279));
#38642=CARTESIAN_POINT('Ctrl Pts',(-0.0018863982675443,-0.0331066320714345,
-0.0138249865451629));
#38643=CARTESIAN_POINT('Ctrl Pts',(-0.0017677846850215,-0.0331173223551014,
-0.0139436025072915));
#38644=CARTESIAN_POINT('Ctrl Pts',(-0.00143207666897764,-0.0331475787038638,
-0.0142793172582532));
#38645=CARTESIAN_POINT('Ctrl Pts',(-0.000996371926244987,-0.0331778408849578,
-0.0145176499124597));
#38646=CARTESIAN_POINT('Ctrl Pts',(-0.000531036937658981,-0.0332081303637266,
-0.0146188022771925));
#38647=CARTESIAN_POINT('Ctrl Pts',(-0.000356506957828496,-0.0332194908293014,
-0.0146567407959149));
#38648=CARTESIAN_POINT('Ctrl Pts',(-0.000178075723610798,-0.0332308551349036,
-0.0146758516231808));
#38649=CARTESIAN_POINT('Ctrl Pts',(-2.33536370774718E-8,-0.033242224413066,
-0.014675853286449));
#38650=CARTESIAN_POINT('Ctrl Pts',(0.000473652017079301,-0.0332724702730293,
-0.0146758577112661));
#38651=CARTESIAN_POINT('Ctrl Pts',(0.000949299429672487,-0.0333027513251704,
-0.0145369128632183));
#38652=CARTESIAN_POINT('Ctrl Pts',(0.00134930500747653,-0.0333329893848579,
-0.0142804615628886));
#38653=CARTESIAN_POINT('Ctrl Pts',(0.00150055285081224,-0.0333444228287101,
-0.0141834936498199));
#38654=CARTESIAN_POINT('Ctrl Pts',(0.00164113036191268,-0.0333558501259118,
-0.0140702546393804));
#38655=CARTESIAN_POINT('Ctrl Pts',(0.00176775165797444,-0.0333672670498662,
-0.0139436355343841));
#38656=CARTESIAN_POINT('Ctrl Pts',(0.00212865259841615,-0.0333998080103543,
-0.0135827408390023));
#38657=CARTESIAN_POINT('Ctrl Pts',(0.00237540286991301,-0.0334322647000166,
-0.0131089574530919));
#38658=CARTESIAN_POINT('Ctrl Pts',(0.00246315794142062,-0.033465001894446,
-0.0126034663775838));
#38659=CARTESIAN_POINT('Ctrl Pts',(0.00248761842763343,-0.03347412692482,
-0.0124625678828216));
#38660=CARTESIAN_POINT('Ctrl Pts',(0.00249999885738162,-0.0334832737486432,
-0.0123193577753516));
#38661=CARTESIAN_POINT('Ctrl Pts',(0.00249999999992074,-0.0334924502655019,
-0.0121758731935598));
#38662=CARTESIAN_POINT('Ctrl Pts',(0.00250000351370605,-0.0335206718899671,
-0.0117345981383053));
#38663=CARTESIAN_POINT('Ctrl Pts',(0.00237875224282036,-0.0335491743569653,
-0.011286396448637));
#38664=CARTESIAN_POINT('Ctrl Pts',(0.0021511060277031,-0.0335776294465269,
-0.0109019840399007));
#38665=CARTESIAN_POINT('Ctrl Pts',(0.00203917054206178,-0.0335916210442673,
-0.0107129653486114));
#38666=CARTESIAN_POINT('Ctrl Pts',(0.00190236078592673,-0.0336056011872405,
-0.0105392696668422));
#38667=CARTESIAN_POINT('Ctrl Pts',(0.00174662181156177,-0.0336195308554648,
-0.0103871911475904));
#38668=CARTESIAN_POINT('Ctrl Pts',(0.00139879381563512,-0.033650641427511,
-0.0100475384255241));
#38669=CARTESIAN_POINT('Ctrl Pts',(0.000950022516408242,-0.0336815002268697,
-0.00981346098105522));
#38670=CARTESIAN_POINT('Ctrl Pts',(0.000475693111364957,-0.0337122238801269,
-0.00972152729684118));
#38671=CARTESIAN_POINT('Ctrl Pts',(0.000305720759323992,-0.0337232334687206,
-0.00968858355696019));
#38672=CARTESIAN_POINT('Ctrl Pts',(0.000132665409089458,-0.0337342257032983,
-0.0096734345216426));
#38673=CARTESIAN_POINT('Ctrl Pts',(-3.96491736052501E-5,-0.033745205950374,
-0.00967616771772501));
#38674=CARTESIAN_POINT('Ctrl Pts',(-0.000518700898371905,-0.0337757321323009,
-0.00968376627541482));
#38675=CARTESIAN_POINT('Ctrl Pts',(-0.00099485729999462,-0.0338061656633708,
-0.00983333862689195));
#38676=CARTESIAN_POINT('Ctrl Pts',(-0.0013908613543846,-0.0338364750949364,
-0.0100984740017669));
#38677=CARTESIAN_POINT('Ctrl Pts',(-0.00153480325056549,-0.0338474921464119,
-0.0101948469761874));
#38678=CARTESIAN_POINT('Ctrl Pts',(-0.00166833809419712,-0.0338584928016113,
-0.0103060091403367));
#38679=CARTESIAN_POINT('Ctrl Pts',(-0.00178867736678944,-0.0338694755502296,
-0.0104292470694802));
#38680=CARTESIAN_POINT('Ctrl Pts',(-0.00212827609129081,-0.0339004689852232,
-0.0107770258340161));
#38681=CARTESIAN_POINT('Ctrl Pts',(-0.00236269258968325,-0.0339313198167728,
-0.0112261021386227));
#38682=CARTESIAN_POINT('Ctrl Pts',(-0.00245456493483844,-0.0339620393589644,
-0.0117013946680659));
#38683=CARTESIAN_POINT('Ctrl Pts',(-0.00248481221025082,-0.0339721532017279,
-0.0118578759684531));
#38684=CARTESIAN_POINT('Ctrl Pts',(-0.00250000044750102,-0.0339822528135889,
-0.0120170244069798));
#38685=CARTESIAN_POINT('Ctrl Pts',(-0.00249999999999008,-0.0339923385983081,
-0.0121758603301622));
#38686=CARTESIAN_POINT('',(-0.00214231189934805,-0.034078774338657,-0.0134644570759021));
#38687=CARTESIAN_POINT('Ctrl Pts',(-0.00249999938363598,-0.0339924495244571,
-0.0121776087977965));
#38688=CARTESIAN_POINT('Ctrl Pts',(-0.00249968291142358,-0.0340212244625237,
-0.0126282925180976));
#38689=CARTESIAN_POINT('Ctrl Pts',(-0.00237461305321147,-0.0340499994005904,
-0.0130782549408287));
#38690=CARTESIAN_POINT('Ctrl Pts',(-0.00214231189934805,-0.034078774338657,
-0.0134644570759021));
#38691=CARTESIAN_POINT('',(-0.000601546286298526,-0.0340787743898723,-0.00974930387114525));
#38692=CARTESIAN_POINT('Origin',(0.,-0.0340787743898623,-0.0121758532865581));
#38693=CARTESIAN_POINT('Ctrl Pts',(-0.000601546286299171,-0.0340787743898619,
-0.00974930387114541));
#38694=CARTESIAN_POINT('Ctrl Pts',(-0.000126738896636988,-0.034047633898331,
-0.00963159820228718));
#38695=CARTESIAN_POINT('Ctrl Pts',(0.000383109996741683,-0.0340164934068,
-0.00965749571553324));
#38696=CARTESIAN_POINT('Ctrl Pts',(0.000843239392728706,-0.033985352915269,
-0.00982235645704026));
#38697=CARTESIAN_POINT('Ctrl Pts',(0.000868642157086713,-0.0339836337150283,
-0.00983145806759789));
#38698=CARTESIAN_POINT('Ctrl Pts',(0.000893894990357826,-0.0339819145147875,
-0.00984097008168301));
#38699=CARTESIAN_POINT('Ctrl Pts',(0.000918984538856573,-0.0339801953145468,
-0.00985088717554861));
#38700=CARTESIAN_POINT('Ctrl Pts',(0.00136814293774854,-0.0339494178285532,
-0.0100284250855098));
#38701=CARTESIAN_POINT('Ctrl Pts',(0.00176464235916692,-0.0339186403425595,
-0.0103402207080788));
#38702=CARTESIAN_POINT('Ctrl Pts',(0.00204312011347985,-0.0338878628565659,
-0.0107351381162715));
#38703=CARTESIAN_POINT('Ctrl Pts',(0.00206196011845155,-0.0338857806507877,
-0.0107618556756403));
#38704=CARTESIAN_POINT('Ctrl Pts',(0.00208027315665946,-0.0338836984450094,
-0.0107889388407447));
#38705=CARTESIAN_POINT('Ctrl Pts',(0.00209804524141437,-0.0338816162392312,
-0.0108163658224826));
#38706=CARTESIAN_POINT('Ctrl Pts',(0.00236143596159679,-0.0338507569626153,
-0.0112228466924531));
#38707=CARTESIAN_POINT('Ctrl Pts',(0.00250323127272012,-0.0338198976859994,
-0.0117083446996253));
#38708=CARTESIAN_POINT('Ctrl Pts',(0.00249994239779229,-0.0337890384093834,
-0.0121928240767732));
#38709=CARTESIAN_POINT('Ctrl Pts',(0.00249972920046646,-0.0337870379942275,
-0.0122242298644343));
#38710=CARTESIAN_POINT('Ctrl Pts',(0.0024989241470306,-0.0337850375790716,
-0.0122556273663398));
#38711=CARTESIAN_POINT('Ctrl Pts',(0.00249752833899235,-0.0337830371639157,
-0.0122869937199302));
#38712=CARTESIAN_POINT('Ctrl Pts',(0.00247600395694093,-0.0337521892973773,
-0.0127706858607799));
#38713=CARTESIAN_POINT('Ctrl Pts',(0.00230970703782302,-0.0337213414308389,
-0.0132481441899844));
#38714=CARTESIAN_POINT('Ctrl Pts',(0.00202594814670806,-0.0336904935643004,
-0.0136406174678686));
#38715=CARTESIAN_POINT('Ctrl Pts',(0.00200744205985623,-0.033688481739067,
-0.0136662136510895));
#38716=CARTESIAN_POINT('Ctrl Pts',(0.00198845339528052,-0.0336864699138336,
-0.0136914555244219));
#38717=CARTESIAN_POINT('Ctrl Pts',(0.00196899657661983,-0.0336844580886002,
-0.0137163247991994));
#38718=CARTESIAN_POINT('Ctrl Pts',(0.00167065985465431,-0.0336536102220617,
-0.0140976521911113));
#38719=CARTESIAN_POINT('Ctrl Pts',(0.00125806506077489,-0.0336227623555233,
-0.01438986140707));
#38720=CARTESIAN_POINT('Ctrl Pts',(0.000799163142138323,-0.0335919144889848,
-0.0145446796356702));
#38721=CARTESIAN_POINT('Ctrl Pts',(0.00076923463935431,-0.0335899026637514,
-0.0145547765160655));
#38722=CARTESIAN_POINT('Ctrl Pts',(0.00073911888749589,-0.033587890838518,
-0.0145643047397628));
#38723=CARTESIAN_POINT('Ctrl Pts',(0.000708838248187203,-0.0335858790132846,
-0.0145732577868264));
#38724=CARTESIAN_POINT('Ctrl Pts',(0.000244365187101707,-0.0335550197366687,
-0.0147105880833672));
#38725=CARTESIAN_POINT('Ctrl Pts',(-0.000261412390778464,-0.0335241604600528,
-0.0147089147516458));
#38726=CARTESIAN_POINT('Ctrl Pts',(-0.000725083512180734,-0.0334933011834368,
-0.0145683945924426));
#38727=CARTESIAN_POINT('Ctrl Pts',(-0.00075514042991596,-0.0334913007682809,
-0.0145592855436571));
#38728=CARTESIAN_POINT('Ctrl Pts',(-0.000785021614133495,-0.033489300353125,
-0.014549611254258));
#38729=CARTESIAN_POINT('Ctrl Pts',(-0.0008147054510334,-0.0334872999379691,
-0.014539379260195));
#38730=CARTESIAN_POINT('Ctrl Pts',(-0.00127140758694842,-0.0334565224519755,
-0.0143819544111438));
#38731=CARTESIAN_POINT('Ctrl Pts',(-0.00168135115512026,-0.0334257449659819,
-0.0140880467024281));
#38732=CARTESIAN_POINT('Ctrl Pts',(-0.00197705569024059,-0.0333949674799883,
-0.0137059679220307));
#38733=CARTESIAN_POINT('Ctrl Pts',(-0.00199706114785999,-0.0333928852742101,
-0.0136801189412384));
#38734=CARTESIAN_POINT('Ctrl Pts',(-0.00201655633294717,-0.0333908030684318,
-0.0136538817710384));
#38735=CARTESIAN_POINT('Ctrl Pts',(-0.00203552635298372,-0.0333887208626536,
-0.0136272775754236));
#38736=CARTESIAN_POINT('Ctrl Pts',(-0.00231923306173773,-0.0333575803711226,
-0.0132293977227732));
#38737=CARTESIAN_POINT('Ctrl Pts',(-0.00248283147535909,-0.0333264398795917,
-0.0127458468591014));
#38738=CARTESIAN_POINT('Ctrl Pts',(-0.00249868674944542,-0.0332952993880607,
-0.0122568750623093));
#38739=CARTESIAN_POINT('Ctrl Pts',(-0.00249956208537264,-0.0332935801878198,
-0.0122298799704049));
#38740=CARTESIAN_POINT('Ctrl Pts',(-0.00249999986943493,-0.0332918609875789,
-0.012202871934591));
#38741=CARTESIAN_POINT('Ctrl Pts',(-0.0024999999999708,-0.033290141787338,
-0.0121758653702745));
#38742=CARTESIAN_POINT('Origin',(0.,-0.0342787743898723,-0.0121758532865581));
#38743=CARTESIAN_POINT('',(-0.00299999988642399,-0.031703806066922,-0.0121752798029594));
#38744=CARTESIAN_POINT('',(-0.00299999939184732,-0.0307036990116105,-0.0121771829558748));
#38745=CARTESIAN_POINT('Ctrl Pts',(-0.00299999977291662,-0.0317037743898623,
-0.0121746860247103));
#38746=CARTESIAN_POINT('Ctrl Pts',(-0.00299978312826752,-0.0316742289770476,
-0.0116178838818835));
#38747=CARTESIAN_POINT('Ctrl Pts',(-0.00284025273261327,-0.0316446835642328,
-0.0110610251285104));
#38748=CARTESIAN_POINT('Ctrl Pts',(-0.00254573842885079,-0.0316151381514181,
-0.0105886495025807));
#38749=CARTESIAN_POINT('Ctrl Pts',(-0.00242491146118173,-0.0316030168975662,
-0.0103948534330767));
#38750=CARTESIAN_POINT('Ctrl Pts',(-0.00228196716891504,-0.0315908956437142,
-0.0102151071015685));
#38751=CARTESIAN_POINT('Ctrl Pts',(-0.00212084111800276,-0.0315787743898623,
-0.0100540538256785));
#38752=CARTESIAN_POINT('Ctrl Pts',(-0.00173533258476648,-0.0315497732024876,
-0.00966871941321266));
#38753=CARTESIAN_POINT('Ctrl Pts',(-0.00124021229841889,-0.031520772015113,
-0.00938998950206325));
#38754=CARTESIAN_POINT('Ctrl Pts',(-0.000708736353863526,-0.0314917708277383,
-0.00926077305083349));
#38755=CARTESIAN_POINT('Ctrl Pts',(-0.000476628699683858,-0.0314791053484463,
-0.00920434128250303));
#38756=CARTESIAN_POINT('Ctrl Pts',(-0.000237958547009543,-0.0314664398691543,
-0.0091758383654527));
#38757=CARTESIAN_POINT('Ctrl Pts',(1.88039627964167E-7,-0.0314537743898623,
-0.00917585329245125));
#38758=CARTESIAN_POINT('Ctrl Pts',(0.000547508419203228,-0.0314246659527796,
-0.00917588759842483));
#38759=CARTESIAN_POINT('Ctrl Pts',(0.00109662914758601,-0.0313955575156969,
-0.00933003319063454));
#38760=CARTESIAN_POINT('Ctrl Pts',(0.00156492802349207,-0.0313664490786142,
-0.00961636109448382));
#38761=CARTESIAN_POINT('Ctrl Pts',(0.00176696583063482,-0.0313538908490302,
-0.00973989131160331));
#38762=CARTESIAN_POINT('Ctrl Pts',(0.00195411565321174,-0.0313413326194463,
-0.00988736184395037));
#38763=CARTESIAN_POINT('Ctrl Pts',(0.00212110708959182,-0.0313287743898623,
-0.0100543197104667));
#38764=CARTESIAN_POINT('Ctrl Pts',(0.00250809996203972,-0.0312996714283877,
-0.0104412347867216));
#38765=CARTESIAN_POINT('Ctrl Pts',(0.00278743908090049,-0.0312705684669131,
-0.0109383763719027));
#38766=CARTESIAN_POINT('Ctrl Pts',(0.00291622376994772,-0.0312414655054385,
-0.0114718370057862));
#38767=CARTESIAN_POINT('Ctrl Pts',(0.00297181992870467,-0.0312289018002464,
-0.0117021311681698));
#38768=CARTESIAN_POINT('Ctrl Pts',(0.00299993759600436,-0.0312163380950544,
-0.0119388347240268));
#38769=CARTESIAN_POINT('Ctrl Pts',(0.00299999989567168,-0.0312037743898623,
-0.0121750621039462));
#38770=CARTESIAN_POINT('Ctrl Pts',(0.00300014420857858,-0.0311746714283877,
-0.0127222666293588));
#38771=CARTESIAN_POINT('Ctrl Pts',(0.00284624088932268,-0.0311455684669131,
-0.0132713404189909));
#38772=CARTESIAN_POINT('Ctrl Pts',(0.00256016617521376,-0.0311164655054385,
-0.0137396784543091));
#38773=CARTESIAN_POINT('Ctrl Pts',(0.00243666814653024,-0.0311039018002464,
-0.0139418592877304));
#38774=CARTESIAN_POINT('Ctrl Pts',(0.00228920193131261,-0.0310913380950544,
-0.0141291490201574));
#38775=CARTESIAN_POINT('Ctrl Pts',(0.00212222580814811,-0.0310787743898623,
-0.0142962677788756));
#38776=CARTESIAN_POINT('Ctrl Pts',(0.00173536429706138,-0.0310496659527796,
-0.0146834597576052));
#38777=CARTESIAN_POINT('Ctrl Pts',(0.00123820729474145,-0.0310205575156969,
-0.0149629884269283));
#38778=CARTESIAN_POINT('Ctrl Pts',(0.000704674944244704,-0.0309914490786142,
-0.0150919179674172));
#38779=CARTESIAN_POINT('Ctrl Pts',(0.000474493511659587,-0.0309788908490302,
-0.0151475419353071));
#38780=CARTESIAN_POINT('Ctrl Pts',(0.000237900354987811,-0.0309663326194463,
-0.0151757134156151));
#38781=CARTESIAN_POINT('Ctrl Pts',(1.77040476739121E-6,-0.0309537743898623,
-0.0151758527641692));
#38782=CARTESIAN_POINT('Ctrl Pts',(-0.000543533285161779,-0.0309247732024876,
-0.015176174566976));
#38783=CARTESIAN_POINT('Ctrl Pts',(-0.00109089993736176,-0.030895772015113,
-0.0150234838642021));
#38784=CARTESIAN_POINT('Ctrl Pts',(-0.00155821273132624,-0.0308667708277383,
-0.014739439267939));
#38785=CARTESIAN_POINT('Ctrl Pts',(-0.00176229887574436,-0.0308541053484463,
-0.0146153905210551));
#38786=CARTESIAN_POINT('Ctrl Pts',(-0.00195127257021304,-0.0308414398691543,
-0.0144669665921402));
#38787=CARTESIAN_POINT('Ctrl Pts',(-0.00211972166913044,-0.0308287743898623,
-0.0142987711006571));
#38788=CARTESIAN_POINT('Ctrl Pts',(-0.00251267151737878,-0.0307992289770476,
-0.0139064128554713));
#38789=CARTESIAN_POINT('Ctrl Pts',(-0.0027945897162608,-0.0307696835642329,
-0.0134009438838064));
#38790=CARTESIAN_POINT('Ctrl Pts',(-0.00292135667822606,-0.0307401381514181,
-0.0128582572421328));
#38791=CARTESIAN_POINT('Ctrl Pts',(-0.00297336388948608,-0.0307280168975662,
-0.012635615487657));
#38792=CARTESIAN_POINT('Ctrl Pts',(-0.00299978937163709,-0.0307158956437142,
-0.0124070355920604));
#38793=CARTESIAN_POINT('Ctrl Pts',(-0.00299999873992521,-0.0307037743898623,
-0.0121786029132924));
#38794=CARTESIAN_POINT('',(-0.00299999999999987,-0.0297037907762723,-0.0121758524173738));
#38795=CARTESIAN_POINT('Ctrl Pts',(-0.00299999999999574,-0.0307036286946763,
-0.0121758583423425));
#38796=CARTESIAN_POINT('Ctrl Pts',(-0.00300000093834573,-0.0306740944474691,
-0.0116190604763335));
#38797=CARTESIAN_POINT('Ctrl Pts',(-0.00284069050734933,-0.0306445602002618,
-0.0110621430487859));
#38798=CARTESIAN_POINT('Ctrl Pts',(-0.00254636475893709,-0.0306150259530546,
-0.0105896545239677));
#38799=CARTESIAN_POINT('Ctrl Pts',(-0.00242552546022251,-0.0306029002802589,
-0.0103956681592079));
#38800=CARTESIAN_POINT('Ctrl Pts',(-0.00228253061514852,-0.0305907746074633,
-0.010215743637405));
#38801=CARTESIAN_POINT('Ctrl Pts',(-0.00212132312544701,-0.0305786489346676,
-0.0100545357248895));
#38802=CARTESIAN_POINT('Ctrl Pts',(-0.00173590887930689,-0.0305496589228007,
-0.00966912046788729));
#38803=CARTESIAN_POINT('Ctrl Pts',(-0.00124086089003451,-0.0305206689109338,
-0.00939027980684245));
#38804=CARTESIAN_POINT('Ctrl Pts',(-0.000709422677418312,-0.0304916788990669,
-0.0092609400005812));
#38805=CARTESIAN_POINT('Ctrl Pts',(-0.000477160843076479,-0.0304790089909309,
-0.00920441282593983));
#38806=CARTESIAN_POINT('Ctrl Pts',(-0.000238320408519796,-0.0304663390827949,
-0.00917585350998904));
#38807=CARTESIAN_POINT('Ctrl Pts',(-2.81258648426431E-9,-0.0304536691746589,
-0.00917585328655942));
#38808=CARTESIAN_POINT('Ctrl Pts',(0.000547308636665276,-0.0304245719283702,
-0.00917585277343916));
#38809=CARTESIAN_POINT('Ctrl Pts',(0.0010964320589705,-0.0303954746820815,
-0.00932995861975189));
#38810=CARTESIAN_POINT('Ctrl Pts',(0.00156474531708854,-0.0303663774357928,
-0.00961624939285707));
#38811=CARTESIAN_POINT('Ctrl Pts',(0.00176693856243628,-0.0303538147620786,
-0.00973985482047163));
#38812=CARTESIAN_POINT('Ctrl Pts',(0.00195422378185452,-0.0303412520883644,
-0.00988743656966469));
#38813=CARTESIAN_POINT('Ctrl Pts',(0.00212131914785055,-0.0303286894146501,
-0.01005453174729));
#38814=CARTESIAN_POINT('Ctrl Pts',(0.00250826720070462,-0.0302995976316232,
-0.0104414793639281));
#38815=CARTESIAN_POINT('Ctrl Pts',(0.00278755503992261,-0.0302705058485962,
-0.0109386406709272));
#38816=CARTESIAN_POINT('Ctrl Pts',(0.00291628881227279,-0.0302414140655693,
-0.0114721064830751));
#38817=CARTESIAN_POINT('Ctrl Pts',(0.0029719039556564,-0.0302288459285933,
-0.011702572638857));
#38818=CARTESIAN_POINT('Ctrl Pts',(0.00299999995513255,-0.0302162777916174,
-0.0119394549660179));
#38819=CARTESIAN_POINT('Ctrl Pts',(0.00299999999999995,-0.0302037096546414,
-0.0121758527171695));
#38820=CARTESIAN_POINT('Ctrl Pts',(0.00300000010385564,-0.0301746178716145,
-0.0127230485424311));
#38821=CARTESIAN_POINT('Ctrl Pts',(0.00284595678365275,-0.0301455260885875,
-0.0132720748242642));
#38822=CARTESIAN_POINT('Ctrl Pts',(0.00255976580244818,-0.0301164343055606,
-0.0137403337231941));
#38823=CARTESIAN_POINT('Ctrl Pts',(0.00243612651056531,-0.0301038661685846,
-0.013942629401548));
#38824=CARTESIAN_POINT('Ctrl Pts',(0.00228848792214319,-0.0300912980316087,
-0.0141300061130754));
#38825=CARTESIAN_POINT('Ctrl Pts',(0.00212131995308795,-0.0300787298946327,
-0.0142971740205894));
#38826=CARTESIAN_POINT('Ctrl Pts',(0.001734299380629,-0.030049632648344,
-0.0146841944505705));
#38827=CARTESIAN_POINT('Ctrl Pts',(0.00123703143457719,-0.0300205354020554,
-0.0149635091150117));
#38828=CARTESIAN_POINT('Ctrl Pts',(0.000703451975723402,-0.0299914381557667,
-0.0150922132296808));
#38829=CARTESIAN_POINT('Ctrl Pts',(0.00047308018810817,-0.0299788754820525,
-0.0151477809553078));
#38830=CARTESIAN_POINT('Ctrl Pts',(0.000236298871225366,-0.0299663128083382,
-0.0151758534183983));
#38831=CARTESIAN_POINT('Ctrl Pts',(-1.67380927159913E-9,-0.029953750134624,
-0.0151758532865576));
#38832=CARTESIAN_POINT('Ctrl Pts',(-0.000545296072162418,-0.0299247601227571,
-0.015175852982318));
#38833=CARTESIAN_POINT('Ctrl Pts',(-0.00109256494565921,-0.0298957701108902,
-0.0150228440193565));
#38834=CARTESIAN_POINT('Ctrl Pts',(-0.00155970580473139,-0.0298667800990233,
-0.0147385311443247));
#38835=CARTESIAN_POINT('Ctrl Pts',(-0.0017638668722805,-0.0298541101908873,
-0.0146142739337699));
#38836=CARTESIAN_POINT('Ctrl Pts',(-0.00195287930718518,-0.0298414402827513,
-0.014465614980402));
#38837=CARTESIAN_POINT('Ctrl Pts',(-0.00212132232021082,-0.0298287703746153,
-0.0142971716534647));
#38838=CARTESIAN_POINT('Ctrl Pts',(-0.00251397211262461,-0.0297992361320834,
-0.0139045211293059));
#38839=CARTESIAN_POINT('Ctrl Pts',(-0.00279550818297967,-0.0297697018895515,
-0.0133988448080529));
#38840=CARTESIAN_POINT('Ctrl Pts',(-0.00292186740455529,-0.0297401676470197,
-0.0128560671280795));
#38841=CARTESIAN_POINT('Ctrl Pts',(-0.00297374563895877,-0.0297280420234372,
-0.0126332234973613));
#38842=CARTESIAN_POINT('Ctrl Pts',(-0.00300000006623164,-0.0297159163998547,
-0.0124044521585));
#38843=CARTESIAN_POINT('Ctrl Pts',(-0.00299999999999987,-0.0297037907762723,
-0.0121758524173738));
#38844=CARTESIAN_POINT('',(0.00267183091333631,-0.0292787743898623,-0.0108115514246007));
#38845=CARTESIAN_POINT('Ctrl Pts',(-0.00299999998382998,-0.0297037743898623,
-0.0121755418060137));
#38846=CARTESIAN_POINT('Ctrl Pts',(-0.00299994185979298,-0.0296740643174192,
-0.0116157247863023));
#38847=CARTESIAN_POINT('Ctrl Pts',(-0.00283892252328663,-0.0296443542449761,
-0.0110562397396311));
#38848=CARTESIAN_POINT('Ctrl Pts',(-0.00254172294431946,-0.029614644172533,
-0.0105822270837364));
#38849=CARTESIAN_POINT('Ctrl Pts',(-0.00248463801449189,-0.0296089375783095,
-0.0104911805913653));
#38850=CARTESIAN_POINT('Ctrl Pts',(-0.00242267577881712,-0.0296032309840859,
-0.0104032360322616));
#38851=CARTESIAN_POINT('Ctrl Pts',(-0.0023562110315139,-0.0295975243898623,
-0.010318901597641));
#38852=CARTESIAN_POINT('Ctrl Pts',(-0.00201476491589461,-0.0295682081807422,
-0.00988565440597122));
#38853=CARTESIAN_POINT('Ctrl Pts',(-0.0015498817289811,-0.029538891971622,
-0.00954850647314129));
#38854=CARTESIAN_POINT('Ctrl Pts',(-0.00103119238248645,-0.0295095757625019,
-0.00935864859568065));
#38855=CARTESIAN_POINT('Ctrl Pts',(-0.000923257474355454,-0.0295034753049554,
-0.0093191407617524));
#38856=CARTESIAN_POINT('Ctrl Pts',(-0.000813093493369863,-0.0294973748474088,
-0.00928585976408999));
#38857=CARTESIAN_POINT('Ctrl Pts',(-0.000701456466827434,-0.0294912743898623,
-0.00925901273124042));
#38858=CARTESIAN_POINT('Ctrl Pts',(-0.00016497631092072,-0.0294619581807422,
-0.00912999728882986));
#38859=CARTESIAN_POINT('Ctrl Pts',(0.000408862167047048,-0.029432641971622,
-0.00915297278038173));
#38860=CARTESIAN_POINT('Ctrl Pts',(0.000933680525875383,-0.0294033257625019,
-0.0093248463283763));
#38861=CARTESIAN_POINT('Ctrl Pts',(0.00104289083013255,-0.0293972253049554,
-0.00936061177399095));
#38862=CARTESIAN_POINT('Ctrl Pts',(0.00114999357473004,-0.0293911248474088,
-0.00940264375250374));
#38863=CARTESIAN_POINT('Ctrl Pts',(0.00125426789939748,-0.0293850243898623,
-0.00945063549039189));
#38864=CARTESIAN_POINT('Ctrl Pts',(0.0017620982901821,-0.0293553143174192,
-0.00968436189508353));
#38865=CARTESIAN_POINT('Ctrl Pts',(0.00220321097255991,-0.0293256042449762,
-0.0100641074196941));
#38866=CARTESIAN_POINT('Ctrl Pts',(0.00250994897180209,-0.0292958941725331,
-0.0105326380970745));
#38867=CARTESIAN_POINT('Ctrl Pts',(0.00256886600399653,-0.0292901875783095,
-0.010622631632507));
#38868=CARTESIAN_POINT('Ctrl Pts',(0.00262293094262228,-0.0292844809840859,
-0.0107157863618546));
#38869=CARTESIAN_POINT('Ctrl Pts',(0.00267183091333631,-0.0292787743898623,
-0.0108115514246007));
#38870=CARTESIAN_POINT('',(0.000927050983124848,-0.0292787743898723,-0.00932268373767264));
#38871=CARTESIAN_POINT('Origin',(0.,-0.0292787743898623,-0.0121758532865581));
#38872=CARTESIAN_POINT('',(-0.00299999932318279,-0.0295787743898623,-0.0121778684547369));
#38873=CARTESIAN_POINT('Ctrl Pts',(0.000927050983124362,-0.0292787743898627,
-0.00932268373767248));
#38874=CARTESIAN_POINT('Ctrl Pts',(0.000403615972859334,-0.029307962090938,
-0.0091526093931396));
#38875=CARTESIAN_POINT('Ctrl Pts',(-0.00016905585335949,-0.0293371497920133,
-0.00913038402760189));
#38876=CARTESIAN_POINT('Ctrl Pts',(-0.00108600803646328,-0.0293871316591116,
-0.00935191796589178));
#38877=CARTESIAN_POINT('Ctrl Pts',(-0.00144812628843063,-0.0294079258251344,
-0.009519776883436));
#38878=CARTESIAN_POINT('Ctrl Pts',(-0.00220580055780451,-0.0294579076922327,
-0.0100702541868122));
#38879=CARTESIAN_POINT('Ctrl Pts',(-0.0025605860953725,-0.0294870953933081,
-0.0105182936949274));
#38880=CARTESIAN_POINT('Ctrl Pts',(-0.00292197599480409,-0.0295370772604064,
-0.0113907378054678));
#38881=CARTESIAN_POINT('Ctrl Pts',(-0.00299999642597719,-0.0295578714264294,
-0.0117837248437925));
#38882=CARTESIAN_POINT('Ctrl Pts',(-0.00299999999987538,-0.0295786655924524,
-0.0121758259423486));
#38883=CARTESIAN_POINT('',(-0.00299999937953697,-0.0305788301727905,-0.0121743809549774));
#38884=CARTESIAN_POINT('Ctrl Pts',(-0.00299999932318279,-0.0295787743898623,
-0.0121778684547369));
#38885=CARTESIAN_POINT('Ctrl Pts',(-0.00299962530604328,-0.0296083208102491,
-0.0127346711956747));
#38886=CARTESIAN_POINT('Ctrl Pts',(-0.00283993715789012,-0.0296378672306359,
-0.0132914854094396));
#38887=CARTESIAN_POINT('Ctrl Pts',(-0.00254528873352183,-0.0296674136510226,
-0.0137637781157005));
#38888=CARTESIAN_POINT('Ctrl Pts',(-0.00242442091188463,-0.0296795338973025,
-0.0139575174533646));
#38889=CARTESIAN_POINT('Ctrl Pts',(-0.00228144489908848,-0.0296916541435824,
-0.0141372040791591));
#38890=CARTESIAN_POINT('Ctrl Pts',(-0.00212029612942546,-0.0297037743898623,
-0.0142981973499803));
#38891=CARTESIAN_POINT('Ctrl Pts',(-0.00173468758494504,-0.0297327766002826,
-0.014683433805476));
#38892=CARTESIAN_POINT('Ctrl Pts',(-0.00123949431793212,-0.0297617788107028,
-0.0149620368237008));
#38893=CARTESIAN_POINT('Ctrl Pts',(-0.000707983886383787,-0.0297907810211231,
-0.0150911163650162));
#38894=CARTESIAN_POINT('Ctrl Pts',(-0.000475888107913542,-0.0298034454773695,
-0.0151474817999126));
#38895=CARTESIAN_POINT('Ctrl Pts',(-0.000237238539839443,-0.0298161099336159,
-0.0151759230887667));
#38896=CARTESIAN_POINT('Ctrl Pts',(8.81047802455638E-7,-0.0298287743898623,
-0.0151758531571839));
#38897=CARTESIAN_POINT('Ctrl Pts',(0.00054820281424355,-0.0298578838496612,
-0.0151756924182971));
#38898=CARTESIAN_POINT('Ctrl Pts',(0.0010972890419145,-0.0298869933094601,
-0.0150214192221399));
#38899=CARTESIAN_POINT('Ctrl Pts',(0.00156552236723977,-0.029916102769259,
-0.0147349819893927));
#38900=CARTESIAN_POINT('Ctrl Pts',(0.0017675083459938,-0.0299286599761268,
-0.0146114190098294));
#38901=CARTESIAN_POINT('Ctrl Pts',(0.00195460421385389,-0.0299412171829946,
-0.0144639246845766));
#38902=CARTESIAN_POINT('Ctrl Pts',(0.00212154235467162,-0.0299537743898623,
-0.0142969515957683));
#38903=CARTESIAN_POINT('Ctrl Pts',(0.00250845679834444,-0.0299828783722448,
-0.0139099561527368));
#38904=CARTESIAN_POINT('Ctrl Pts',(0.00278769415448554,-0.0300119823546272,
-0.0134127559676335));
#38905=CARTESIAN_POINT('Ctrl Pts',(0.00291636900172886,-0.0300410863370097,
-0.0128792677061963));
#38906=CARTESIAN_POINT('Ctrl Pts',(0.00297191127975778,-0.0300536490212939,
-0.012648988409374));
#38907=CARTESIAN_POINT('Ctrl Pts',(0.00299998006402622,-0.0300662117055781,
-0.0124123068592859));
#38908=CARTESIAN_POINT('Ctrl Pts',(0.0029999999893257,-0.0300787743898623,
-0.0121761063592579));
#38909=CARTESIAN_POINT('Ctrl Pts',(0.00300004615028558,-0.0301078783722448,
-0.0116289004408389));
#38910=CARTESIAN_POINT('Ctrl Pts',(0.00284604360528892,-0.0301369823546272,
-0.011079853172088));
#38911=CARTESIAN_POINT('Ctrl Pts',(0.00255988376205479,-0.0301660863370097,
-0.010611565868988));
#38912=CARTESIAN_POINT('Ctrl Pts',(0.00243636335449944,-0.0301786490212939,
-0.0104094304544652));
#38913=CARTESIAN_POINT('Ctrl Pts',(0.00228888295904802,-0.0301912117055781,
-0.0102221870407097));
#38914=CARTESIAN_POINT('Ctrl Pts',(0.0021219001858595,-0.0302037743898623,
-0.0100551129438359));
#38915=CARTESIAN_POINT('Ctrl Pts',(0.00173497823404734,-0.0302328838496612,
-0.00966797938253934));
#38916=CARTESIAN_POINT('Ctrl Pts',(0.00123777698915588,-0.0302619933094601,
-0.00938852679820759));
#38917=CARTESIAN_POINT('Ctrl Pts',(0.000704223598844007,-0.030291102769259,
-0.00925967957382575));
#38918=CARTESIAN_POINT('Ctrl Pts',(0.000474059922038583,-0.0303036599761268,
-0.00920409759937224));
#38919=CARTESIAN_POINT('Ctrl Pts',(0.000237490241918617,-0.0303162171829945,
-0.00917596278079916));
#38920=CARTESIAN_POINT('Ctrl Pts',(1.38719316590359E-6,-0.0303287743898623,
-0.0091758536072756));
#38921=CARTESIAN_POINT('Ctrl Pts',(-0.000543918014664728,-0.0303577766002826,
-0.00917560145936276));
#38922=CARTESIAN_POINT('Ctrl Pts',(-0.00109126634046794,-0.0303867788107028,
-0.00932836287458711));
#38923=CARTESIAN_POINT('Ctrl Pts',(-0.00155854349046879,-0.0304157810211231,
-0.00961246837821574));
#38924=CARTESIAN_POINT('Ctrl Pts',(-0.00176259038673546,-0.0304284454773695,
-0.00973652932625824));
#38925=CARTESIAN_POINT('Ctrl Pts',(-0.00195152515402665,-0.0304411099336159,
-0.00988495792512666));
#38926=CARTESIAN_POINT('Ctrl Pts',(-0.00211993802768848,-0.0304537743898623,
-0.0100531515272993));
#38927=CARTESIAN_POINT('Ctrl Pts',(-0.00251284850619159,-0.030483320810249,
-0.0104455504411943));
#38928=CARTESIAN_POINT('Ctrl Pts',(-0.00279471530702616,-0.0305128672306358,
-0.0109510489415062));
#38929=CARTESIAN_POINT('Ctrl Pts',(-0.00292142670497378,-0.0305424136510226,
-0.011493749183458));
#38930=CARTESIAN_POINT('Ctrl Pts',(-0.002973405026865,-0.0305545338973025,
-0.011716370418197));
#38931=CARTESIAN_POINT('Ctrl Pts',(-0.00299980697922492,-0.0305666541435824,
-0.011944925777034));
#38932=CARTESIAN_POINT('Ctrl Pts',(-0.00299999894049624,-0.0305787743898623,
-0.0121733319731243));
#38933=CARTESIAN_POINT('',(-0.00299999999999953,-0.0315788060372049,-0.0121758516139528));
#38934=CARTESIAN_POINT('Ctrl Pts',(-0.00299999999998308,-0.0305789090044302,
-0.0121758633611915));
#38935=CARTESIAN_POINT('Ctrl Pts',(-0.002999998130136,-0.0306084450666598,
-0.0127326619098351));
#38936=CARTESIAN_POINT('Ctrl Pts',(-0.00284068451932866,-0.0306379811288893,
-0.0132895791065831));
#38937=CARTESIAN_POINT('Ctrl Pts',(-0.00254635576498619,-0.0306675171911189,
-0.0137620664872728));
#38938=CARTESIAN_POINT('Ctrl Pts',(-0.00242552940725285,-0.0306796421866157,
-0.0139560296269302));
#38939=CARTESIAN_POINT('Ctrl Pts',(-0.00228255274909621,-0.0306917671821125,
-0.0141359340922567));
#38940=CARTESIAN_POINT('Ctrl Pts',(-0.00212136726850902,-0.0307038921776093,
-0.0142971267041303));
#38941=CARTESIAN_POINT('Ctrl Pts',(-0.00173595997884731,-0.0307328840051272,
-0.0146825510452645));
#38942=CARTESIAN_POINT('Ctrl Pts',(-0.0012409163762974,-0.0307618758326452,
-0.0149614022816779));
#38943=CARTESIAN_POINT('Ctrl Pts',(-0.000709479533810012,-0.0307908676601631,
-0.015090752734413));
#38944=CARTESIAN_POINT('Ctrl Pts',(-0.0004772452707397,-0.0308035368903715,
-0.0151472779969976));
#38945=CARTESIAN_POINT('Ctrl Pts',(-0.000238433368114515,-0.0308162061205799,
-0.0151758419405363));
#38946=CARTESIAN_POINT('Ctrl Pts',(-1.42799900971172E-7,-0.0308288753507883,
-0.0151758532831595));
#38947=CARTESIAN_POINT('Ctrl Pts',(0.000547170060450925,-0.0308579744153287,
-0.0151758793352336));
#38948=CARTESIAN_POINT('Ctrl Pts',(0.00109630179715439,-0.0308870734798691,
-0.0150217983519956));
#38949=CARTESIAN_POINT('Ctrl Pts',(0.00156462901955293,-0.0309161725444094,
-0.0147355282720148));
#38950=CARTESIAN_POINT('Ctrl Pts',(0.00176680470696733,-0.0309287345375954,
-0.0146119461964099));
#38951=CARTESIAN_POINT('Ctrl Pts',(0.00195407689624954,-0.0309412965307813,
-0.0144643926465557));
#38952=CARTESIAN_POINT('Ctrl Pts',(0.00212116531380692,-0.0309538585239673,
-0.0142973286485414));
#38953=CARTESIAN_POINT('Ctrl Pts',(0.00250814239611413,-0.0309829521232851,
-0.0139104081219411));
#38954=CARTESIAN_POINT('Ctrl Pts',(0.00278746653687675,-0.0310120457226029,
-0.0134132657730967));
#38955=CARTESIAN_POINT('Ctrl Pts',(0.00291623861273731,-0.0310411393219208,
-0.0128798080816835));
#38956=CARTESIAN_POINT('Ctrl Pts',(0.00297186382740656,-0.0310537067803293,
-0.0126493722639526));
#38957=CARTESIAN_POINT('Ctrl Pts',(0.00299997668915932,-0.0310662742387378,
-0.0124125197856121));
#38958=CARTESIAN_POINT('Ctrl Pts',(0.00299999998542944,-0.0310788416971463,
-0.0121761489609931));
#38959=CARTESIAN_POINT('Ctrl Pts',(0.00300005391617075,-0.0311079352964641,
-0.0116289517602262));
#38960=CARTESIAN_POINT('Ctrl Pts',(0.00284606386147954,-0.031137028895782,
-0.0110799092327468));
#38961=CARTESIAN_POINT('Ctrl Pts',(0.00255991781383716,-0.0311661224950998,
-0.0106116215945127));
#38962=CARTESIAN_POINT('Ctrl Pts',(0.00243631232545395,-0.0311786899535083,
-0.0104093370523894));
#38963=CARTESIAN_POINT('Ctrl Pts',(0.00228871161240723,-0.0311912574119168,
-0.0102219657098566));
#38964=CARTESIAN_POINT('Ctrl Pts',(0.00212158344994877,-0.0312038248703253,
-0.0100547960820246));
#38965=CARTESIAN_POINT('Ctrl Pts',(0.00173460996431537,-0.0312329239348657,
-0.00966772658624013));
#38966=CARTESIAN_POINT('Ctrl Pts',(0.00123737539096422,-0.0312620229994061,
-0.00938834989393673));
#38967=CARTESIAN_POINT('Ctrl Pts',(0.000703810673627834,-0.0312911220639464,
-0.00925957988790571));
#38968=CARTESIAN_POINT('Ctrl Pts',(0.000473472123254697,-0.0313036840571324,
-0.00920399019923815));
#38969=CARTESIAN_POINT('Ctrl Pts',(0.000236722135829542,-0.0313162460503184,
-0.00917588864684906));
#38970=CARTESIAN_POINT('Ctrl Pts',(4.48548968202519E-7,-0.0313288080435043,
-0.0091758533200908));
#38971=CARTESIAN_POINT('Ctrl Pts',(-0.000544847326927436,-0.0313577998710222,
-0.00917577178945572));
#38972=CARTESIAN_POINT('Ctrl Pts',(-0.00109214034091453,-0.0313867916985402,
-0.00932869941596481));
#38973=CARTESIAN_POINT('Ctrl Pts',(-0.00155932450626538,-0.0314157835260581,
-0.00961294340047934));
#38974=CARTESIAN_POINT('Ctrl Pts',(-0.00176348078916547,-0.0314284527562665,
-0.00973715607637691));
#38975=CARTESIAN_POINT('Ctrl Pts',(-0.00195249554526538,-0.0314411219864749,
-0.00988576715654636));
#38976=CARTESIAN_POINT('Ctrl Pts',(-0.00212094908975225,-0.0314537912166833,
-0.0100541617541531));
#38977=CARTESIAN_POINT('Ctrl Pts',(-0.00251366863868406,-0.0314833272789129,
-0.0104467438788933));
#38978=CARTESIAN_POINT('Ctrl Pts',(-0.00279529381109297,-0.0315128633411424,
-0.0109523715539673));
#38979=CARTESIAN_POINT('Ctrl Pts',(-0.00292174824045499,-0.031542399403372,
-0.0114951277769743));
#38980=CARTESIAN_POINT('Ctrl Pts',(-0.00297365967586053,-0.0315545243988687,
-0.0117179373278435));
#38981=CARTESIAN_POINT('Ctrl Pts',(-0.00299995411642938,-0.0315666493943655,
-0.0119466777319896));
#38982=CARTESIAN_POINT('Ctrl Pts',(-0.00299999993971496,-0.0315787743898623,
-0.0121752518630578));
#38983=CARTESIAN_POINT('',(-0.00299999948627239,-0.0325786872255947,-0.0121769732930159));
#38984=CARTESIAN_POINT('Ctrl Pts',(-0.00299999999999953,-0.0315788060372049,
-0.0121758516139528));
#38985=CARTESIAN_POINT('Ctrl Pts',(-0.00300000031042998,-0.0316082332034078,
-0.0127326424646223));
#38986=CARTESIAN_POINT('Ctrl Pts',(-0.0028406931286498,-0.031637678669113,
-0.0132895533835456));
#38987=CARTESIAN_POINT('Ctrl Pts',(-0.00254637369723003,-0.0316671428820116,
-0.013762037700192));
#38988=CARTESIAN_POINT('Ctrl Pts',(-0.00242550781667549,-0.031679242722038,
-0.0139560691737654));
#38989=CARTESIAN_POINT('Ctrl Pts',(-0.00228247616791868,-0.0316913457236565,
-0.0141360323583952));
#38990=CARTESIAN_POINT('Ctrl Pts',(-0.00212122458616147,-0.0317034519178721,
-0.0142972693831936));
#38991=CARTESIAN_POINT('Ctrl Pts',(-0.00173579172354728,-0.0317323888438919,
-0.0146826674509222));
#38992=CARTESIAN_POINT('Ctrl Pts',(-0.0012407291534123,-0.0317613440102813,
-0.0149614859389926));
#38993=CARTESIAN_POINT('Ctrl Pts',(-0.000709282271278857,-0.0317903161467925,
-0.0150908007405698));
#38994=CARTESIAN_POINT('Ctrl Pts',(-0.000476972294568734,-0.0318029806605651,
-0.0151473277794003));
#38995=CARTESIAN_POINT('Ctrl Pts',(-0.000238082320351396,-0.0318156484169943,
-0.0151758756826124));
#38996=CARTESIAN_POINT('Ctrl Pts',(2.82038538772012E-7,-0.0318283193099807,
-0.0151758532733005));
#38997=CARTESIAN_POINT('Ctrl Pts',(0.000547626181592029,-0.0318574148471478,
-0.0151758018159195));
#38998=CARTESIAN_POINT('Ctrl Pts',(0.00109676449279499,-0.0318865269226405,
-0.0150216259929139));
#38999=CARTESIAN_POINT('Ctrl Pts',(0.00156506872148099,-0.0319156602466803,
-0.0147352594475732));
#39000=CARTESIAN_POINT('Ctrl Pts',(0.0017672604829583,-0.0319282386470971,
-0.014611619828958));
#39001=CARTESIAN_POINT('Ctrl Pts',(0.00195453948115426,-0.0319408210084698,
-0.01446400220402));
#39002=CARTESIAN_POINT('Ctrl Pts',(0.00212162342931928,-0.0319534077098926,
-0.0142968705010482));
#39003=CARTESIAN_POINT('Ctrl Pts',(0.00250834747015757,-0.03198254025128,
-0.0139100359293539));
#39004=CARTESIAN_POINT('Ctrl Pts',(0.00278749957941142,-0.0320116960429182,
-0.0134130827230974));
#39005=CARTESIAN_POINT('Ctrl Pts',(0.00291622471053343,-0.0320408575633779,
-0.012879865671161));
#39006=CARTESIAN_POINT('Ctrl Pts',(0.00297192875716824,-0.032053476814036,
-0.012649123256928));
#39007=CARTESIAN_POINT('Ctrl Pts',(0.00300004532358358,-0.0320660971374776,
-0.0124119508547963));
#39008=CARTESIAN_POINT('Ctrl Pts',(0.00299999994485587,-0.0320787171138616,
-0.0121752780781099));
#39009=CARTESIAN_POINT('Ctrl Pts',(0.00299989497489855,-0.0321079096110824,
-0.0116278072140276));
#39010=CARTESIAN_POINT('Ctrl Pts',(0.00284559654022781,-0.0321371002512389,
-0.0110785818195714));
#39011=CARTESIAN_POINT('Ctrl Pts',(0.00255908040558366,-0.0321662753031713,
-0.0106102519714853));
#39012=CARTESIAN_POINT('Ctrl Pts',(0.002435506461596,-0.0321788584557321,
-0.0104082620678904));
#39013=CARTESIAN_POINT('Ctrl Pts',(0.00228800007691206,-0.032191438708598,
-0.0102211643532271));
#39014=CARTESIAN_POINT('Ctrl Pts',(0.00212101305761234,-0.0322040149601267,
-0.0100542257015569));
#39015=CARTESIAN_POINT('Ctrl Pts',(0.0017339610656569,-0.0322331649097809,
-0.00966728581883857));
#39016=CARTESIAN_POINT('Ctrl Pts',(0.00123668732942299,-0.0322622933624106,
-0.00938805092606279));
#39017=CARTESIAN_POINT('Ctrl Pts',(0.000703123706334418,-0.0322914039985368,
-0.00925941418148655));
#39018=CARTESIAN_POINT('Ctrl Pts',(0.000472760129879772,-0.0323039723783152,
-0.00920387587403498));
#39019=CARTESIAN_POINT('Ctrl Pts',(0.000235991095858931,-0.0323165374370263,
-0.00917583015568731));
#39020=CARTESIAN_POINT('Ctrl Pts',(-2.93864620455047E-7,-0.0323290994708749,
-0.00917585330095084));
#39021=CARTESIAN_POINT('Ctrl Pts',(-0.000545585330011292,-0.0323580897622235,
-0.0091759067149076));
#39022=CARTESIAN_POINT('Ctrl Pts',(-0.00109283713400837,-0.0323870639437451,
-0.00932896737902686));
#39023=CARTESIAN_POINT('Ctrl Pts',(-0.00155994938770585,-0.0324160210225555,
-0.00961332369496386));
#39024=CARTESIAN_POINT('Ctrl Pts',(-0.0017640600889872,-0.0324286741902176,
-0.00973757684096947));
#39025=CARTESIAN_POINT('Ctrl Pts',(-0.00195302566753906,-0.0324413240923474,
-0.00988622107287341));
#39026=CARTESIAN_POINT('Ctrl Pts',(-0.00212142866450282,-0.0324539706461063,
-0.0100546412694731));
#39027=CARTESIAN_POINT('Ctrl Pts',(-0.0025140641651425,-0.0324834563800662,
-0.0104473168714637));
#39028=CARTESIAN_POINT('Ctrl Pts',(-0.00279557634430618,-0.0325129239122803,
-0.0109530147086656));
#39029=CARTESIAN_POINT('Ctrl Pts',(-0.00292190610715409,-0.0325423735927181,
-0.0114958057139754));
#39030=CARTESIAN_POINT('Ctrl Pts',(-0.00297375926539034,-0.0325544614721324,
-0.011718599038787));
#39031=CARTESIAN_POINT('Ctrl Pts',(-0.00300000058860966,-0.0325665463439438,
-0.0119473157627861));
#39032=CARTESIAN_POINT('Ctrl Pts',(-0.00299999999999005,-0.0325786282323535,
-0.0121758610130754));
#39033=CARTESIAN_POINT('',(-0.00299999999995998,-0.0335788169750034,-0.0121758687814435));
#39034=CARTESIAN_POINT('Ctrl Pts',(-0.00299999872723928,-0.0325787743898623,
-0.012178616719692));
#39035=CARTESIAN_POINT('Ctrl Pts',(-0.0029994858324129,-0.0326083191993918,
-0.0127354182603145));
#39036=CARTESIAN_POINT('Ctrl Pts',(-0.0028396594007697,-0.0326378640089213,
-0.0132921917133723));
#39037=CARTESIAN_POINT('Ctrl Pts',(-0.0025448941804952,-0.0326674088184508,
-0.0137644103708587));
#39038=CARTESIAN_POINT('Ctrl Pts',(-0.0024239557840027,-0.032679530675588,
-0.0139581556409997));
#39039=CARTESIAN_POINT('Ctrl Pts',(-0.00228090445082536,-0.0326916525327251,
-0.01413783744446));
#39040=CARTESIAN_POINT('Ctrl Pts',(-0.00211967908184265,-0.0327037743898623,
-0.0142988136229748));
#39041=CARTESIAN_POINT('Ctrl Pts',(-0.00173396026633068,-0.0327327749646866,
-0.0146839362701995));
#39042=CARTESIAN_POINT('Ctrl Pts',(-0.00123868829186396,-0.0327617755395109,
-0.0149623948905047));
#39043=CARTESIAN_POINT('Ctrl Pts',(-0.000707142468841261,-0.0327907761143351,
-0.0150913205782218));
#39044=CARTESIAN_POINT('Ctrl Pts',(-0.000474988166602747,-0.0328034422061775,
-0.0151476292759412));
#39045=CARTESIAN_POINT('Ctrl Pts',(-0.000236285739616681,-0.0328161082980199,
-0.0151760017068329));
#39046=CARTESIAN_POINT('Ctrl Pts',(1.87696153578847E-6,-0.0328287743898623,
-0.0151758526993939));
#39047=CARTESIAN_POINT('Ctrl Pts',(0.000549196391118819,-0.0328578822145917,
-0.0151755102668212));
#39048=CARTESIAN_POINT('Ctrl Pts',(0.00109822958083191,-0.0328869900393211,
-0.0150210560134721));
#39049=CARTESIAN_POINT('Ctrl Pts',(0.00156636682566337,-0.0329160978640505,
-0.01473446520857));
#39050=CARTESIAN_POINT('Ctrl Pts',(0.00176834899772359,-0.0329286567059878,
-0.0146108129379897));
#39051=CARTESIAN_POINT('Ctrl Pts',(0.00195542767052654,-0.032941215547925,
-0.0144632254267738));
#39052=CARTESIAN_POINT('Ctrl Pts',(0.00212233389845239,-0.0329537743898623,
-0.0142961595907226));
#39053=CARTESIAN_POINT('Ctrl Pts',(0.00250910232189599,-0.0329828767400665,
-0.013909021310601));
#39054=CARTESIAN_POINT('Ctrl Pts',(0.00278815368193294,-0.0330119790902707,
-0.0134117190045828));
#39055=CARTESIAN_POINT('Ctrl Pts',(0.00291663000649855,-0.0330410814404749,
-0.0128781846935109));
#39056=CARTESIAN_POINT('Ctrl Pts',(0.00297209690825918,-0.0330536457569373,
-0.0126478426805509));
#39057=CARTESIAN_POINT('Ctrl Pts',(0.00300007783540791,-0.0330662100733998,
-0.0124111062716708));
#39058=CARTESIAN_POINT('Ctrl Pts',(0.00299999983648833,-0.0330787743898623,
-0.0121748627967843));
#39059=CARTESIAN_POINT('Ctrl Pts',(0.00299981916992521,-0.0331078767400665,
-0.0116276591060678));
#39060=CARTESIAN_POINT('Ctrl Pts',(0.00284559023185504,-0.0331369790902707,
-0.0110786774696764));
#39061=CARTESIAN_POINT('Ctrl Pts',(0.00255923810211162,-0.0331660814404748,
-0.0106105097662086));
#39062=CARTESIAN_POINT('Ctrl Pts',(0.00243561170243732,-0.0331786457569373,
-0.0104083883862302));
#39063=CARTESIAN_POINT('Ctrl Pts',(0.00228802265505789,-0.0331912100733998,
-0.0102211743760228));
#39064=CARTESIAN_POINT('Ctrl Pts',(0.00212093334135249,-0.0332037743898623,
-0.010054146011381));
#39065=CARTESIAN_POINT('Ctrl Pts',(0.00173383656040047,-0.0332328822145917,
-0.00966719043147765));
#39066=CARTESIAN_POINT('Ctrl Pts',(0.0012365101137741,-0.0332619900393211,
-0.00938796491070863));
#39067=CARTESIAN_POINT('Ctrl Pts',(0.000702900046714844,-0.0332910978640505,
-0.00925936026850915));
#39068=CARTESIAN_POINT('Ctrl Pts',(0.000472669016033597,-0.0333036567059878,
-0.00920387259848232));
#39069=CARTESIAN_POINT('Ctrl Pts',(0.000236042090910841,-0.033316215547925,
-0.00917584510055194));
#39070=CARTESIAN_POINT('Ctrl Pts',(-1.04017925362034E-7,-0.0333287743898623,
-0.00917585328836139));
#39071=CARTESIAN_POINT('Ctrl Pts',(-0.000545406915514975,-0.0333577749646866,
-0.00917587219545343));
#39072=CARTESIAN_POINT('Ctrl Pts',(-0.00109267735081907,-0.0333867755395109,
-0.00932890439108765));
#39073=CARTESIAN_POINT('Ctrl Pts',(-0.00155981219574908,-0.0334157761143351,
-0.00961324018388489));
#39074=CARTESIAN_POINT('Ctrl Pts',(-0.0017638348016634,-0.0334284422061775,
-0.00973742473151781));
#39075=CARTESIAN_POINT('Ctrl Pts',(-0.00195272767242404,-0.0334411082980199,
-0.00988597836688022));
#39076=CARTESIAN_POINT('Ctrl Pts',(-0.00212108046664552,-0.0334537743898623,
-0.0100542930932063));
#39077=CARTESIAN_POINT('Ctrl Pts',(-0.00251377864860435,-0.0334833191993918,
-0.010446902478342));
#39078=CARTESIAN_POINT('Ctrl Pts',(-0.00279537308278998,-0.0335128640089212,
-0.0109525513711848));
#39079=CARTESIAN_POINT('Ctrl Pts',(-0.00292179270627805,-0.0335424088184507,
-0.0114953186573581));
#39080=CARTESIAN_POINT('Ctrl Pts',(-0.00297366105945631,-0.0335545306755879,
-0.0117180091267337));
#39081=CARTESIAN_POINT('Ctrl Pts',(-0.00299994031444842,-0.0335666525327251,
-0.0119466221991571));
#39082=CARTESIAN_POINT('Ctrl Pts',(-0.00299999989796097,-0.0335787743898623,
-0.0121750708326259));
#39083=CARTESIAN_POINT('',(0.00299999097150563,-0.0340787743898654,-0.0121736669288307));
#39084=CARTESIAN_POINT('Ctrl Pts',(-0.00299999999995998,-0.0335788169750034,
-0.0121758687814435));
#39085=CARTESIAN_POINT('Ctrl Pts',(-0.00299999712337882,-0.0336083693720943,
-0.0127328102029425));
#39086=CARTESIAN_POINT('Ctrl Pts',(-0.00284060331293545,-0.0336379217691852,
-0.013289857790904));
#39087=CARTESIAN_POINT('Ctrl Pts',(-0.00254613224254524,-0.0336674741662761,
-0.0137624252526131));
#39088=CARTESIAN_POINT('Ctrl Pts',(-0.00242545651832797,-0.0336795848870901,
-0.013956085772839));
#39089=CARTESIAN_POINT('Ctrl Pts',(-0.00228269685520116,-0.0336916956079041,
-0.014135728072455));
#39090=CARTESIAN_POINT('Ctrl Pts',(-0.00212177464786208,-0.0337038063287181,
-0.0142967192285002));
#39091=CARTESIAN_POINT('Ctrl Pts',(-0.0017363337691742,-0.033732813927789,
-0.0146823252531321));
#39092=CARTESIAN_POINT('Ctrl Pts',(-0.00124119544968554,-0.0337618215268599,
-0.0149613032246193));
#39093=CARTESIAN_POINT('Ctrl Pts',(-0.000709640673447739,-0.0337908291259308,
-0.0150907135086937));
#39094=CARTESIAN_POINT('Ctrl Pts',(-0.000477732425352501,-0.0338034846447648,
-0.0151471729999951));
#39095=CARTESIAN_POINT('Ctrl Pts',(-0.000239263314320967,-0.0338161401635988,
-0.015175749839925));
#39096=CARTESIAN_POINT('Ctrl Pts',(-1.30059909074996E-6,-0.0338287956824328,
-0.0151758530046318));
#39097=CARTESIAN_POINT('Ctrl Pts',(0.000544131565940404,-0.0338578032815037,
-0.0151760894675133));
#39098=CARTESIAN_POINT('Ctrl Pts',(0.00109159196088156,-0.0338868108805747,
-0.0150232433455221));
#39099=CARTESIAN_POINT('Ctrl Pts',(0.00155893455235758,-0.0339158184796456,
-0.0147390003875778));
#39100=CARTESIAN_POINT('Ctrl Pts',(0.00176282812362129,-0.0339284739984796,
-0.0146149900515654));
#39101=CARTESIAN_POINT('Ctrl Pts',(0.00195162785719649,-0.0339411295173136,
-0.0144666455862975));
#39102=CARTESIAN_POINT('Ctrl Pts',(0.00211993491957889,-0.0339537850361476,
-0.0142985581498752));
#39103=CARTESIAN_POINT('Ctrl Pts',(0.00251295532482384,-0.0339833374332385,
-0.013906050601801));
#39104=CARTESIAN_POINT('Ctrl Pts',(0.00279485478800578,-0.0340128898303293,
-0.0134003999633648));
#39105=CARTESIAN_POINT('Ctrl Pts',(0.00292152123044294,-0.0340424422274202,
-0.0128575524137918));
#39106=CARTESIAN_POINT('Ctrl Pts',(0.00297342977498999,-0.0340545529482342,
-0.012635090760436));
#39107=CARTESIAN_POINT('Ctrl Pts',(0.00299979978310408,-0.0340666636690483,
-0.0124067072854433));
#39108=CARTESIAN_POINT('Ctrl Pts',(0.00299999885881957,-0.0340787743898623,
-0.0121784699793747));
#39109=CARTESIAN_POINT('',(0.00212132034355965,-0.0340787743898723,-0.0142971736301177));
#39110=CARTESIAN_POINT('Origin',(0.,-0.0340787743898623,-0.0121758532865581));
#39111=CARTESIAN_POINT('',(-0.00299989950608398,-0.0337035851790747,-0.0121776595950485));
#39112=CARTESIAN_POINT('Ctrl Pts',(0.00212132034355965,-0.0340787743898623,
-0.0142971736301177));
#39113=CARTESIAN_POINT('Ctrl Pts',(0.0017049242015075,-0.0340475243898623,
-0.0147135697721699));
#39114=CARTESIAN_POINT('Ctrl Pts',(0.000620767042151375,-0.0339850243898623,
-0.0152929740109833));
#39115=CARTESIAN_POINT('Ctrl Pts',(-0.00121534600412802,-0.0338912743898623,
-0.0151128743279742));
#39116=CARTESIAN_POINT('Ctrl Pts',(-0.00264184561203855,-0.0337975243898623,
-0.0139428974550539));
#39117=CARTESIAN_POINT('Ctrl Pts',(-0.00299958575104565,-0.0337350243898623,
-0.012766832826268));
#39118=CARTESIAN_POINT('Ctrl Pts',(-0.00299999926036318,-0.0337037743898623,
-0.0121779599000421));
#39119=CARTESIAN_POINT('',(-0.00299999923775439,-0.0327037743898623,-0.0121737147185652));
#39120=CARTESIAN_POINT('Ctrl Pts',(-0.00299932366121755,-0.0337024929345961,
-0.0121759260444648));
#39121=CARTESIAN_POINT('Ctrl Pts',(-0.00299712296400654,-0.0336720038405544,
-0.0116201236474055));
#39122=CARTESIAN_POINT('Ctrl Pts',(-0.00284134996265265,-0.0336450671877836,
-0.0110636879727134));
#39123=CARTESIAN_POINT('Ctrl Pts',(-0.00254831752635056,-0.0336169910244305,
-0.0105910159029857));
#39124=CARTESIAN_POINT('Ctrl Pts',(-0.00250350847321846,-0.0336126977580901,
-0.0105187372564517));
#39125=CARTESIAN_POINT('Ctrl Pts',(-0.00245567366869795,-0.0336082649481663,
-0.0104483703245496));
#39126=CARTESIAN_POINT('Ctrl Pts',(-0.00240484794115916,-0.033603720390553,
-0.0103802875159579));
#39127=CARTESIAN_POINT('Ctrl Pts',(-0.00231856073827001,-0.0335960050624345,
-0.0102647028425515));
#39128=CARTESIAN_POINT('Ctrl Pts',(-0.00222364272152698,-0.0335879676540423,
-0.0101557057813394));
#39129=CARTESIAN_POINT('Ctrl Pts',(-0.00212163897555336,-0.033579744174801,
-0.0100541729698885));
#39130=CARTESIAN_POINT('Ctrl Pts',(-0.00173486111027858,-0.0335485623812726,
-0.00966918079441987));
#39131=CARTESIAN_POINT('Ctrl Pts',(-0.00123883616658502,-0.0335185292847313,
-0.00939260545203301));
#39132=CARTESIAN_POINT('Ctrl Pts',(-0.000707074316813727,-0.0334910935177513,
-0.00926138600833388));
#39133=CARTESIAN_POINT('Ctrl Pts',(-0.000475778990634066,-0.0334791600466394,
-0.00920431075172313));
#39134=CARTESIAN_POINT('Ctrl Pts',(-0.000237646442315334,-0.033467829772317,
-0.00917515682429721));
#39135=CARTESIAN_POINT('Ctrl Pts',(7.38310283306005E-8,-0.0334557455696987,
-0.00917485485860858));
#39136=CARTESIAN_POINT('Ctrl Pts',(6.96966992447012E-5,-0.033452206381246,
-0.00917476641971757));
#39137=CARTESIAN_POINT('Ctrl Pts',(0.000139279753693056,-0.0334485633437618,
-0.00917707797200307));
#39138=CARTESIAN_POINT('Ctrl Pts',(0.000208683016430185,-0.0334448399147507,
-0.00918190242644719));
#39139=CARTESIAN_POINT('Ctrl Pts',(0.000689586586317118,-0.0334190398264973,
-0.00921533165258783));
#39140=CARTESIAN_POINT('Ctrl Pts',(0.00116359922847722,-0.0333893799231094,
-0.00937025399267345));
#39141=CARTESIAN_POINT('Ctrl Pts',(0.00157475316846205,-0.0333636641845656,
-0.00962402027786571));
#39142=CARTESIAN_POINT('Ctrl Pts',(0.00177265356168317,-0.0333512864489418,
-0.00974616539856592));
#39143=CARTESIAN_POINT('Ctrl Pts',(0.00195640797895683,-0.0333396246142925,
-0.00989103223327693));
#39144=CARTESIAN_POINT('Ctrl Pts',(0.00212100455005177,-0.033328264314852,
-0.0100547923352072));
#39145=CARTESIAN_POINT('Ctrl Pts',(0.00232121948316958,-0.0333144456698003,
-0.0102539897889405));
#39146=CARTESIAN_POINT('Ctrl Pts',(0.00249575585499712,-0.0333000788700998,
-0.0104821170588777));
#39147=CARTESIAN_POINT('Ctrl Pts',(0.00263223344424879,-0.0332850382196607,
-0.010731087603101));
#39148=CARTESIAN_POINT('Ctrl Pts',(0.002746503265138,-0.0332724449987432,
-0.0109395454140213));
#39149=CARTESIAN_POINT('Ctrl Pts',(0.00283411747476242,-0.0332593793841039,
-0.011162518444991));
#39150=CARTESIAN_POINT('Ctrl Pts',(0.00289549840934342,-0.033245767596808,
-0.0113913522361136));
#39151=CARTESIAN_POINT('Ctrl Pts',(0.0029643578013657,-0.0332304973927303,
-0.0116480664070271));
#39152=CARTESIAN_POINT('Ctrl Pts',(0.00299871148338599,-0.0332155634345403,
-0.0119129046483332));
#39153=CARTESIAN_POINT('Ctrl Pts',(0.00299877890744598,-0.0332016648463028,
-0.0121757419432914));
#39154=CARTESIAN_POINT('Ctrl Pts',(0.00299890693696643,-0.0331752732349504,
-0.0126748357806571));
#39155=CARTESIAN_POINT('Ctrl Pts',(0.0028748961594508,-0.033152653571698,
-0.013172493157235));
#39156=CARTESIAN_POINT('Ctrl Pts',(0.00263826635774537,-0.033126523774227,
-0.0136074814841024));
#39157=CARTESIAN_POINT('Ctrl Pts',(0.00258279739963268,-0.0331203986258689,
-0.0137094481388036));
#39158=CARTESIAN_POINT('Ctrl Pts',(0.00252110363446337,-0.0331140805985485,
-0.0138080698342926));
#39159=CARTESIAN_POINT('Ctrl Pts',(0.00245391928001071,-0.0331074758934644,
-0.0139030936547182));
#39160=CARTESIAN_POINT('Ctrl Pts',(0.00236154049408779,-0.0330983943946241,
-0.0140337518300656));
#39161=CARTESIAN_POINT('Ctrl Pts',(0.00225854225119812,-0.0330891010895125,
-0.0141570197667402));
#39162=CARTESIAN_POINT('Ctrl Pts',(0.00214609493720693,-0.0330800644838706,
-0.0142713277699323));
#39163=CARTESIAN_POINT('Ctrl Pts',(0.00176980594943767,-0.0330498247647598,
-0.0146538432902091));
#39164=CARTESIAN_POINT('Ctrl Pts',(0.00128664527240643,-0.0330218468616416,
-0.0149389591782877));
#39165=CARTESIAN_POINT('Ctrl Pts',(0.000761545417184402,-0.0329953331669265,
-0.0150781148955854));
#39166=CARTESIAN_POINT('Ctrl Pts',(0.000585478026924089,-0.0329864430539542,
-0.0151247741809399));
#39167=CARTESIAN_POINT('Ctrl Pts',(0.000404957692717902,-0.0329773611900798,
-0.0151554473731775));
#39168=CARTESIAN_POINT('Ctrl Pts',(0.000223331473602049,-0.0329676888854435,
-0.0151689182329267));
#39169=CARTESIAN_POINT('Ctrl Pts',(0.000164832159414799,-0.032964573568775,
-0.0151732570121));
#39170=CARTESIAN_POINT('Ctrl Pts',(0.000106214754925876,-0.0329613970000329,
-0.0151758161624007));
#39171=CARTESIAN_POINT('Ctrl Pts',(4.75877733928088E-5,-0.032958145857755,
-0.01517667014769));
#39172=CARTESIAN_POINT('Ctrl Pts',(-0.000493648198624367,-0.0329281317737125,
-0.0151845540186668));
#39173=CARTESIAN_POINT('Ctrl Pts',(-0.00103971989257228,-0.0328963193462496,
-0.0150392486864561));
#39174=CARTESIAN_POINT('Ctrl Pts',(-0.00151253595850431,-0.0328681306236198,
-0.0147650753466467));
#39175=CARTESIAN_POINT('Ctrl Pts',(-0.00172418321353248,-0.0328555124699714,
-0.0146423467869516));
#39176=CARTESIAN_POINT('Ctrl Pts',(-0.00192091540781267,-0.0328438008855719,
-0.0144933772495667));
#39177=CARTESIAN_POINT('Ctrl Pts',(-0.00209642903093382,-0.0328317779866714,
-0.0143227737760233));
#39178=CARTESIAN_POINT('Ctrl Pts',(-0.00220478715253754,-0.032824355322163,
-0.0142174470691643));
#39179=CARTESIAN_POINT('Ctrl Pts',(-0.00230563731691904,-0.0328164509163901,
-0.0141041753377086));
#39180=CARTESIAN_POINT('Ctrl Pts',(-0.00239698774693834,-0.0328082565659287,
-0.013983366227865));
#39181=CARTESIAN_POINT('Ctrl Pts',(-0.00263994304948872,-0.0327864628984535,
-0.0136620627175618));
#39182=CARTESIAN_POINT('Ctrl Pts',(-0.00281552462457732,-0.0327626183203804,
-0.0132865952314827));
#39183=CARTESIAN_POINT('Ctrl Pts',(-0.00291196287183983,-0.0327403310118172,
-0.0128924370499046));
#39184=CARTESIAN_POINT('Ctrl Pts',(-0.00296920402740611,-0.0327271023257634,
-0.0126584835052284));
#39185=CARTESIAN_POINT('Ctrl Pts',(-0.00299873369263853,-0.0327144851464306,
-0.0124173715237727));
#39186=CARTESIAN_POINT('Ctrl Pts',(-0.00299918122624294,-0.0327024705208686,
-0.0121759162920882));
#39187=CARTESIAN_POINT('Ctrl Pts',(-0.00299999923775439,-0.0327037743898623,
-0.0121737147185652));
#39188=CARTESIAN_POINT('Ctrl Pts',(-0.002999602319356,-0.0326742337072068,
-0.0116169146090542));
#39189=CARTESIAN_POINT('Ctrl Pts',(-0.002839892690886,-0.0326446930245512,
-0.0110601091576252));
#39190=CARTESIAN_POINT('Ctrl Pts',(-0.00254522722774817,-0.0326151523418957,
-0.0105878298739066));
#39191=CARTESIAN_POINT('Ctrl Pts',(-0.00242429803692082,-0.0326030289976395,
-0.0103940088844481));
#39192=CARTESIAN_POINT('Ctrl Pts',(-0.00228124142308449,-0.0325909056533834,
-0.0102142540931621));
#39193=CARTESIAN_POINT('Ctrl Pts',(-0.0021199985543597,-0.0325787823091272,
-0.0100532119768892));
#39194=CARTESIAN_POINT('Ctrl Pts',(-0.00173434008204576,-0.032549785861333,
-0.00966803366152436));
#39195=CARTESIAN_POINT('Ctrl Pts',(-0.00123911318528987,-0.0325207894135388,
-0.00938950111789259));
#39196=CARTESIAN_POINT('Ctrl Pts',(-0.000707589724350954,-0.0324917929657446,
-0.00926049451241161));
#39197=CARTESIAN_POINT('Ctrl Pts',(-0.000475384885260714,-0.0324791253866271,
-0.00920413583726607));
#39198=CARTESIAN_POINT('Ctrl Pts',(-0.00023662427972223,-0.0324664578075097,
-0.0091757267513867));
#39199=CARTESIAN_POINT('Ctrl Pts',(1.59885239224121E-6,-0.0324537902283922,
-0.00917585371261296));
#39200=CARTESIAN_POINT('Ctrl Pts',(0.000548915156033654,-0.0324246865367518,
-0.00917614540531485));
#39201=CARTESIAN_POINT('Ctrl Pts',(0.00109796015032326,-0.0323955828451114,
-0.00933054705960091));
#39202=CARTESIAN_POINT('Ctrl Pts',(0.00156612260844863,-0.032366479153471,
-0.00961709187225897));
#39203=CARTESIAN_POINT('Ctrl Pts',(0.00176816836635975,-0.0323539188181997,
-0.0097407565592585));
#39204=CARTESIAN_POINT('Ctrl Pts',(0.00195530521981268,-0.0323413584829284,
-0.00988837024876112));
#39205=CARTESIAN_POINT('Ctrl Pts',(0.00212225987648144,-0.0323287981476571,
-0.0100554728922239));
#39206=CARTESIAN_POINT('Ctrl Pts',(0.00250903964605414,-0.0322996999261464,
-0.0104425954991826));
#39207=CARTESIAN_POINT('Ctrl Pts',(0.00278810780862761,-0.0322706017046357,
-0.0109398851664139));
#39208=CARTESIAN_POINT('Ctrl Pts',(0.00291660361119665,-0.032241503483125,
-0.0114734122746897));
#39209=CARTESIAN_POINT('Ctrl Pts',(0.0029720933685116,-0.032228937677724,
-0.0117038111606243));
#39210=CARTESIAN_POINT('Ctrl Pts',(0.00300008323900718,-0.032216371872323,
-0.011940608760253));
#39211=CARTESIAN_POINT('Ctrl Pts',(0.00299999981303822,-0.032203806066922,
-0.0121769124232979));
#39212=CARTESIAN_POINT('Ctrl Pts',(0.00299980662627087,-0.0321747078454113,
-0.0127241130293597));
#39213=CARTESIAN_POINT('Ctrl Pts',(0.00284556678595463,-0.0321456096239006,
-0.0132730886889762));
#39214=CARTESIAN_POINT('Ctrl Pts',(0.00255920646923548,-0.0321165114023899,
-0.0137412485234945));
#39215=CARTESIAN_POINT('Ctrl Pts',(0.00243554434049904,-0.032103945596989,
-0.0139434191398311));
#39216=CARTESIAN_POINT('Ctrl Pts',(0.00228790753192101,-0.032091379791588,
-0.0141306742213337));
#39217=CARTESIAN_POINT('Ctrl Pts',(0.00212076216568075,-0.032078813986187,
-0.0142977316611633));
#39218=CARTESIAN_POINT('Ctrl Pts',(0.00173363638719356,-0.0320497102945466,
-0.0146846537930824));
#39219=CARTESIAN_POINT('Ctrl Pts',(0.00123629038411274,-0.0320206066029062,
-0.0149638386139045));
#39220=CARTESIAN_POINT('Ctrl Pts',(0.000702672738198018,-0.0319915029112658,
-0.0150924010785535));
#39221=CARTESIAN_POINT('Ctrl Pts',(0.00047237836103825,-0.0319789425759945,
-0.0151478850246882));
#39222=CARTESIAN_POINT('Ctrl Pts',(0.000235686941747564,-0.0319663822407232,
-0.0151758941384449));
#39223=CARTESIAN_POINT('Ctrl Pts',(-5.19421053127542E-7,-0.0319538219054519,
-0.0151758532415917));
#39224=CARTESIAN_POINT('Ctrl Pts',(-0.00054581899464477,-0.0319248254576577,
-0.0151757588282307));
#39225=CARTESIAN_POINT('Ctrl Pts',(-0.00109306558886062,-0.0318958290098635,
-0.0150226526353755));
#39226=CARTESIAN_POINT('Ctrl Pts',(-0.00156015962044416,-0.0318668325620693,
-0.0147382548863733));
#39227=CARTESIAN_POINT('Ctrl Pts',(-0.00176421739477506,-0.0318541649829518,
-0.0146140110130586));
#39228=CARTESIAN_POINT('Ctrl Pts',(-0.00195313436141152,-0.0318414974038343,
-0.0144653876112966));
#39229=CARTESIAN_POINT('Ctrl Pts',(-0.00212149680405239,-0.0318288298247168,
-0.014296997154945));
#39230=CARTESIAN_POINT('Ctrl Pts',(-0.00251411653376062,-0.0317992891420613,
-0.0139043120975107));
#39231=CARTESIAN_POINT('Ctrl Pts',(-0.00279561145356866,-0.0317697484594058,
-0.0133986097351527));
#39232=CARTESIAN_POINT('Ctrl Pts',(-0.00292192511681729,-0.0317402077767503,
-0.0128558191766675));
#39233=CARTESIAN_POINT('Ctrl Pts',(-0.00297376359467769,-0.0317280844324941,
-0.0126330607226316));
#39234=CARTESIAN_POINT('Ctrl Pts',(-0.00299999845410164,-0.031715961088238,
-0.0124043815409992));
#39235=CARTESIAN_POINT('Ctrl Pts',(-0.00299999999993135,-0.0317038377439818,
-0.0121758735812085));
#39236=CARTESIAN_POINT('Origin',(0.,-0.0341787743898723,-0.0121758532865581));
#39237=CARTESIAN_POINT('',(0.000999999999999998,-0.0340787743898723,-0.0121758532865581));
#39238=CARTESIAN_POINT('Origin',(0.,-0.0340787743898623,-0.0121758532865581));
#39239=CARTESIAN_POINT('',(0.001200000000005,-0.0342787743898773,-0.0121758532865581));
#39240=CARTESIAN_POINT('',(0.0011,-0.0341787743898723,-0.0121758532865581));
#39241=CARTESIAN_POINT('Origin',(0.,-0.0342787743898723,-0.0121758532865581));
#39242=CARTESIAN_POINT('Origin',(0.,-0.0121787743898723,-0.0121758532865581));
#39243=CARTESIAN_POINT('',(0.001,-0.0181787743898623,-0.0121758532865581));
#39244=CARTESIAN_POINT('Origin',(0.,-0.0181787743898623,-0.0121758532865581));
#39245=CARTESIAN_POINT('',(0.001,-0.0121787743898723,-0.0121758532865581));
#39246=CARTESIAN_POINT('Origin',(0.,-0.0342787743898723,-0.0121758532865581));
#39247=CARTESIAN_POINT('',(-0.002800000000005,-0.0342787743898673,-0.0121758532865581));
#39248=CARTESIAN_POINT('Origin',(0.,-0.0342787743898723,-0.0121758532865581));
#39249=CARTESIAN_POINT('Origin',(0.,-0.0122787743898723,-0.0121758532865581));
#39250=CARTESIAN_POINT('',(0.00210000000001,-0.0123787743898623,-0.0121758532865581));
#39251=CARTESIAN_POINT('Origin',(0.,-0.0123787743898623,-0.0121758532865581));
#39252=CARTESIAN_POINT('',(0.00230000000001,-0.0121787743898623,-0.0121758532865581));
#39253=CARTESIAN_POINT('',(0.0022,-0.0122787743898723,-0.0121758532865581));
#39254=CARTESIAN_POINT('Origin',(0.,-0.0121787743898623,-0.0121758532865581));
#39255=CARTESIAN_POINT('Origin',(0.,-0.0121787743898723,-0.0121758532865581));
#39256=CARTESIAN_POINT('',(0.00255,-0.0121787743898723,-0.0121758532865581));
#39257=CARTESIAN_POINT('Origin',(0.,-0.0121787743898623,-0.0121758532865581));
#39258=CARTESIAN_POINT('Origin',(0.,-0.0121787743898723,-0.0121758532865581));
#39259=CARTESIAN_POINT('',(0.0021,-0.0171787743898623,-0.0121758532865581));
#39260=CARTESIAN_POINT('',(0.0021,-0.0121787743898723,-0.0121758532865581));
#39261=CARTESIAN_POINT('Origin',(0.,-0.0171787743898623,-0.0121758532865581));
#39262=CARTESIAN_POINT('Origin',(0.,-0.0176787743898723,-0.0121758532865581));
#39263=CARTESIAN_POINT('',(0.00155,-0.0176787743898723,-0.0121758532865581));
#39264=CARTESIAN_POINT('Origin',(0.,-0.0122787743898723,-0.0121758532865581));
#39265=CARTESIAN_POINT('',(0.00275,-0.0123787743898723,-0.0121758532865581));
#39266=CARTESIAN_POINT('Origin',(0.,-0.0123787743898623,-0.0121758532865581));
#39267=CARTESIAN_POINT('',(0.00265,-0.0122787743898723,-0.0121758532865581));
#39268=CARTESIAN_POINT('Origin',(0.,-0.0171787743898723,-0.0121758532865581));
#39269=CARTESIAN_POINT('',(0.00275,-0.0171787743898623,-0.0121758532865581));
#39270=CARTESIAN_POINT('',(0.00275,-0.0171787743898723,-0.0121758532865581));
#39271=CARTESIAN_POINT('Origin',(0.,-0.0171787743898623,-0.0121758532865581));
#39272=CARTESIAN_POINT('Origin',(-3.47714923605922E-19,-0.0173787743898723,
-0.0121758532865581));
#39273=CARTESIAN_POINT('',(-0.00268069430974081,-0.0173787743898623,-0.0135226561740599));
#39274=CARTESIAN_POINT('',(0.00300000000001,-0.0173787743898623,-0.0121758532865581));
#39275=CARTESIAN_POINT('Origin',(0.,-0.0173787743898623,-0.0121758532865581));
#39276=CARTESIAN_POINT('Ctrl Pts',(-0.0026806943097408,-0.017378774389871,
-0.0135226561740599));
#39277=CARTESIAN_POINT('Ctrl Pts',(-0.00271392633795641,-0.0173787741749263,
-0.0134352550519111));
#39278=CARTESIAN_POINT('Ctrl Pts',(-0.00274298533440864,-0.0173787743898643,
-0.0133463390881159));
#39279=CARTESIAN_POINT('Ctrl Pts',(-0.00276788023433509,-0.0173787743898644,
-0.0132562475799165));
#39280=CARTESIAN_POINT('Ctrl Pts',(-0.00282788362768599,-0.0173787743898647,
-0.0130391028546903));
#39281=CARTESIAN_POINT('Ctrl Pts',(-0.00286378472390475,-0.0173787743898649,
-0.0128151065976874));
#39282=CARTESIAN_POINT('Ctrl Pts',(-0.00287475302218889,-0.0173787743898652,
-0.0125890170413387));
#39283=CARTESIAN_POINT('Ctrl Pts',(-0.00287554103043115,-0.0173787743898652,
-0.0125727738257299));
#39284=CARTESIAN_POINT('Ctrl Pts',(-0.00287619933294147,-0.0173787743898653,
-0.0125565288873291));
#39285=CARTESIAN_POINT('Ctrl Pts',(-0.00287672773145678,-0.0173787743898653,
-0.0125402876026397));
#39286=CARTESIAN_POINT('Ctrl Pts',(-0.00287991617497516,-0.0173787743898654,
-0.0124422850205016));
#39287=CARTESIAN_POINT('Ctrl Pts',(-0.00287838091164588,-0.0173787743898657,
-0.0123443722698902));
#39288=CARTESIAN_POINT('Ctrl Pts',(-0.00287208727180318,-0.0173787743898654,
-0.0122469392994813));
#39289=CARTESIAN_POINT('Ctrl Pts',(-0.00285958163282609,-0.0173787743898649,
-0.0120533372531536));
#39290=CARTESIAN_POINT('Ctrl Pts',(-0.00282833650432931,-0.0173787743898647,
-0.0118615973081069));
#39291=CARTESIAN_POINT('Ctrl Pts',(-0.00277748993655705,-0.0173787743898645,
-0.0116750173394792));
#39292=CARTESIAN_POINT('Ctrl Pts',(-0.00277235536708658,-0.0173787743898644,
-0.0116561761894727));
#39293=CARTESIAN_POINT('Ctrl Pts',(-0.0027670189588198,-0.0173787743898644,
-0.0116373840454527));
#39294=CARTESIAN_POINT('Ctrl Pts',(-0.00276148764352656,-0.0173787743898644,
-0.0116186713947204));
#39295=CARTESIAN_POINT('Ctrl Pts',(-0.00272061920221593,-0.0173787743898642,
-0.0114804118980766));
#39296=CARTESIAN_POINT('Ctrl Pts',(-0.00266906423161114,-0.0173787743898641,
-0.0113462105835281));
#39297=CARTESIAN_POINT('Ctrl Pts',(-0.00260657226363377,-0.017378774389864,
-0.0112173959288558));
#39298=CARTESIAN_POINT('Ctrl Pts',(-0.00252329114560864,-0.0173787743898639,
-0.0110457286121373));
#39299=CARTESIAN_POINT('Ctrl Pts',(-0.00242059060388749,-0.0173787743898637,
-0.0108835928969429));
#39300=CARTESIAN_POINT('Ctrl Pts',(-0.00230096382390033,-0.0173787743898637,
-0.0107331618622516));
#39301=CARTESIAN_POINT('Ctrl Pts',(-0.00228846353348929,-0.0173787743898637,
-0.0107174427095612));
#39302=CARTESIAN_POINT('Ctrl Pts',(-0.00227577417957042,-0.0173787743898637,
-0.0107018475972849));
#39303=CARTESIAN_POINT('Ctrl Pts',(-0.00226291969158275,-0.0173787743898637,
-0.0106864045911225));
#39304=CARTESIAN_POINT('Ctrl Pts',(-0.0020869743162019,-0.0173787743898636,
-0.0104750289596036));
#39305=CARTESIAN_POINT('Ctrl Pts',(-0.0018796914814688,-0.0173787743898636,
-0.0102910931413629));
#39306=CARTESIAN_POINT('Ctrl Pts',(-0.00164888534756171,-0.0173787743898638,
-0.0101410525216628));
#39307=CARTESIAN_POINT('Ctrl Pts',(-0.00160588295044858,-0.0173787743898638,
-0.010113097864643));
#39308=CARTESIAN_POINT('Ctrl Pts',(-0.00156205963042595,-0.0173787743898638,
-0.010086330500961));
#39309=CARTESIAN_POINT('Ctrl Pts',(-0.00151746195886052,-0.0173787743898638,
-0.0100608079878154));
#39310=CARTESIAN_POINT('Ctrl Pts',(-0.00150248206522892,-0.0173787743898638,
-0.0100522352413308));
#39311=CARTESIAN_POINT('Ctrl Pts',(-0.00148741201804428,-0.0173787743898639,
-0.0100438015756368));
#39312=CARTESIAN_POINT('Ctrl Pts',(-0.00147227556935763,-0.0173787743898639,
-0.0100355210027254));
#39313=CARTESIAN_POINT('Ctrl Pts',(-0.00119042933630068,-0.0173787743898641,
-0.00988133369426643));
#39314=CARTESIAN_POINT('Ctrl Pts',(-0.000884129244039172,-0.0173787743898644,
-0.009778575357405));
#39315=CARTESIAN_POINT('Ctrl Pts',(-0.000565648716062966,-0.0173787743898649,
-0.0097406856270151));
#39316=CARTESIAN_POINT('Ctrl Pts',(0.00249547098945156,-0.017378774389874,
-0.0123517024776432));
#39317=CARTESIAN_POINT('Ctrl Pts',(0.0025025789150578,-0.0173787743898744,
-0.0125930835426984));
#39318=CARTESIAN_POINT('Ctrl Pts',(0.0024739241321343,-0.0173787743898748,
-0.0128349355184667));
#39319=CARTESIAN_POINT('Ctrl Pts',(0.00241344648103719,-0.0173787743898751,
-0.0130700286939032));
#39320=CARTESIAN_POINT('Ctrl Pts',(0.00240775502746633,-0.0173787743898751,
-0.0130921529310148));
#39321=CARTESIAN_POINT('Ctrl Pts',(0.00240177958578699,-0.0173787743898751,
-0.0131142177455514));
#39322=CARTESIAN_POINT('Ctrl Pts',(0.00239552211903118,-0.0173787743898751,
-0.0131362172550705));
#39323=CARTESIAN_POINT('Ctrl Pts',(0.0023872874601568,-0.0173787743898752,
-0.0131651680211493));
#39324=CARTESIAN_POINT('Ctrl Pts',(0.00237856046135632,-0.0173787743898752,
-0.0131940169394221));
#39325=CARTESIAN_POINT('Ctrl Pts',(0.00236936612861886,-0.0173787743898752,
-0.0132226879746876));
#39326=CARTESIAN_POINT('Ctrl Pts',(0.00228485698784404,-0.0173787743898755,
-0.0134862160223009));
#39327=CARTESIAN_POINT('Ctrl Pts',(0.00216102083655063,-0.0173787743898758,
-0.013735547013867));
#39328=CARTESIAN_POINT('Ctrl Pts',(0.00200195343303136,-0.0173787743898758,
-0.0139605028246134));
#39329=CARTESIAN_POINT('Ctrl Pts',(0.00199374263882198,-0.0173787743898758,
-0.01397211466857));
#39330=CARTESIAN_POINT('Ctrl Pts',(0.00198544255492749,-0.0173787743898758,
-0.0139836535663112));
#39331=CARTESIAN_POINT('Ctrl Pts',(0.00197705447952352,-0.0173787743898758,
-0.0139951174266605));
#39332=CARTESIAN_POINT('Ctrl Pts',(0.00189574251367433,-0.0173787743898759,
-0.0141062453047889));
#39333=CARTESIAN_POINT('Ctrl Pts',(0.00180616371909361,-0.0173787743898759,
-0.0142103508031204));
#39334=CARTESIAN_POINT('Ctrl Pts',(0.00170885054614273,-0.0173787743898759,
-0.0143062456970463));
#39335=CARTESIAN_POINT('Ctrl Pts',(0.00157900085243143,-0.0173787743898759,
-0.014434202912161));
#39336=CARTESIAN_POINT('Ctrl Pts',(0.00143540122347535,-0.0173787743898759,
-0.01454757649909));
#39337=CARTESIAN_POINT('Ctrl Pts',(0.00128084268067104,-0.0173787743898758,
-0.014646071767013));
#39338=CARTESIAN_POINT('Ctrl Pts',(0.0012664895905635,-0.0173787743898758,
-0.0146552185370977));
#39339=CARTESIAN_POINT('Ctrl Pts',(0.00125204156802668,-0.0173787743898758,
-0.0146642365899005));
#39340=CARTESIAN_POINT('Ctrl Pts',(0.00123750060782707,-0.0173787743898757,
-0.0146731254295959));
#39341=CARTESIAN_POINT('Ctrl Pts',(0.0012250706672739,-0.0173787743898757,
-0.014680723810135));
#39342=CARTESIAN_POINT('Ctrl Pts',(0.00121258012573586,-0.0173787743898757,
-0.0146882232766687));
#39343=CARTESIAN_POINT('Ctrl Pts',(0.00120003402569006,-0.0173787743898757,
-0.0146956217909455));
#39344=CARTESIAN_POINT('Ctrl Pts',(0.000904617897650414,-0.0173787743898755,
-0.0148698305437002));
#39345=CARTESIAN_POINT('Ctrl Pts',(0.000578281544735326,-0.0173787743898752,
-0.0149889800424757));
#39346=CARTESIAN_POINT('Ctrl Pts',(0.000238503122206503,-0.0173787743898748,
-0.0150506991599622));
#39347=CARTESIAN_POINT('Ctrl Pts',(0.000218843683908667,-0.0173787743898748,
-0.0150542702024463));
#39348=CARTESIAN_POINT('Ctrl Pts',(0.000199132992020951,-0.0173787743898748,
-0.0150576477208599));
#39349=CARTESIAN_POINT('Ctrl Pts',(0.000179404432188849,-0.0173787743898747,
-0.0150608259170612));
#39350=CARTESIAN_POINT('Ctrl Pts',(8.08486648710589E-5,-0.0173787743898746,
-0.0150767028775679));
#39351=CARTESIAN_POINT('Ctrl Pts',(-1.82764467995728E-5,-0.0173787743898737,
-0.0150876344329206));
#39352=CARTESIAN_POINT('Ctrl Pts',(-0.00011755903599944,-0.0173787743898738,
-0.0150935879009351));
#39353=CARTESIAN_POINT('Ctrl Pts',(-0.000314661884901832,-0.0173787743898741,
-0.015105407148559));
#39354=CARTESIAN_POINT('Ctrl Pts',(-0.000512377756271194,-0.0173787743898745,
-0.0150976565743765));
#39355=CARTESIAN_POINT('Ctrl Pts',(-0.000707721724771412,-0.0173787743898747,
-0.0150695266038167));
#39356=CARTESIAN_POINT('Ctrl Pts',(-0.000781218199492438,-0.0173787743898748,
-0.0150589429462509));
#39357=CARTESIAN_POINT('Ctrl Pts',(-0.000854380568763212,-0.0173787743898749,
-0.0150454663912922));
#39358=CARTESIAN_POINT('Ctrl Pts',(-0.00092705098312487,-0.0173787743898723,
-0.0150290228354436));
#39359=CARTESIAN_POINT('Origin',(0.,-0.0173787743898623,-0.0121758532865581));
#39360=CARTESIAN_POINT('Ctrl Pts',(-0.00176576417784588,-0.0274694134009467,
-0.0104108140867378));
#39361=CARTESIAN_POINT('Ctrl Pts',(-0.00118292095981484,-0.0274168573249058,
-0.0098277128924115));
#39362=CARTESIAN_POINT('Ctrl Pts',(0.00059527173215891,-0.0273117560658722,
-0.00929359972128072));
#39363=CARTESIAN_POINT('Ctrl Pts',(0.00274092821966559,-0.0271541096238461,
-0.011096746535157));
#39364=CARTESIAN_POINT('Ctrl Pts',(0.00240319207333727,-0.0269964740748679,
-0.0138747749556991));
#39365=CARTESIAN_POINT('Ctrl Pts',(-0.000101975422128609,-0.02683883852589,
-0.015117915947344));
#39366=CARTESIAN_POINT('Ctrl Pts',(-0.0025168541262501,-0.0266812029769119,
-0.0137033259019318));
#39367=CARTESIAN_POINT('Ctrl Pts',(-0.00265711008968434,-0.0265235674279339,
-0.0109088159045253));
#39368=CARTESIAN_POINT('Ctrl Pts',(-0.000397484020939204,-0.0263659318789558,
-0.00925893793215084));
#39369=CARTESIAN_POINT('Ctrl Pts',(0.00222147717336516,-0.0262082963299777,
-0.0102441291704481));
#39370=CARTESIAN_POINT('Ctrl Pts',(0.00283347043813024,-0.0260506607809997,
-0.0129744031307677));
#39371=CARTESIAN_POINT('Ctrl Pts',(0.000885836877589451,-0.0258930252320217,
-0.014983281882999));
#39372=CARTESIAN_POINT('Ctrl Pts',(-0.00186207862087175,-0.0257353896830436,
-0.0144559914602417));
#39373=CARTESIAN_POINT('Ctrl Pts',(-0.00292781373092146,-0.0255777541340656,
-0.0118688726936714));
#39374=CARTESIAN_POINT('Ctrl Pts',(-0.00134863475409321,-0.0254201185850875,
-0.00955907392664864));
#39375=CARTESIAN_POINT('Ctrl Pts',(0.00144887683555256,-0.0252624830361095,
-0.00961321703853231));
#39376=CARTESIAN_POINT('Ctrl Pts',(0.00293750170311061,-0.0251048474871315,
-0.0119823905855329));
#39377=CARTESIAN_POINT('Ctrl Pts',(0.00177245222274447,-0.0249472119381534,
-0.0145263341168514));
#39378=CARTESIAN_POINT('Ctrl Pts',(-0.000993793093215091,-0.0247895763891753,
-0.0149469039637085));
#39379=CARTESIAN_POINT('Ctrl Pts',(-0.00286226678504763,-0.0246319408401973,
-0.0128641663544265));
#39380=CARTESIAN_POINT('Ctrl Pts',(-0.00214503055983681,-0.0244743052912193,
-0.0101596215653044));
#39381=CARTESIAN_POINT('Ctrl Pts',(0.000509980129524932,-0.0243166697422412,
-0.00927649704326958));
#39382=CARTESIAN_POINT('Ctrl Pts',(0.00270428571248687,-0.0241590341932632,
-0.0110125884483945));
#39383=CARTESIAN_POINT('Ctrl Pts',(0.00245559790913657,-0.0240013986442851,
-0.0137995482294608));
#39384=CARTESIAN_POINT('Ctrl Pts',(-1.14241210114808E-5,-0.0238437630953071,
-0.0151196970035421));
#39385=CARTESIAN_POINT('Ctrl Pts',(-0.00246812583927738,-0.0236861275463291,
-0.0137804408273949));
#39386=CARTESIAN_POINT('Ctrl Pts',(-0.00269517588644093,-0.023528491997351,
-0.0109916348590015));
#39387=CARTESIAN_POINT('Ctrl Pts',(-0.000487462138964281,-0.023370856448373,
-0.00927262628838117));
#39388=CARTESIAN_POINT('Ctrl Pts',(0.00216061439503312,-0.0232132208993949,
-0.0101763303996177));
#39389=CARTESIAN_POINT('Ctrl Pts',(0.00285683846403066,-0.0230555853504169,
-0.0128863603807944));
#39390=CARTESIAN_POINT('Ctrl Pts',(0.000972256252628799,-0.0228979498014388,
-0.0149545335702968));
#39391=CARTESIAN_POINT('Ctrl Pts',(-0.00179064129716749,-0.0227403142524608,
-0.0145125068947971));
#39392=CARTESIAN_POINT('Ctrl Pts',(-0.00293591210216717,-0.0225826787034828,
-0.0119595977236454));
#39393=CARTESIAN_POINT('Ctrl Pts',(-0.00142894320700064,-0.0224250431545047,
-0.00960204916595687));
#39394=CARTESIAN_POINT('Ctrl Pts',(0.0013689021759258,-0.0222674076055267,
-0.0095696197642336));
#39395=CARTESIAN_POINT('Ctrl Pts',(0.00293011084416917,-0.0221097720565486,
-0.0118916055409205));
#39396=CARTESIAN_POINT('Ctrl Pts',(0.00184432054372579,-0.0219521365075706,
-0.014470374603087));
#39397=CARTESIAN_POINT('Ctrl Pts',(-0.000907589175775288,-0.0217945009585925,
-0.0149763225737564));
#39398=CARTESIAN_POINT('Ctrl Pts',(-0.00283960239971302,-0.0216368654096145,
-0.0129523869632051));
#39399=CARTESIAN_POINT('Ctrl Pts',(-0.00220638003274556,-0.0214792298606364,
-0.010226947570273));
#39400=CARTESIAN_POINT('Ctrl Pts',(0.000420038490802218,-0.0213215943116584,
-0.00926210758570121));
#39401=CARTESIAN_POINT('Ctrl Pts',(0.00266700329593708,-0.0211639587626804,
-0.0109294826538095));
#39402=CARTESIAN_POINT('Ctrl Pts',(0.00250465482140347,-0.0210063232137023,
-0.0137228020789193));
#39403=CARTESIAN_POINT('Ctrl Pts',(7.96551729982372E-5,-0.0208486876647243,
-0.0151186413204434));
#39404=CARTESIAN_POINT('Ctrl Pts',(-0.00241730323367411,-0.0206910521157462,
-0.0138560292817851));
#39405=CARTESIAN_POINT('Ctrl Pts',(-0.00273052202674609,-0.0205334165667682,
-0.0110755824928619));
#39406=CARTESIAN_POINT('Ctrl Pts',(-0.000577046057097934,-0.0203757810177901,
-0.00928909657626689));
#39407=CARTESIAN_POINT('Ctrl Pts',(0.00209772082487443,-0.0202181454688121,
-0.0101104445209445));
#39408=CARTESIAN_POINT('Ctrl Pts',(0.00287745204370962,-0.020060509919834,
-0.0127976380592968));
#39409=CARTESIAN_POINT('Ctrl Pts',(0.0010577549130369,-0.019902874370856,
-0.0149231249439365));
#39410=CARTESIAN_POINT('Ctrl Pts',(-0.00171749480653482,-0.019745238821878,
-0.0145667852517114));
#39411=CARTESIAN_POINT('Ctrl Pts',(-0.00294119750658452,-0.0195876032728999,
-0.0120505302976156));
#39412=CARTESIAN_POINT('Ctrl Pts',(-0.00150788431839104,-0.0194299677239219,
-0.0096474872527832));
#39413=CARTESIAN_POINT('Ctrl Pts',(0.00128761623108036,-0.0192723321749438,
-0.00952851976604358));
#39414=CARTESIAN_POINT('Ctrl Pts',(0.00291991747238735,-0.0191146966259658,
-0.0118010882457072));
#39415=CARTESIAN_POINT('Ctrl Pts',(0.00191441775473846,-0.0189570610769877,
-0.0144122269043048));
#39416=CARTESIAN_POINT('Ctrl Pts',(-0.000820505555265474,-0.0187994255280097,
-0.0150030439789635));
#39417=CARTESIAN_POINT('Ctrl Pts',(-0.00281424058814684,-0.0186417899790317,
-0.0130398954178051));
#39418=CARTESIAN_POINT('Ctrl Pts',(-0.00226557676094723,-0.0184841544300536,
-0.0102960791852537));
#39419=CARTESIAN_POINT('Ctrl Pts',(0.000329616729494906,-0.0183265188810756,
-0.00925062328400989));
#39420=CARTESIAN_POINT('Ctrl Pts',(0.00262731783985433,-0.0181688833320975,
-0.0108473472640193));
#39421=CARTESIAN_POINT('Ctrl Pts',(0.00255102483355773,-0.0180112477831195,
-0.0136450040566565));
#39422=CARTESIAN_POINT('Ctrl Pts',(0.000171215685035621,-0.0178536122341414,
-0.0151139397673183));
#39423=CARTESIAN_POINT('Ctrl Pts',(-0.00236524911441394,-0.0176959766851634,
-0.0139316310381663));
#39424=CARTESIAN_POINT('Ctrl Pts',(-0.00276110049454826,-0.0175383326154246,
-0.0111570598155219));
#39425=CARTESIAN_POINT('Ctrl Pts',(-0.00136756358585242,-0.0174332337286785,
-0.00993024457820385));
#39426=CARTESIAN_POINT('Ctrl Pts',(-0.000564501289899483,-0.017380680024925,
-0.00974385311997074));
#39427=CARTESIAN_POINT('Ctrl Pts',(-0.00188620817627642,-0.0273710914741913,
-0.0102904195395609));
#39428=CARTESIAN_POINT('Ctrl Pts',(-0.00126360881837204,-0.0273185353981504,
-0.00966754460861935));
#39429=CARTESIAN_POINT('Ctrl Pts',(0.000635875629595165,-0.0272134341391169,
-0.00909699920788931));
#39430=CARTESIAN_POINT('Ctrl Pts',(0.00292788883327953,-0.0270557876970907,
-0.01102313991571));
#39431=CARTESIAN_POINT('Ctrl Pts',(0.00256711547032362,-0.0268981521481127,
-0.013990659580282));
#39432=CARTESIAN_POINT('Ctrl Pts',(-0.000108931236351646,-0.0267405165991346,
-0.0153185960805941));
#39433=CARTESIAN_POINT('Ctrl Pts',(-0.00268853049064535,-0.0265828810501566,
-0.0138075158677251));
#39434=CARTESIAN_POINT('Ctrl Pts',(-0.00283835341055753,-0.0264252455011785,
-0.0108223904065071));
#39435=CARTESIAN_POINT('Ctrl Pts',(-0.000424596681505571,-0.0262676099522004,
-0.00905997311409863));
#39436=CARTESIAN_POINT('Ctrl Pts',(0.00237300567107693,-0.0261099744032224,
-0.010112364929601));
#39437=CARTESIAN_POINT('Ctrl Pts',(0.00302674342060714,-0.0259523388542444,
-0.0130288727691199));
#39438=CARTESIAN_POINT('Ctrl Pts',(0.000946260424987647,-0.0257947033052664,
-0.0151747785334045));
#39439=CARTESIAN_POINT('Ctrl Pts',(-0.00198909229421707,-0.0256370677562883,
-0.0146115212654435));
#39440=CARTESIAN_POINT('Ctrl Pts',(-0.00312752193478945,-0.0254794322073103,
-0.0118479333346609));
#39441=CARTESIAN_POINT('Ctrl Pts',(-0.00144062606541516,-0.0253217966583322,
-0.00938058159280683));
#39442=CARTESIAN_POINT('Ctrl Pts',(0.0015477057287291,-0.0251641611093541,
-0.00943841784387892));
#39443=CARTESIAN_POINT('Ctrl Pts',(0.0031378707302764,-0.0250065255603761,
-0.0119691943606062));
#39444=CARTESIAN_POINT('Ctrl Pts',(0.00189335241735305,-0.0248488900113981,
-0.0146866620434152));
#39445=CARTESIAN_POINT('Ctrl Pts',(-0.00106158040890607,-0.02469125446242,
-0.0151359192510257));
#39446=CARTESIAN_POINT('Ctrl Pts',(-0.00305750398630663,-0.024533618913442,
-0.012911116665859));
#39447=CARTESIAN_POINT('Ctrl Pts',(-0.00229134458105431,-0.024375983364464,
-0.0100220930021377));
#39448=CARTESIAN_POINT('Ctrl Pts',(0.000544766227629503,-0.0242183478154859,
-0.00907872994435708));
#39449=CARTESIAN_POINT('Ctrl Pts',(0.00288874691528906,-0.0240607122665079,
-0.0109332413475189));
#39450=CARTESIAN_POINT('Ctrl Pts',(0.00262309594450553,-0.0239030767175298,
-0.0139103015869071));
#39451=CARTESIAN_POINT('Ctrl Pts',(-1.22033682237757E-5,-0.0237454411685518,
-0.0153204986238699));
#39452=CARTESIAN_POINT('Ctrl Pts',(-0.00263647841344439,-0.0235878056195737,
-0.0138898908557028));
#39453=CARTESIAN_POINT('Ctrl Pts',(-0.00287901570169447,-0.0234301700705957,
-0.0109108584992703));
#39454=CARTESIAN_POINT('Ctrl Pts',(-0.000520712269325407,-0.0232725345216176,
-0.00907459516259491));
#39455=CARTESIAN_POINT('Ctrl Pts',(0.00230799140045058,-0.0231148989726396,
-0.0100399415576206));
#39456=CARTESIAN_POINT('Ctrl Pts',(0.00305170539575071,-0.0229572634236615,
-0.0129348245621481));
#39457=CARTESIAN_POINT('Ctrl Pts',(0.00103857452549612,-0.0227996278746835,
-0.0151440692783674));
#39458=CARTESIAN_POINT('Ctrl Pts',(-0.0019127821811494,-0.0226419923257055,
-0.014671891656961));
#39459=CARTESIAN_POINT('Ctrl Pts',(-0.00313617270155084,-0.0224843567767274,
-0.0119448467818114));
#39460=CARTESIAN_POINT('Ctrl Pts',(-0.00152641241355761,-0.0223267212277494,
-0.00942648820297463));
#39461=CARTESIAN_POINT('Ctrl Pts',(0.00146227594213839,-0.0221690856787713,
-0.00939184676928282));
#39462=CARTESIAN_POINT('Ctrl Pts',(0.0031299757357239,-0.0220114501297933,
-0.011872216805177));
#39463=CARTESIAN_POINT('Ctrl Pts',(0.0019701229263208,-0.0218538145808152,
-0.0146268854924312));
#39464=CARTESIAN_POINT('Ctrl Pts',(-0.000969496462509344,-0.0216961790318372,
-0.0151673445248549));
#39465=CARTESIAN_POINT('Ctrl Pts',(-0.00303329364753954,-0.0215385434828592,
-0.0130053548635084));
#39466=CARTESIAN_POINT('Ctrl Pts',(-0.00235687874403178,-0.0213809079338811,
-0.0100940113605692));
#39467=CARTESIAN_POINT('Ctrl Pts',(0.000448689607390529,-0.0212232723849031,
-0.00906335897191456));
#39468=CARTESIAN_POINT('Ctrl Pts',(0.00284892143926579,-0.021065636835925,
-0.0108444668490842));
#39469=CARTESIAN_POINT('Ctrl Pts',(0.00267549906275975,-0.020908001286947,
-0.0138283205282439));
#39470=CARTESIAN_POINT('Ctrl Pts',(8.50885075578431E-5,-0.0207503657379689,
-0.0153193709318953));
#39471=CARTESIAN_POINT('Ctrl Pts',(-0.00258218916268753,-0.0205927301889909,
-0.0139706352509576));
#39472=CARTESIAN_POINT('Ctrl Pts',(-0.00291677282672843,-0.0204350946400128,
-0.0110005322594209));
#39473=CARTESIAN_POINT('Ctrl Pts',(-0.000616406768606,-0.0202774590910348,
-0.00909218890023294));
#39474=CARTESIAN_POINT('Ctrl Pts',(0.00224080781627953,-0.0201198235420567,
-0.00996956155749723));
#39475=CARTESIAN_POINT('Ctrl Pts',(0.00307372504198695,-0.0199621879930787,
-0.0128400504296073));
#39476=CARTESIAN_POINT('Ctrl Pts',(0.00112990510879018,-0.0198045524441007,
-0.0151105182478334));
#39477=CARTESIAN_POINT('Ctrl Pts',(-0.00183464631769248,-0.0196469168951226,
-0.0147298723782209));
#39478=CARTESIAN_POINT('Ctrl Pts',(-0.00314181862706683,-0.0194892813461446,
-0.012041981929678));
#39479=CARTESIAN_POINT('Ctrl Pts',(-0.0016107381528704,-0.0193316457971665,
-0.00947502565319674));
#39480=CARTESIAN_POINT('Ctrl Pts',(0.00137544542665535,-0.0191740102481885,
-0.00934794331172965));
#39481=CARTESIAN_POINT('Ctrl Pts',(0.00311908706698777,-0.0190163746992104,
-0.0117755252625193));
#39482=CARTESIAN_POINT('Ctrl Pts',(0.00204500151668136,-0.0188587391502324,
-0.0145647714988127));
#39483=CARTESIAN_POINT('Ctrl Pts',(-0.000876472807886479,-0.0187011036012544,
-0.015195888615632));
#39484=CARTESIAN_POINT('Ctrl Pts',(-0.00300620188922807,-0.0185434680522763,
-0.0130988323304493));
#39485=CARTESIAN_POINT('Ctrl Pts',(-0.00242011332209363,-0.0183858325032983,
-0.0101678584909233));
#39486=CARTESIAN_POINT('Ctrl Pts',(0.000352100115072687,-0.0182281969543202,
-0.00905109131804506));
#39487=CARTESIAN_POINT('Ctrl Pts',(0.00280652901071745,-0.0180705614053422,
-0.010756728947428));
#39488=CARTESIAN_POINT('Ctrl Pts',(0.00272503200558233,-0.0179129258563641,
-0.0137452158489603));
#39489=CARTESIAN_POINT('Ctrl Pts',(0.000182894425582328,-0.0177552903073861,
-0.0153143486825729));
#39490=CARTESIAN_POINT('Ctrl Pts',(-0.00252658439587369,-0.017597654758408,
-0.0140513938555416));
#39491=CARTESIAN_POINT('Ctrl Pts',(-0.00294943707301346,-0.0174400106886692,
-0.0110875672067319));
#39492=CARTESIAN_POINT('Ctrl Pts',(-0.00146084604590834,-0.0173349118019229,
-0.0097770700517648));
#39493=CARTESIAN_POINT('Ctrl Pts',(-0.000603006314142103,-0.0172823580981696,
-0.00957796470297678));
#39494=CARTESIAN_POINT('Ctrl Pts',(-0.00200665217470697,-0.0272727695474359,
-0.010170024992384));
#39495=CARTESIAN_POINT('Ctrl Pts',(-0.00134429667692924,-0.0272202134713949,
-0.00950737632482718));
#39496=CARTESIAN_POINT('Ctrl Pts',(0.000676479527031423,-0.0271151122123614,
-0.00890039869449788));
#39497=CARTESIAN_POINT('Ctrl Pts',(0.00311484944689349,-0.0269574657703352,
-0.0109495332962628));
#39498=CARTESIAN_POINT('Ctrl Pts',(0.00273103886730998,-0.0267998302213571,
-0.0141065442048648));
#39499=CARTESIAN_POINT('Ctrl Pts',(-0.000115887050574685,-0.026642194672379,
-0.0155192762138441));
#39500=CARTESIAN_POINT('Ctrl Pts',(-0.00286020685504059,-0.026484559123401,
-0.0139117058335183));
#39501=CARTESIAN_POINT('Ctrl Pts',(-0.00301959673143072,-0.026326923574423,
-0.0107359649084888));
#39502=CARTESIAN_POINT('Ctrl Pts',(-0.000451709342071937,-0.026169288025445,
-0.00886100829604641));
#39503=CARTESIAN_POINT('Ctrl Pts',(0.00252453416878869,-0.0260116524764669,
-0.00998060068875387));
#39504=CARTESIAN_POINT('Ctrl Pts',(0.00322001640308403,-0.0258540169274889,
-0.0130833424074723));
#39505=CARTESIAN_POINT('Ctrl Pts',(0.00100668397238585,-0.0256963813785108,
-0.01536627518381));
#39506=CARTESIAN_POINT('Ctrl Pts',(-0.00211610596756238,-0.0255387458295328,
-0.0147670510706451));
#39507=CARTESIAN_POINT('Ctrl Pts',(-0.00332723013865741,-0.0253811102805547,
-0.0118269939756503));
#39508=CARTESIAN_POINT('Ctrl Pts',(-0.00153261737673712,-0.0252234747315767,
-0.00920208925896502));
#39509=CARTESIAN_POINT('Ctrl Pts',(0.00164653462190566,-0.0250658391825986,
-0.00926361864922554));
#39510=CARTESIAN_POINT('Ctrl Pts',(0.00333823975744216,-0.0249082036336206,
-0.0119559981356793));
#39511=CARTESIAN_POINT('Ctrl Pts',(0.00201425261196165,-0.0247505680846425,
-0.0148469899699792));
#39512=CARTESIAN_POINT('Ctrl Pts',(-0.00112936772459704,-0.0245929325356645,
-0.0153249345383428));
#39513=CARTESIAN_POINT('Ctrl Pts',(-0.00325274118756563,-0.0244352969866865,
-0.0129580669772913));
#39514=CARTESIAN_POINT('Ctrl Pts',(-0.00243765860227181,-0.0242776614377084,
-0.00988456443897111));
#39515=CARTESIAN_POINT('Ctrl Pts',(0.000579552325734072,-0.0241200258887304,
-0.00888096284544458));
#39516=CARTESIAN_POINT('Ctrl Pts',(0.00307320811809126,-0.0239623903397523,
-0.0108538942466433));
#39517=CARTESIAN_POINT('Ctrl Pts',(0.00279059397987449,-0.0238047547907743,
-0.0140210549443533));
#39518=CARTESIAN_POINT('Ctrl Pts',(-1.29826154360689E-5,-0.0236471192417962,
-0.0155213002441977));
#39519=CARTESIAN_POINT('Ctrl Pts',(-0.00280483098761143,-0.0234894836928182,
-0.0139993408840106));
#39520=CARTESIAN_POINT('Ctrl Pts',(-0.00306285551694802,-0.0233318481438402,
-0.0108300821395392));
#39521=CARTESIAN_POINT('Ctrl Pts',(-0.000553962399686529,-0.0231742125948621,
-0.00887656403680862));
#39522=CARTESIAN_POINT('Ctrl Pts',(0.00245536840586803,-0.0230165770458841,
-0.0099035527156234));
#39523=CARTESIAN_POINT('Ctrl Pts',(0.00324657232747075,-0.022858941496906,
-0.0129832887435019));
#39524=CARTESIAN_POINT('Ctrl Pts',(0.00110489279836343,-0.022701305947928,
-0.0153336049864378));
#39525=CARTESIAN_POINT('Ctrl Pts',(-0.0020349230651313,-0.0225436703989499,
-0.0148312764191248));
#39526=CARTESIAN_POINT('Ctrl Pts',(-0.00333643330093449,-0.0223860348499719,
-0.0119300958399773));
#39527=CARTESIAN_POINT('Ctrl Pts',(-0.00162388162011455,-0.0222283993009938,
-0.00925092723999238));
#39528=CARTESIAN_POINT('Ctrl Pts',(0.00155564970835097,-0.0220707637520158,
-0.00921407377433204));
#39529=CARTESIAN_POINT('Ctrl Pts',(0.00332984062727863,-0.0219131282030377,
-0.0118528280694337));
#39530=CARTESIAN_POINT('Ctrl Pts',(0.0020959253089158,-0.0217554926540597,
-0.0147833963817754));
#39531=CARTESIAN_POINT('Ctrl Pts',(-0.0010314037492434,-0.0215978571050817,
-0.0153583664759535));
#39532=CARTESIAN_POINT('Ctrl Pts',(-0.00322698489536608,-0.0214402215561036,
-0.0130583227638117));
#39533=CARTESIAN_POINT('Ctrl Pts',(-0.002507377455318,-0.0212825860071256,
-0.00996107515086551));
#39534=CARTESIAN_POINT('Ctrl Pts',(0.000477340723978841,-0.0211249504581475,
-0.00886461035812792));
#39535=CARTESIAN_POINT('Ctrl Pts',(0.0030308395825945,-0.0209673149091695,
-0.0107594510443588));
#39536=CARTESIAN_POINT('Ctrl Pts',(0.00284634330411602,-0.0208096793601914,
-0.0139338389775685));
#39537=CARTESIAN_POINT('Ctrl Pts',(9.0521842117449E-5,-0.0206520438112134,
-0.0155201005433471));
#39538=CARTESIAN_POINT('Ctrl Pts',(-0.00274707509170096,-0.0204944082622354,
-0.0140852412201302));
#39539=CARTESIAN_POINT('Ctrl Pts',(-0.00310302362671076,-0.0203367727132573,
-0.0109254820259798));
#39540=CARTESIAN_POINT('Ctrl Pts',(-0.000655767480114067,-0.0201791371642793,
-0.00889528122419899));
#39541=CARTESIAN_POINT('Ctrl Pts',(0.00238389480768462,-0.0200215016153012,
-0.00982867859404995));
#39542=CARTESIAN_POINT('Ctrl Pts',(0.00326999804026427,-0.0198638660663232,
-0.0128824627999178));
#39543=CARTESIAN_POINT('Ctrl Pts',(0.00120205530454347,-0.0197062305173451,
-0.0152979115517304));
#39544=CARTESIAN_POINT('Ctrl Pts',(-0.00195179782885014,-0.0195485949683671,
-0.0148929595047305));
#39545=CARTESIAN_POINT('Ctrl Pts',(-0.00334243974754914,-0.019390959419389,
-0.0120334335617402));
#39546=CARTESIAN_POINT('Ctrl Pts',(-0.00171359198734975,-0.019233323870411,
-0.00930256405361027));
#39547=CARTESIAN_POINT('Ctrl Pts',(0.00146327462223035,-0.0190756883214329,
-0.00916736685741573));
#39548=CARTESIAN_POINT('Ctrl Pts',(0.00331825666158819,-0.0189180527724549,
-0.0117499622793314));
#39549=CARTESIAN_POINT('Ctrl Pts',(0.00217558527862425,-0.0187604172234769,
-0.0147173160933204));
#39550=CARTESIAN_POINT('Ctrl Pts',(-0.000932440060507479,-0.0186027816744988,
-0.0153887332523004));
#39551=CARTESIAN_POINT('Ctrl Pts',(-0.00319816319030928,-0.0184451461255208,
-0.0131577692430934));
#39552=CARTESIAN_POINT('Ctrl Pts',(-0.00257464988324002,-0.0182875105765427,
-0.0100396377965929));
#39553=CARTESIAN_POINT('Ctrl Pts',(0.000374583500650467,-0.0181298750275647,
-0.00885155935208023));
#39554=CARTESIAN_POINT('Ctrl Pts',(0.00298574018158057,-0.0179722394785867,
-0.0106661106308367));
#39555=CARTESIAN_POINT('Ctrl Pts',(0.00289903917760691,-0.0178146039296086,
-0.0138454276412644));
#39556=CARTESIAN_POINT('Ctrl Pts',(0.000194573166129036,-0.0176569683806306,
-0.0155147575978273));
#39557=CARTESIAN_POINT('Ctrl Pts',(-0.00268791967733341,-0.0174993328316525,
-0.0141711566729167));
#39558=CARTESIAN_POINT('Ctrl Pts',(-0.00313777365147868,-0.0173416887619137,
-0.0110180745979418));
#39559=CARTESIAN_POINT('Ctrl Pts',(-0.00155412850596426,-0.0172365898751676,
-0.00962389552532573));
#39560=CARTESIAN_POINT('Ctrl Pts',(-0.000641511338384723,-0.0171840361714141,
-0.00941207628598281));
#39561=CARTESIAN_POINT('Ctrl Pts',(-0.0021270961731375,-0.0271744476206803,
-0.010049630445207));
#39562=CARTESIAN_POINT('Ctrl Pts',(-0.00142498453548643,-0.0271218915446394,
-0.00934720804103501));
#39563=CARTESIAN_POINT('Ctrl Pts',(0.000717083424467678,-0.0270167902856059,
-0.00870379818110647));
#39564=CARTESIAN_POINT('Ctrl Pts',(0.00330181006050744,-0.0268591438435796,
-0.0108759266768156));
#39565=CARTESIAN_POINT('Ctrl Pts',(0.00289496226429633,-0.0267015082946015,
-0.0142224288294477));
#39566=CARTESIAN_POINT('Ctrl Pts',(-0.000122842864797722,-0.0265438727456235,
-0.0157199563470941));
#39567=CARTESIAN_POINT('Ctrl Pts',(-0.00303188321943583,-0.0263862371966456,
-0.0140158957993116));
#39568=CARTESIAN_POINT('Ctrl Pts',(-0.00320084005230392,-0.0262286016476674,
-0.0106495394104707));
#39569=CARTESIAN_POINT('Ctrl Pts',(-0.000478822002638301,-0.0260709660986895,
-0.0086620434779942));
#39570=CARTESIAN_POINT('Ctrl Pts',(0.00267606266650046,-0.0259133305497115,
-0.0098488364479067));
#39571=CARTESIAN_POINT('Ctrl Pts',(0.00341328938556092,-0.0257556950007333,
-0.0131378120458245));
#39572=CARTESIAN_POINT('Ctrl Pts',(0.00106710751978404,-0.0255980594517554,
-0.0155577718342156));
#39573=CARTESIAN_POINT('Ctrl Pts',(-0.0022431196409077,-0.0254404239027772,
-0.0149225808758469));
#39574=CARTESIAN_POINT('Ctrl Pts',(-0.00352693834252537,-0.0252827883537992,
-0.0118060546166399));
#39575=CARTESIAN_POINT('Ctrl Pts',(-0.00162460868805907,-0.0251251528048211,
-0.00902359692512321));
#39576=CARTESIAN_POINT('Ctrl Pts',(0.0017453635150822,-0.0249675172558432,
-0.00908881945457216));
#39577=CARTESIAN_POINT('Ctrl Pts',(0.00353860878460794,-0.024809881706865,
-0.0119428019107525));
#39578=CARTESIAN_POINT('Ctrl Pts',(0.00213515280657024,-0.024652246157887,
-0.015007317896543));
#39579=CARTESIAN_POINT('Ctrl Pts',(-0.00119715504028801,-0.0244946106089089,
-0.0155139498256597));
#39580=CARTESIAN_POINT('Ctrl Pts',(-0.00344797838882464,-0.0243369750599309,
-0.0130050172887238));
#39581=CARTESIAN_POINT('Ctrl Pts',(-0.00258397262348931,-0.0241793395109529,
-0.00974703587580447));
#39582=CARTESIAN_POINT('Ctrl Pts',(0.000614338423838643,-0.0240217039619748,
-0.00868319574653206));
#39583=CARTESIAN_POINT('Ctrl Pts',(0.00325766932089345,-0.0238640684129969,
-0.0107745471457676));
#39584=CARTESIAN_POINT('Ctrl Pts',(0.00295809201524345,-0.0237064328640187,
-0.0141318083017995));
#39585=CARTESIAN_POINT('Ctrl Pts',(-1.37618626483643E-5,-0.0235487973150408,
-0.0157221018645255));
#39586=CARTESIAN_POINT('Ctrl Pts',(-0.00297318356177844,-0.0233911617660626,
-0.0141087909123184));
#39587=CARTESIAN_POINT('Ctrl Pts',(-0.00324669533220156,-0.0232335262170846,
-0.010749305779808));
#39588=CARTESIAN_POINT('Ctrl Pts',(-0.000587212530047655,-0.0230758906681066,
-0.00867853291102234));
#39589=CARTESIAN_POINT('Ctrl Pts',(0.00260274541128548,-0.0229182551191285,
-0.00976716387362624));
#39590=CARTESIAN_POINT('Ctrl Pts',(0.0034414392591908,-0.0227606195701505,
-0.0130317529248556));
#39591=CARTESIAN_POINT('Ctrl Pts',(0.00117121107123076,-0.0226029840211724,
-0.0155231406945085));
#39592=CARTESIAN_POINT('Ctrl Pts',(-0.0021570639491132,-0.0224453484721945,
-0.0149906611812887));
#39593=CARTESIAN_POINT('Ctrl Pts',(-0.00353669390031815,-0.0222877129232163,
-0.0119153448981433));
#39594=CARTESIAN_POINT('Ctrl Pts',(-0.0017213508266715,-0.0221300773742383,
-0.00907536627701014));
#39595=CARTESIAN_POINT('Ctrl Pts',(0.00164902347456355,-0.0219724418252602,
-0.00903630077938126));
#39596=CARTESIAN_POINT('Ctrl Pts',(0.00352970551883337,-0.0218148062762822,
-0.0118334393336902));
#39597=CARTESIAN_POINT('Ctrl Pts',(0.00222172769151081,-0.0216571707273041,
-0.0149399072711196));
#39598=CARTESIAN_POINT('Ctrl Pts',(-0.00109331103597745,-0.0214995351783261,
-0.015549388427052));
#39599=CARTESIAN_POINT('Ctrl Pts',(-0.00342067614319262,-0.0213418996293481,
-0.013111290664115));
#39600=CARTESIAN_POINT('Ctrl Pts',(-0.00265787616660422,-0.02118426408037,
-0.00982813894116177));
#39601=CARTESIAN_POINT('Ctrl Pts',(0.000505991840567147,-0.021026628531392,
-0.00866586174434128));
#39602=CARTESIAN_POINT('Ctrl Pts',(0.00321275772592322,-0.020868992982414,
-0.0106744352396337));
#39603=CARTESIAN_POINT('Ctrl Pts',(0.00301718754547228,-0.020711357433436,
-0.0140393574268932));
#39604=CARTESIAN_POINT('Ctrl Pts',(9.59551766770587E-5,-0.0205537218844579,
-0.0157208301547992));
#39605=CARTESIAN_POINT('Ctrl Pts',(-0.00291196102071441,-0.0203960863354798,
-0.0141998471893027));
#39606=CARTESIAN_POINT('Ctrl Pts',(-0.00328927442669309,-0.0202384507865018,
-0.010850431792539));
#39607=CARTESIAN_POINT('Ctrl Pts',(-0.000695128191622135,-0.0200808152375237,
-0.00869837354816502));
#39608=CARTESIAN_POINT('Ctrl Pts',(0.00252698179908972,-0.0199231796885458,
-0.00968779563060266));
#39609=CARTESIAN_POINT('Ctrl Pts',(0.00346627103854158,-0.0197655441395676,
-0.0129248751702283));
#39610=CARTESIAN_POINT('Ctrl Pts',(0.00127420550029675,-0.0196079085905897,
-0.0154853048556274));
#39611=CARTESIAN_POINT('Ctrl Pts',(-0.0020689493400078,-0.0194502730416115,
-0.0150560466312401));
#39612=CARTESIAN_POINT('Ctrl Pts',(-0.00354306086803145,-0.0192926374926335,
-0.0120248851938025));
#39613=CARTESIAN_POINT('Ctrl Pts',(-0.00181644582182911,-0.0191350019436555,
-0.00913010245402381));
#39614=CARTESIAN_POINT('Ctrl Pts',(0.00155110381780535,-0.0189773663946774,
-0.0089867904031018));
#39615=CARTESIAN_POINT('Ctrl Pts',(0.0035174262561886,-0.0188197308456995,
-0.0117243992961435));
#39616=CARTESIAN_POINT('Ctrl Pts',(0.00230616904056715,-0.0186620952967213,
-0.0148698606878284));
#39617=CARTESIAN_POINT('Ctrl Pts',(-0.000988407313128485,-0.0185044597477434,
-0.0155815778889689));
#39618=CARTESIAN_POINT('Ctrl Pts',(-0.0033901244913905,-0.0183468241987653,
-0.0132167061557375));
#39619=CARTESIAN_POINT('Ctrl Pts',(-0.00272918644438642,-0.0181891886497872,
-0.00991141710226236));
#39620=CARTESIAN_POINT('Ctrl Pts',(0.000397066886228245,-0.0180315531008093,
-0.0086520273861154));
#39621=CARTESIAN_POINT('Ctrl Pts',(0.00316495135244369,-0.0178739175518311,
-0.0105754923142454));
#39622=CARTESIAN_POINT('Ctrl Pts',(0.00307304634963151,-0.0177162820028532,
-0.0139456394335682));
#39623=CARTESIAN_POINT('Ctrl Pts',(0.000206251906675747,-0.0175586464538751,
-0.0157151665130819));
#39624=CARTESIAN_POINT('Ctrl Pts',(-0.00284925495879315,-0.017401010904897,
-0.014290919490292));
#39625=CARTESIAN_POINT('Ctrl Pts',(-0.00332611022994388,-0.0172433668351582,
-0.0109485819891518));
#39626=CARTESIAN_POINT('Ctrl Pts',(-0.00164741096602017,-0.0171382679484121,
-0.00947072099888669));
#39627=CARTESIAN_POINT('Ctrl Pts',(-0.000680016362627343,-0.0170857142446586,
-0.00924618786898885));
#39628=CARTESIAN_POINT('Ctrl Pts',(-0.00267260870462009,-0.0173794995011935,
-0.0135402263681242));
#39629=CARTESIAN_POINT('Ctrl Pts',(-0.00267396311369304,-0.0173793789565635,
-0.0135373081584126));
#39630=CARTESIAN_POINT('Ctrl Pts',(-0.00267531279930547,-0.0173792583760944,
-0.0135343877591632));
#39631=CARTESIAN_POINT('Ctrl Pts',(-0.00267800804240615,-0.0173790166708016,
-0.0135285310334481));
#39632=CARTESIAN_POINT('Ctrl Pts',(-0.00267935356128369,-0.0173788955458108,
-0.0135255946920731));
#39633=CARTESIAN_POINT('Ctrl Pts',(-0.00268069430973449,-0.0173787743898751,
-0.0135226561740565));
#39634=CARTESIAN_POINT('Ctrl Pts',(0.00214364697154644,-0.027178774389864,
-0.0108862500897033));
#39635=CARTESIAN_POINT('Ctrl Pts',(0.00200718019753922,-0.0271787743898637,
-0.0105977254813795));
#39636=CARTESIAN_POINT('Ctrl Pts',(0.00181515016014682,-0.0271787743898637,
-0.0103370893624455));
#39637=CARTESIAN_POINT('Ctrl Pts',(0.0015825829649816,-0.0271787743898636,
-0.0101151998101994));
#39638=CARTESIAN_POINT('Ctrl Pts',(0.00156807204491965,-0.0271787743898636,
-0.0101013551166134));
#39639=CARTESIAN_POINT('Ctrl Pts',(0.00155339606635249,-0.0271787743898636,
-0.0100876582609352));
#39640=CARTESIAN_POINT('Ctrl Pts',(0.00153858322606208,-0.0271787743898636,
-0.0100741352287478));
#39641=CARTESIAN_POINT('Ctrl Pts',(0.00130703486088774,-0.0271787743898636,
-0.00986274862538259));
#39642=CARTESIAN_POINT('Ctrl Pts',(0.00104161596381899,-0.0271787743898638,
-0.00969262022738725));
#39643=CARTESIAN_POINT('Ctrl Pts',(0.000754106682302279,-0.0271787743898641,
-0.00957416699352214));
#39644=CARTESIAN_POINT('Ctrl Pts',(0.000721077701908584,-0.0271787743898641,
-0.00956055912139272));
#39645=CARTESIAN_POINT('Ctrl Pts',(0.00068773017489579,-0.0271787743898642,
-0.00954763097757543));
#39646=CARTESIAN_POINT('Ctrl Pts',(0.000654172404124864,-0.0271787743898642,
-0.00953543584602603));
#39647=CARTESIAN_POINT('Ctrl Pts',(0.000621454371281899,-0.0271787743898643,
-0.00952354588118656));
#39648=CARTESIAN_POINT('Ctrl Pts',(0.000588531611466588,-0.0271787743898643,
-0.00951234954431439));
#39649=CARTESIAN_POINT('Ctrl Pts',(0.000555420931463722,-0.0271787743898643,
-0.00950185931133918));
#39650=CARTESIAN_POINT('Ctrl Pts',(0.00038258051039096,-0.0271787743898646,
-0.00944709944882868));
#39651=CARTESIAN_POINT('Ctrl Pts',(0.000204654649537397,-0.0271787743898647,
-0.00941152019527573));
#39652=CARTESIAN_POINT('Ctrl Pts',(2.43336311719498E-5,-0.0271787743898655,
-0.00939382593790338));
#39653=CARTESIAN_POINT('Ctrl Pts',(-7.0449357939566E-5,-0.0271787743898659,
-0.00938452522177465));
#39654=CARTESIAN_POINT('Ctrl Pts',(-0.000165901707066126,-0.0271787743898656,
-0.00938017829844935));
#39655=CARTESIAN_POINT('Ctrl Pts',(-0.000261664269848712,-0.0271787743898654,
-0.00938067795709841));
#39656=CARTESIAN_POINT('Ctrl Pts',(-0.000283370180679184,-0.0271787743898654,
-0.00938079121164974));
#39657=CARTESIAN_POINT('Ctrl Pts',(-0.000305092069150565,-0.0271787743898653,
-0.00938115369090413));
#39658=CARTESIAN_POINT('Ctrl Pts',(-0.000326825803069745,-0.0271787743898653,
-0.00938176453997136));
#39659=CARTESIAN_POINT('Ctrl Pts',(-0.000345831109748606,-0.0271787743898653,
-0.00938229870376947));
#39660=CARTESIAN_POINT('Ctrl Pts',(-0.000364849161917403,-0.0271787743898653,
-0.00938302307415796));
#39661=CARTESIAN_POINT('Ctrl Pts',(-0.000383850544190616,-0.0271787743898652,
-0.00938393558023816));
#39662=CARTESIAN_POINT('Ctrl Pts',(-0.0006742994320196,-0.0271787743898648,
-0.00939788384843884));
#39663=CARTESIAN_POINT('Ctrl Pts',(-0.000961964432259771,-0.0271787743898645,
-0.00945545867279974));
#39664=CARTESIAN_POINT('Ctrl Pts',(-0.00123688275642929,-0.0271787743898642,
-0.00955336079145493));
#39665=CARTESIAN_POINT('Ctrl Pts',(-0.00125242205520696,-0.0271787743898642,
-0.00955889454507919));
#39666=CARTESIAN_POINT('Ctrl Pts',(-0.00126792259952857,-0.0271787743898642,
-0.00956455895934887));
#39667=CARTESIAN_POINT('Ctrl Pts',(-0.00128337643900455,-0.0271787743898642,
-0.00957035152521633));
#39668=CARTESIAN_POINT('Ctrl Pts',(-0.00156303926269199,-0.0271787743898639,
-0.00967517759963037));
#39669=CARTESIAN_POINT('Ctrl Pts',(-0.00182522482013095,-0.0271787743898638,
-0.00982078890803008));
#39670=CARTESIAN_POINT('Ctrl Pts',(-0.0020595896027101,-0.0271787743898637,
-0.0100046652555036));
#39671=CARTESIAN_POINT('Ctrl Pts',(-0.00208038902733874,-0.0271787743898637,
-0.010020983928421));
#39672=CARTESIAN_POINT('Ctrl Pts',(-0.00210096855971851,-0.0271787743898637,
-0.0100376065791357));
#39673=CARTESIAN_POINT('Ctrl Pts',(-0.00212132034355959,-0.0271787743898723,
-0.0100545329429984));
#39674=CARTESIAN_POINT('Ctrl Pts',(0.000734447700009759,-0.027496347211233,
-0.0151361043823298));
#39675=CARTESIAN_POINT('Ctrl Pts',(-0.000243069169262639,-0.0274437919704715,
-0.0153786446838308));
#39676=CARTESIAN_POINT('Ctrl Pts',(-0.0024403684665538,-0.0273386915467173,
-0.0148161659350916));
#39677=CARTESIAN_POINT('Ctrl Pts',(-0.00354831004413418,-0.0271810459399706,
-0.0115765056537264));
#39678=CARTESIAN_POINT('Ctrl Pts',(-0.00144312695496411,-0.0270234103909925,
-0.00888283623912904));
#39679=CARTESIAN_POINT('Ctrl Pts',(0.00196194337287167,-0.0268657748420145,
-0.00916187994792398));
#39680=CARTESIAN_POINT('Ctrl Pts',(0.00359659766777445,-0.0267081392930364,
-0.0121647738576856));
#39681=CARTESIAN_POINT('Ctrl Pts',(0.00198114537143259,-0.0265505037440584,
-0.0151771107943776));
#39682=CARTESIAN_POINT('Ctrl Pts',(-0.00142350210994787,-0.0263928681950803,
-0.0154784703644144));
#39683=CARTESIAN_POINT('Ctrl Pts',(-0.00354246332004805,-0.0262352326461021,
-0.0127961640919714));
#39684=CARTESIAN_POINT('Ctrl Pts',(-0.00246109668429956,-0.0260775970971242,
-0.00955356181364477));
#39685=CARTESIAN_POINT('Ctrl Pts',(0.000843497391267268,-0.025919961548146,
-0.00867983985000952));
#39686=CARTESIAN_POINT('Ctrl Pts',(0.00338613269875458,-0.0257623259991681,
-0.0109643625076157));
#39687=CARTESIAN_POINT('Ctrl Pts',(0.00286978866718684,-0.0256046904501901,
-0.0143433086683626));
#39688=CARTESIAN_POINT('Ctrl Pts',(-0.000239050153610035,-0.025447054901212,
-0.0157642281583879));
#39689=CARTESIAN_POINT('Ctrl Pts',(-0.00313194163772321,-0.025289419352234,
-0.0139434841362084));
#39690=CARTESIAN_POINT('Ctrl Pts',(-0.00319550174896822,-0.025131783803256,
-0.0105259020768301));
#39691=CARTESIAN_POINT('Ctrl Pts',(-0.000372315933265614,-0.0249741482542779,
-0.00859884955669905));
#39692=CARTESIAN_POINT('Ctrl Pts',(0.00278721283092204,-0.0248165127052998,
-0.00990318551528194));
#39693=CARTESIAN_POINT('Ctrl Pts',(0.00342883321548304,-0.0246588771563218,
-0.0132606003240156));
#39694=CARTESIAN_POINT('Ctrl Pts',(0.00097291979816731,-0.0245012416073438,
-0.0156380781585438));
#39695=CARTESIAN_POINT('Ctrl Pts',(-0.00236190849724789,-0.0243436060583657,
-0.0148878566236573));
#39696=CARTESIAN_POINT('Ctrl Pts',(-0.00356303951920687,-0.0241859705093877,
-0.0116876697707944));
#39697=CARTESIAN_POINT('Ctrl Pts',(-0.00154539748107324,-0.0240283349604096,
-0.00892849736567574));
#39698=CARTESIAN_POINT('Ctrl Pts',(0.00186832334048244,-0.0238706994114316,
-0.00910291630068922));
#39699=CARTESIAN_POINT('Ctrl Pts',(0.003594241126128,-0.0237130638624535,
-0.0120533602574297));
#39700=CARTESIAN_POINT('Ctrl Pts',(0.00207319896783111,-0.0235554283134755,
-0.0151144617782086));
#39701=CARTESIAN_POINT('Ctrl Pts',(-0.00132072644568367,-0.0233977927644975,
-0.0155208877375533));
#39702=CARTESIAN_POINT('Ctrl Pts',(-0.00352153605955123,-0.0232401572155194,
-0.0129054816873811));
#39703=CARTESIAN_POINT('Ctrl Pts',(-0.00254106591574783,-0.0230825216665414,
-0.0096309450690597));
#39704=CARTESIAN_POINT('Ctrl Pts',(0.000734948395842858,-0.0229248861175633,
-0.00865542367096509));
#39705=CARTESIAN_POINT('Ctrl Pts',(0.00334702617063905,-0.0227672505685853,
-0.0108601824934037));
#39706=CARTESIAN_POINT('Ctrl Pts',(0.00293547265879514,-0.0226096150196073,
-0.0142534899469383));
#39707=CARTESIAN_POINT('Ctrl Pts',(-0.000127923569543504,-0.0224519794706292,
-0.0157699052315523));
#39708=CARTESIAN_POINT('Ctrl Pts',(-0.00307575640295856,-0.0222943439216512,
-0.014039531470352));
#39709=CARTESIAN_POINT('Ctrl Pts',(-0.00324501720966393,-0.0221367083726731,
-0.0106255510154228));
#39710=CARTESIAN_POINT('Ctrl Pts',(-0.000482799425948263,-0.0219790728236951,
-0.0086120802105612));
#39711=CARTESIAN_POINT('Ctrl Pts',(0.00271556895104147,-0.021821437274717,
-0.00981804517396586));
#39712=CARTESIAN_POINT('Ctrl Pts',(0.00346075088011901,-0.021663801725739,
-0.0131540031563442));
#39713=CARTESIAN_POINT('Ctrl Pts',(0.00107956507222703,-0.0215061661767609,
-0.0156063216332275));
#39714=CARTESIAN_POINT('Ctrl Pts',(-0.00227687654957576,-0.0213485306277829,
-0.014959628960963));
#39715=CARTESIAN_POINT('Ctrl Pts',(-0.00357643697965559,-0.0211908950788049,
-0.0117981333566007));
#39716=CARTESIAN_POINT('Ctrl Pts',(-0.00164512134804076,-0.0210332595298268,
-0.00897786179596077));
#39717=CARTESIAN_POINT('Ctrl Pts',(0.0017723614516327,-0.0208756239808488,
-0.00904658680123543));
#39718=CARTESIAN_POINT('Ctrl Pts',(0.00358873110925933,-0.0207179884318707,
-0.011942223695265));
#39719=CARTESIAN_POINT('Ctrl Pts',(0.00216311847927169,-0.0205603528828927,
-0.0150489165114876));
#39720=CARTESIAN_POINT('Ctrl Pts',(-0.0012166088095401,-0.0204027173339146,
-0.0155601459752024));
#39721=CARTESIAN_POINT('Ctrl Pts',(-0.003497277816922,-0.0202450817849366,
-0.0130140783316013));
#39722=CARTESIAN_POINT('Ctrl Pts',(-0.00261858165263156,-0.0200874462359586,
-0.0097107763522708));
#39723=CARTESIAN_POINT('Ctrl Pts',(0.000625685134828339,-0.0199298106869805,
-0.00863437154163214));
#39724=CARTESIAN_POINT('Ctrl Pts',(0.00330472067115259,-0.0197721751380025,
-0.0107572653591462));
#39725=CARTESIAN_POINT('Ctrl Pts',(0.00299834431493395,-0.0196145395890244,
-0.014161680220569));
#39726=CARTESIAN_POINT('Ctrl Pts',(-1.6674577032454E-5,-0.0194569040400464,
-0.0157721432019016));
#39727=CARTESIAN_POINT('Ctrl Pts',(-0.00301662439656255,-0.0192992684910683,
-0.0141337927842166));
#39728=CARTESIAN_POINT('Ctrl Pts',(-0.00329143158006377,-0.0191416329420903,
-0.0107266870729041));
#39729=CARTESIAN_POINT('Ctrl Pts',(-0.00059280963165573,-0.0189839973931122,
-0.00862871718285146));
#39730=CARTESIAN_POINT('Ctrl Pts',(0.00264130373978803,-0.0188263618441342,
-0.00973517223149046));
#39731=CARTESIAN_POINT('Ctrl Pts',(0.00348939724868163,-0.0186687262951562,
-0.013046450041716));
#39732=CARTESIAN_POINT('Ctrl Pts',(0.00118509637283412,-0.0185110907461781,
-0.0155713185576321));
#39733=CARTESIAN_POINT('Ctrl Pts',(-0.00218951000492656,-0.0183534551972001,
-0.0150286641021081));
#39734=CARTESIAN_POINT('Ctrl Pts',(-0.00358670864122049,-0.018195819648222,
-0.0119090974795379));
#39735=CARTESIAN_POINT('Ctrl Pts',(-0.00174269656258942,-0.018038184099244,
-0.00903002020530739));
#39736=CARTESIAN_POINT('Ctrl Pts',(0.00167359605724419,-0.0178805485502659,
-0.00899377017639597));
#39737=CARTESIAN_POINT('Ctrl Pts',(0.00358194225358649,-0.0177229130012879,
-0.0118302936733849));
#39738=CARTESIAN_POINT('Ctrl Pts',(0.0022464705553738,-0.0175652666528983,
-0.0149830002760419));
#39739=CARTESIAN_POINT('Ctrl Pts',(1.47162903616745E-5,-0.0174601654875016,
-0.0153878269104618));
#39740=CARTESIAN_POINT('Ctrl Pts',(-0.000943092295784545,-0.0174076095050974,
-0.0150763837366195));
#39741=CARTESIAN_POINT('Ctrl Pts',(0.000690033766136825,-0.0273898599693712,
-0.0149570904152181));
#39742=CARTESIAN_POINT('Ctrl Pts',(-0.000228370153920869,-0.0273373047286097,
-0.0151849636833654));
#39743=CARTESIAN_POINT('Ctrl Pts',(-0.00229279313382739,-0.0272322043048555,
-0.0146564994654789));
#39744=CARTESIAN_POINT('Ctrl Pts',(-0.00333373464596939,-0.0270745586981087,
-0.0116127497404478));
#39745=CARTESIAN_POINT('Ctrl Pts',(-0.00135585737110244,-0.0269169231491307,
-0.00908197341579252));
#39746=CARTESIAN_POINT('Ctrl Pts',(0.00184329963115394,-0.0267592876001526,
-0.00934414263668327));
#39747=CARTESIAN_POINT('Ctrl Pts',(0.00337910219330849,-0.0266016520511746,
-0.0121654438591319));
#39748=CARTESIAN_POINT('Ctrl Pts',(0.00186134043567162,-0.0264440165021965,
-0.0149956170644823));
#39749=CARTESIAN_POINT('Ctrl Pts',(-0.00133741929073781,-0.0262863809532184,
-0.0152787526493183));
#39750=CARTESIAN_POINT('Ctrl Pts',(-0.00332824148826644,-0.0261287454042405,
-0.0127586523085022));
#39751=CARTESIAN_POINT('Ctrl Pts',(-0.00231226786314605,-0.0259711098552624,
-0.00971213849660252));
#39752=CARTESIAN_POINT('Ctrl Pts',(0.000792488943208649,-0.0258134743062844,
-0.00889125273834406));
#39753=CARTESIAN_POINT('Ctrl Pts',(0.00318136458011873,-0.0256558387573063,
-0.011037624458525));
#39754=CARTESIAN_POINT('Ctrl Pts',(0.00269624519487149,-0.0254982032083283,
-0.0142122370889994));
#39755=CARTESIAN_POINT('Ctrl Pts',(-0.00022459417844039,-0.0253405676593502,
-0.0155472299374572));
#39756=CARTESIAN_POINT('Ctrl Pts',(-0.00294254510371564,-0.0251829321103721,
-0.0138365909705451));
#39757=CARTESIAN_POINT('Ctrl Pts',(-0.00300226157221008,-0.0250252965613941,
-0.0106256788532042));
#39758=CARTESIAN_POINT('Ctrl Pts',(-0.000349801035009846,-0.024867661012416,
-0.00881516013554496));
#39759=CARTESIAN_POINT('Ctrl Pts',(0.00261866293096226,-0.024710025463438,
-0.0100406195573617));
#39760=CARTESIAN_POINT('Ctrl Pts',(0.00322148288721361,-0.02455238991446,
-0.0131950028918365));
#39761=CARTESIAN_POINT('Ctrl Pts',(0.000914084845618756,-0.024394754365482,
-0.0154287085512653));
#39762=CARTESIAN_POINT('Ctrl Pts',(-0.00221907783985831,-0.0242371188165039,
-0.0147238548344551));
#39763=CARTESIAN_POINT('Ctrl Pts',(-0.00334757339195157,-0.0240794832675258,
-0.0117171914785847));
#39764=CARTESIAN_POINT('Ctrl Pts',(-0.00145194333650873,-0.0239218477185478,
-0.00912487329704566));
#39765=CARTESIAN_POINT('Ctrl Pts',(0.00175534104195211,-0.0237642121695698,
-0.00928874467224547));
#39766=CARTESIAN_POINT('Ctrl Pts',(0.00337688815777223,-0.0236065766205917,
-0.0120607677246945));
#39767=CARTESIAN_POINT('Ctrl Pts',(0.00194782731527988,-0.0234489410716137,
-0.0149367565948105));
#39768=CARTESIAN_POINT('Ctrl Pts',(-0.00124085873417469,-0.0232913055226356,
-0.0153186049352418));
#39769=CARTESIAN_POINT('Ctrl Pts',(-0.00330857975282177,-0.0231336699736576,
-0.0128613591888756));
#39770=CARTESIAN_POINT('Ctrl Pts',(-0.00238740115030942,-0.0229760344246795,
-0.00978484218832786));
#39771=CARTESIAN_POINT('Ctrl Pts',(0.00069050418361027,-0.0228183988757015,
-0.00886831306819399));
#39772=CARTESIAN_POINT('Ctrl Pts',(0.00314462292393853,-0.0226607633267235,
-0.0109397444766531));
#39773=CARTESIAN_POINT('Ctrl Pts',(0.00275795710724289,-0.0225031277777454,
-0.0141278499357506));
#39774=CARTESIAN_POINT('Ctrl Pts',(-0.000120187703588163,-0.0223454922287674,
-0.0155525637034643));
#39775=CARTESIAN_POINT('Ctrl Pts',(-0.00288975753402832,-0.0221878566797893,
-0.0139268300763462));
#39776=CARTESIAN_POINT('Ctrl Pts',(-0.00304878270615251,-0.0220302211308113,
-0.0107193017652071));
#39777=CARTESIAN_POINT('Ctrl Pts',(-0.0004536033078616,-0.0218725855818332,
-0.00882759069787478));
#39778=CARTESIAN_POINT('Ctrl Pts',(0.00255135154003003,-0.0217149500328552,
-0.00996062787059126));
#39779=CARTESIAN_POINT('Ctrl Pts',(0.00325147040890474,-0.0215573144838771,
-0.0130948519279668));
#39780=CARTESIAN_POINT('Ctrl Pts',(0.00101428100676018,-0.0213996789348991,
-0.0153988724243863));
#39781=CARTESIAN_POINT('Ctrl Pts',(-0.00213918799189042,-0.0212420433859211,
-0.0147912869146629));
#39782=CARTESIAN_POINT('Ctrl Pts',(-0.00336016067364632,-0.021084407836943,
-0.01182097504838));
#39783=CARTESIAN_POINT('Ctrl Pts',(-0.00154563664577557,-0.020926772287965,
-0.00917125253377325));
#39784=CARTESIAN_POINT('Ctrl Pts',(0.00166518221434912,-0.0207691367389869,
-0.00923582156192436));
#39785=CARTESIAN_POINT('Ctrl Pts',(0.00337171134573875,-0.0206115011900089,
-0.0119563518751454));
#39786=CARTESIAN_POINT('Ctrl Pts',(0.00203230916351456,-0.0204538656410308,
-0.014875175018277));
#39787=CARTESIAN_POINT('Ctrl Pts',(-0.00114303735820951,-0.0202962300920528,
-0.0153554891266914));
#39788=CARTESIAN_POINT('Ctrl Pts',(-0.00328578846826729,-0.0201385945430748,
-0.0129633887158252));
#39789=CARTESIAN_POINT('Ctrl Pts',(-0.00246022931200976,-0.0199809589940967,
-0.00985984586933738));
#39790=CARTESIAN_POINT('Ctrl Pts',(0.000587848351891767,-0.0198233234451187,
-0.00884853401505157));
#39791=CARTESIAN_POINT('Ctrl Pts',(0.0031048757463811,-0.0196656878961406,
-0.0108430510051495));
#39792=CARTESIAN_POINT('Ctrl Pts',(0.00281702675327508,-0.0195080523471626,
-0.014041592178726));
#39793=CARTESIAN_POINT('Ctrl Pts',(-1.56662226436196E-5,-0.0193504167981845,
-0.0155546663380134));
#39794=CARTESIAN_POINT('Ctrl Pts',(-0.00283420139153906,-0.0191927812492065,
-0.0140153911670897));
#39795=CARTESIAN_POINT('Ctrl Pts',(-0.0030923902806734,-0.0190351457002284,
-0.0108143218662095));
#39796=CARTESIAN_POINT('Ctrl Pts',(-0.000556960914614001,-0.0188775101512504,
-0.00884322158983128));
#39797=CARTESIAN_POINT('Ctrl Pts',(0.00248157733634815,-0.0187198746022724,
-0.0098827664672451));
#39798=CARTESIAN_POINT('Ctrl Pts',(0.00327838445817626,-0.0185622390532943,
-0.0129938028257018));
#39799=CARTESIAN_POINT('Ctrl Pts',(0.00111343055927733,-0.0184046035043163,
-0.0153659860744406));
#39800=CARTESIAN_POINT('Ctrl Pts',(-0.00205710472600525,-0.0182469679553382,
-0.0148561473239737));
#39801=CARTESIAN_POINT('Ctrl Pts',(-0.00336981118152323,-0.0180893324063602,
-0.0119252288865435));
#39802=CARTESIAN_POINT('Ctrl Pts',(-0.00163731123713958,-0.0179316968573822,
-0.00922025679049115));
#39803=CARTESIAN_POINT('Ctrl Pts',(0.0015723894163691,-0.0177740613084041,
-0.00918619889369064));
#39804=CARTESIAN_POINT('Ctrl Pts',(0.00336533302955961,-0.017616425759426,
-0.0118511905484224));
#39805=CARTESIAN_POINT('Ctrl Pts',(0.00211062072604963,-0.0174587794110365,
-0.0148132449064481));
#39806=CARTESIAN_POINT('Ctrl Pts',(1.38263585844006E-5,-0.0173536782456397,
-0.01519359063723));
#39807=CARTESIAN_POINT('Ctrl Pts',(-0.000886061088714966,-0.0173011222632356,
-0.0149009812299417));
#39808=CARTESIAN_POINT('Ctrl Pts',(0.000645619832263892,-0.0272833727275095,
-0.0147780764481064));
#39809=CARTESIAN_POINT('Ctrl Pts',(-0.0002136711385791,-0.0272308174867479,
-0.0149912826829002));
#39810=CARTESIAN_POINT('Ctrl Pts',(-0.002145217801101,-0.0271257170629937,
-0.014496832995866));
#39811=CARTESIAN_POINT('Ctrl Pts',(-0.0031191592478046,-0.026968071456247,
-0.0116489938271691));
#39812=CARTESIAN_POINT('Ctrl Pts',(-0.00126858778724075,-0.0268104359072689,
-0.00928111059245599));
#39813=CARTESIAN_POINT('Ctrl Pts',(0.00172465588943622,-0.0266528003582908,
-0.00952640532544256));
#39814=CARTESIAN_POINT('Ctrl Pts',(0.00316160671884255,-0.0264951648093128,
-0.0121661138605784));
#39815=CARTESIAN_POINT('Ctrl Pts',(0.00174153549991065,-0.0263375292603347,
-0.0148141233345868));
#39816=CARTESIAN_POINT('Ctrl Pts',(-0.00125133647152775,-0.0261798937113568,
-0.0150790349342222));
#39817=CARTESIAN_POINT('Ctrl Pts',(-0.00311401965648484,-0.0260222581623787,
-0.0127211405250328));
#39818=CARTESIAN_POINT('Ctrl Pts',(-0.00216343904199254,-0.0258646226134007,
-0.00987071517956028));
#39819=CARTESIAN_POINT('Ctrl Pts',(0.00074148049515003,-0.0257069870644226,
-0.0091026656266786));
#39820=CARTESIAN_POINT('Ctrl Pts',(0.00297659646148286,-0.0255493515154446,
-0.0111108864094343));
#39821=CARTESIAN_POINT('Ctrl Pts',(0.00252270172255615,-0.0253917159664665,
-0.0140811655096361));
#39822=CARTESIAN_POINT('Ctrl Pts',(-0.000210138203270753,-0.0252340804174884,
-0.0153302317165266));
#39823=CARTESIAN_POINT('Ctrl Pts',(-0.00275314856970804,-0.0250764448685105,
-0.0137296978048819));
#39824=CARTESIAN_POINT('Ctrl Pts',(-0.00280902139545195,-0.0249188093195324,
-0.0107254556295784));
#39825=CARTESIAN_POINT('Ctrl Pts',(-0.000327286136754079,-0.0247611737705544,
-0.00903147071439088));
#39826=CARTESIAN_POINT('Ctrl Pts',(0.0024501130310025,-0.0246035382215763,
-0.0101780535994417));
#39827=CARTESIAN_POINT('Ctrl Pts',(0.00301413255894418,-0.0244459026725983,
-0.0131294054596574));
#39828=CARTESIAN_POINT('Ctrl Pts',(0.000855249893070201,-0.0242882671236202,
-0.0152193389439868));
#39829=CARTESIAN_POINT('Ctrl Pts',(-0.00207624718246873,-0.0241306315746422,
-0.0145598530452527));
#39830=CARTESIAN_POINT('Ctrl Pts',(-0.00313210726469626,-0.0239729960256641,
-0.011746713186375));
#39831=CARTESIAN_POINT('Ctrl Pts',(-0.00135848919194423,-0.0238153604766861,
-0.00932124922841558));
#39832=CARTESIAN_POINT('Ctrl Pts',(0.00164235874342176,-0.0236577249277079,
-0.00947457304380171));
#39833=CARTESIAN_POINT('Ctrl Pts',(0.00315953518941646,-0.02350008937873,
-0.0120681751919595));
#39834=CARTESIAN_POINT('Ctrl Pts',(0.00182245566272866,-0.0233424538297518,
-0.0147590514114124));
#39835=CARTESIAN_POINT('Ctrl Pts',(-0.00116099102266572,-0.0231848182807739,
-0.0151163221329304));
#39836=CARTESIAN_POINT('Ctrl Pts',(-0.0030956234460923,-0.0230271827317957,
-0.0128172366903702));
#39837=CARTESIAN_POINT('Ctrl Pts',(-0.00223373638487103,-0.0228695471828178,
-0.00993873930759601));
#39838=CARTESIAN_POINT('Ctrl Pts',(0.000646059971377684,-0.0227119116338398,
-0.00908120246542289));
#39839=CARTESIAN_POINT('Ctrl Pts',(0.00294221967723799,-0.0225542760848617,
-0.0110193064599024));
#39840=CARTESIAN_POINT('Ctrl Pts',(0.00258044155569065,-0.0223966405358837,
-0.0140022099245627));
#39841=CARTESIAN_POINT('Ctrl Pts',(-0.000112451837632818,-0.0222390049869056,
-0.0153352221753762));
#39842=CARTESIAN_POINT('Ctrl Pts',(-0.0027037586650981,-0.0220813694379276,
-0.0138141286823404));
#39843=CARTESIAN_POINT('Ctrl Pts',(-0.00285254820264108,-0.0219237338889494,
-0.0108130525149913));
#39844=CARTESIAN_POINT('Ctrl Pts',(-0.000424407189774945,-0.0217660983399715,
-0.00904310118518834));
#39845=CARTESIAN_POINT('Ctrl Pts',(0.00238713412901858,-0.0216084627909933,
-0.0101032105672167));
#39846=CARTESIAN_POINT('Ctrl Pts',(0.00304218993769049,-0.0214508272420154,
-0.0130357006995895));
#39847=CARTESIAN_POINT('Ctrl Pts',(0.000948996941293319,-0.0212931916930374,
-0.0151914232155454));
#39848=CARTESIAN_POINT('Ctrl Pts',(-0.00200149943420506,-0.0211355561440593,
-0.0146229448683627));
#39849=CARTESIAN_POINT('Ctrl Pts',(-0.00314388436763707,-0.0209779205950813,
-0.0118438167401592));
#39850=CARTESIAN_POINT('Ctrl Pts',(-0.00144615194351038,-0.0208202850461031,
-0.00936464327158571));
#39851=CARTESIAN_POINT('Ctrl Pts',(0.00155800297706554,-0.0206626494971252,
-0.0094250563226133));
#39852=CARTESIAN_POINT('Ctrl Pts',(0.00315469158221817,-0.020505013948147,
-0.0119704800550257));
#39853=CARTESIAN_POINT('Ctrl Pts',(0.00190149984775741,-0.0203473783991691,
-0.0147014335250665));
#39854=CARTESIAN_POINT('Ctrl Pts',(-0.00106946590687894,-0.020189742850191,
-0.0151508322781805));
#39855=CARTESIAN_POINT('Ctrl Pts',(-0.00307429911961257,-0.020032107301213,
-0.0129126991000491));
#39856=CARTESIAN_POINT('Ctrl Pts',(-0.00230187697138798,-0.019874471752235,
-0.0100089153864039));
#39857=CARTESIAN_POINT('Ctrl Pts',(0.000550011568955204,-0.0197168362032569,
-0.00906269648847102));
#39858=CARTESIAN_POINT('Ctrl Pts',(0.00290503082160958,-0.0195592006542789,
-0.0109288366511528));
#39859=CARTESIAN_POINT('Ctrl Pts',(0.0026357091916162,-0.0194015651053008,
-0.0139215041368831));
#39860=CARTESIAN_POINT('Ctrl Pts',(-1.46578682547907E-5,-0.0192439295563228,
-0.0153371894741254));
#39861=CARTESIAN_POINT('Ctrl Pts',(-0.00265177838651556,-0.0190862940073448,
-0.0138969895499631));
#39862=CARTESIAN_POINT('Ctrl Pts',(-0.00289334898128302,-0.0189286584583667,
-0.0109019566595151));
#39863=CARTESIAN_POINT('Ctrl Pts',(-0.000521112197572276,-0.0187710229093887,
-0.00905772599681111));
#39864=CARTESIAN_POINT('Ctrl Pts',(0.00232185093290827,-0.0186133873604106,
-0.0100303607029996));
#39865=CARTESIAN_POINT('Ctrl Pts',(0.00306737166767089,-0.0184557518114326,
-0.0129411556096876));
#39866=CARTESIAN_POINT('Ctrl Pts',(0.00104176474572055,-0.0182981162624545,
-0.0151606535912491));
#39867=CARTESIAN_POINT('Ctrl Pts',(-0.00192469944708394,-0.0181404807134765,
-0.0146836305458396));
#39868=CARTESIAN_POINT('Ctrl Pts',(-0.00315291372182597,-0.0179828451644985,
-0.0119413602935491));
#39869=CARTESIAN_POINT('Ctrl Pts',(-0.00153192591168972,-0.0178252096155204,
-0.0094104933756749));
#39870=CARTESIAN_POINT('Ctrl Pts',(0.001471182775494,-0.0176675740665424,
-0.00937862761098531));
#39871=CARTESIAN_POINT('Ctrl Pts',(0.00314872380553277,-0.0175099385175643,
-0.0118720874234598));
#39872=CARTESIAN_POINT('Ctrl Pts',(0.00197477089672548,-0.0173522921691749,
-0.0146434895368542));
#39873=CARTESIAN_POINT('Ctrl Pts',(1.29364268071242E-5,-0.017247191003778,
-0.014999354363998));
#39874=CARTESIAN_POINT('Ctrl Pts',(-0.000829029881645386,-0.0171946350213738,
-0.0147255787232639));
#39875=CARTESIAN_POINT('Ctrl Pts',(0.000601205898390958,-0.0271768854856476,
-0.0145990624809945));
#39876=CARTESIAN_POINT('Ctrl Pts',(-0.000198972123237332,-0.0271243302448861,
-0.0147976016824351));
#39877=CARTESIAN_POINT('Ctrl Pts',(-0.00199764246837458,-0.027019229821132,
-0.0143371665262532));
#39878=CARTESIAN_POINT('Ctrl Pts',(-0.00290458384963981,-0.0268615842143851,
-0.0116852379138905));
#39879=CARTESIAN_POINT('Ctrl Pts',(-0.00118131820337908,-0.026703948665407,
-0.00948024776911945));
#39880=CARTESIAN_POINT('Ctrl Pts',(0.00160601214771848,-0.026546313116429,
-0.00970866801420186));
#39881=CARTESIAN_POINT('Ctrl Pts',(0.0029441112443766,-0.026388677567451,
-0.0121667838620248));
#39882=CARTESIAN_POINT('Ctrl Pts',(0.00162173056414967,-0.0262310420184729,
-0.0146326296046914));
#39883=CARTESIAN_POINT('Ctrl Pts',(-0.00116525365231769,-0.0260734064694949,
-0.0148793172191262));
#39884=CARTESIAN_POINT('Ctrl Pts',(-0.00289979782470325,-0.0259157709205169,
-0.0126836287415636));
#39885=CARTESIAN_POINT('Ctrl Pts',(-0.00201461022083903,-0.0257581353715388,
-0.010029291862518));
#39886=CARTESIAN_POINT('Ctrl Pts',(0.000690472047091409,-0.0256004998225608,
-0.00931407851501315));
#39887=CARTESIAN_POINT('Ctrl Pts',(0.00277182834284702,-0.0254428642735827,
-0.0111841483603438));
#39888=CARTESIAN_POINT('Ctrl Pts',(0.00234915825024082,-0.0252852287246047,
-0.013950093930273));
#39889=CARTESIAN_POINT('Ctrl Pts',(-0.000195682228101112,-0.0251275931756266,
-0.015113233495596));
#39890=CARTESIAN_POINT('Ctrl Pts',(-0.00256375203570046,-0.0249699576266486,
-0.0136228046392186));
#39891=CARTESIAN_POINT('Ctrl Pts',(-0.00261578121869382,-0.0248123220776705,
-0.0108252324059526));
#39892=CARTESIAN_POINT('Ctrl Pts',(-0.000304771238498309,-0.0246546865286925,
-0.00924778129323679));
#39893=CARTESIAN_POINT('Ctrl Pts',(0.00228156313104271,-0.0244970509797144,
-0.0103154876415214));
#39894=CARTESIAN_POINT('Ctrl Pts',(0.00280678223067475,-0.0243394154307364,
-0.0130638080274784));
#39895=CARTESIAN_POINT('Ctrl Pts',(0.000796414940521645,-0.0241817798817584,
-0.0150099693367085));
#39896=CARTESIAN_POINT('Ctrl Pts',(-0.00193341652507914,-0.0240241443327803,
-0.0143958512560506));
#39897=CARTESIAN_POINT('Ctrl Pts',(-0.00291664113744096,-0.0238665087838023,
-0.0117762348941654));
#39898=CARTESIAN_POINT('Ctrl Pts',(-0.00126503504737973,-0.0237088732348243,
-0.0095176251597855));
#39899=CARTESIAN_POINT('Ctrl Pts',(0.00152937644489143,-0.0235512376858462,
-0.00966040141535797));
#39900=CARTESIAN_POINT('Ctrl Pts',(0.00294218222106068,-0.0233936021368682,
-0.0120755826592244));
#39901=CARTESIAN_POINT('Ctrl Pts',(0.00169708401017743,-0.0232359665878901,
-0.0145813462280142));
#39902=CARTESIAN_POINT('Ctrl Pts',(-0.00108112331115675,-0.0230783310389121,
-0.0149140393306191));
#39903=CARTESIAN_POINT('Ctrl Pts',(-0.00288266713936284,-0.022920695489934,
-0.0127731141918649));
#39904=CARTESIAN_POINT('Ctrl Pts',(-0.00208007161943263,-0.022763059940956,
-0.0100926364268643));
#39905=CARTESIAN_POINT('Ctrl Pts',(0.000601615759145098,-0.0226054243919779,
-0.00929409186265181));
#39906=CARTESIAN_POINT('Ctrl Pts',(0.00273981643053748,-0.0224477888429999,
-0.0110988684431518));
#39907=CARTESIAN_POINT('Ctrl Pts',(0.00240292600413841,-0.0222901532940218,
-0.0138765699133749));
#39908=CARTESIAN_POINT('Ctrl Pts',(-0.000104715971677476,-0.0221325177450438,
-0.0151178806472884));
#39909=CARTESIAN_POINT('Ctrl Pts',(-0.00251775979616787,-0.0219748821960658,
-0.0137014272883347));
#39910=CARTESIAN_POINT('Ctrl Pts',(-0.00265631369912967,-0.0218172466470877,
-0.0109068032647757));
#39911=CARTESIAN_POINT('Ctrl Pts',(-0.000395211071688283,-0.0216596110981097,
-0.0092586116725019));
#39912=CARTESIAN_POINT('Ctrl Pts',(0.00222291671800713,-0.0215019755491316,
-0.0102457932638421));
#39913=CARTESIAN_POINT('Ctrl Pts',(0.00283290946647623,-0.0213443400001536,
-0.0129765494712121));
#39914=CARTESIAN_POINT('Ctrl Pts',(0.000883712875826465,-0.0211867044511755,
-0.0149839740067044));
#39915=CARTESIAN_POINT('Ctrl Pts',(-0.00186381087651972,-0.0210290689021975,
-0.0144546028220626));
#39916=CARTESIAN_POINT('Ctrl Pts',(-0.00292760806162782,-0.0208714333532195,
-0.0118666584319385));
#39917=CARTESIAN_POINT('Ctrl Pts',(-0.00134666724124519,-0.0207137978042414,
-0.00955803400939818));
#39918=CARTESIAN_POINT('Ctrl Pts',(0.00145082373978195,-0.0205561622552634,
-0.00961429108330222));
#39919=CARTESIAN_POINT('Ctrl Pts',(0.00293767181869759,-0.0203985267062853,
-0.0119846082349061));
#39920=CARTESIAN_POINT('Ctrl Pts',(0.00177069053200028,-0.0202408911573073,
-0.0145276920318559));
#39921=CARTESIAN_POINT('Ctrl Pts',(-0.000995894455548362,-0.0200832556083292,
-0.0149461754296697));
#39922=CARTESIAN_POINT('Ctrl Pts',(-0.00286280977095785,-0.0199256200593512,
-0.0128620094842728));
#39923=CARTESIAN_POINT('Ctrl Pts',(-0.00214352463076619,-0.0197679845103731,
-0.0101579849034705));
#39924=CARTESIAN_POINT('Ctrl Pts',(0.000512174786018637,-0.0196103489613951,
-0.00927685896189047));
#39925=CARTESIAN_POINT('Ctrl Pts',(0.00270518589683808,-0.019452713412417,
-0.0110146222971561));
#39926=CARTESIAN_POINT('Ctrl Pts',(0.00245439162995732,-0.019295077863439,
-0.0138014160950401));
#39927=CARTESIAN_POINT('Ctrl Pts',(-1.3649513865962E-5,-0.019137442314461,
-0.0151197126102372));
#39928=CARTESIAN_POINT('Ctrl Pts',(-0.00246935538149206,-0.0189798067654829,
-0.0137785879328362));
#39929=CARTESIAN_POINT('Ctrl Pts',(-0.00269430768189265,-0.0188221712165049,
-0.0109895914528207));
#39930=CARTESIAN_POINT('Ctrl Pts',(-0.000485263480530543,-0.0186645356675268,
-0.00927223040379092));
#39931=CARTESIAN_POINT('Ctrl Pts',(0.0021621245294684,-0.0185069001185488,
-0.0101779549387543));
#39932=CARTESIAN_POINT('Ctrl Pts',(0.00285635887716552,-0.0183492645695708,
-0.0128885083936734));
#39933=CARTESIAN_POINT('Ctrl Pts',(0.000970098932163777,-0.0181916290205927,
-0.0149553211080576));
#39934=CARTESIAN_POINT('Ctrl Pts',(-0.00179229416816263,-0.0180339934716147,
-0.0145111137677053));
#39935=CARTESIAN_POINT('Ctrl Pts',(-0.0029360162621287,-0.0178763579226366,
-0.0119574917005547));
#39936=CARTESIAN_POINT('Ctrl Pts',(-0.00142654058623987,-0.0177187223736586,
-0.00960072996085867));
#39937=CARTESIAN_POINT('Ctrl Pts',(0.00136997613461892,-0.0175610868246805,
-0.00957105632827997));
#39938=CARTESIAN_POINT('Ctrl Pts',(0.00293211458150592,-0.0174034512757025,
-0.0118929842984973));
#39939=CARTESIAN_POINT('Ctrl Pts',(0.0018389210674013,-0.017245804927313,
-0.0144737341672604));
#39940=CARTESIAN_POINT('Ctrl Pts',(1.20464950298498E-5,-0.0171407037619162,
-0.0148051180907662));
#39941=CARTESIAN_POINT('Ctrl Pts',(-0.000771998674575806,-0.017088147779512,
-0.0145501762165862));
#39942=CARTESIAN_POINT('Ctrl Pts',(-0.00300179803210124,-0.0271787743899901,
-0.0121753188445143));
#39943=CARTESIAN_POINT('Ctrl Pts',(-0.00299170500774972,-0.0271787744029572,
-0.012274001554098));
#39944=CARTESIAN_POINT('Ctrl Pts',(-0.00297664702496829,-0.0271787743898748,
-0.0123720503346277));
#39945=CARTESIAN_POINT('Ctrl Pts',(-0.00295682936558202,-0.0271787743898749,
-0.0124691137840994));
#39946=CARTESIAN_POINT('Ctrl Pts',(-0.00290457240419616,-0.0271787743898752,
-0.0127250592937154));
#39947=CARTESIAN_POINT('Ctrl Pts',(-0.00281935579375609,-0.0271787743898754,
-0.012974265349726));
#39948=CARTESIAN_POINT('Ctrl Pts',(-0.00270343235514401,-0.0271787743898756,
-0.0132095505979502));
#39949=CARTESIAN_POINT('Ctrl Pts',(-0.00269512702070926,-0.0271787743898756,
-0.0132264076089004));
#39950=CARTESIAN_POINT('Ctrl Pts',(-0.00268666329850635,-0.0271787743898756,
-0.0132431924273196));
#39951=CARTESIAN_POINT('Ctrl Pts',(-0.00267804168256273,-0.0271787743898756,
-0.0132599020323125));
#39952=CARTESIAN_POINT('Ctrl Pts',(-0.00267151568645102,-0.0271787743898757,
-0.0132725501040805));
#39953=CARTESIAN_POINT('Ctrl Pts',(-0.00266490146409413,-0.0271787743898756,
-0.0132851506618195));
#39954=CARTESIAN_POINT('Ctrl Pts',(-0.00265820309333032,-0.0271787743898756,
-0.0132976957827427));
#39955=CARTESIAN_POINT('Ctrl Pts',(-0.00249348720410649,-0.0271787743898759,
-0.0136061858351965));
#39956=CARTESIAN_POINT('Ctrl Pts',(-0.00227771368615723,-0.0271787743898759,
-0.0138830139207218));
#39957=CARTESIAN_POINT('Ctrl Pts',(-0.00201563806114113,-0.0271787743898759,
-0.0141093884962233));
#39958=CARTESIAN_POINT('Ctrl Pts',(-0.00200231890338116,-0.0271787743898759,
-0.014120893262009));
#39959=CARTESIAN_POINT('Ctrl Pts',(-0.00198887690751847,-0.0271787743898759,
-0.0141322675641596));
#39960=CARTESIAN_POINT('Ctrl Pts',(-0.00197533127033276,-0.0271787743898759,
-0.0141434930754665));
#39961=CARTESIAN_POINT('Ctrl Pts',(-0.00194648600772747,-0.0271787743898759,
-0.0141673976594359));
#39962=CARTESIAN_POINT('Ctrl Pts',(-0.0019171536737065,-0.0271787743898759,
-0.014190642780961));
#39963=CARTESIAN_POINT('Ctrl Pts',(-0.00188734151124788,-0.0271787743898759,
-0.0142132063515489));
#39964=CARTESIAN_POINT('Ctrl Pts',(-0.00166838124506507,-0.0271787743898758,
-0.0143789281581709));
#39965=CARTESIAN_POINT('Ctrl Pts',(-0.00142362040013632,-0.0271787743898756,
-0.014508195233492));
#39966=CARTESIAN_POINT('Ctrl Pts',(-0.00116282079016005,-0.0271787743898753,
-0.0145991360864556));
#39967=CARTESIAN_POINT('Ctrl Pts',(-0.00114190913175246,-0.0271787743898753,
-0.0146064279840648));
#39968=CARTESIAN_POINT('Ctrl Pts',(-0.00112089415409831,-0.0271787743898753,
-0.0146134714313065));
#39969=CARTESIAN_POINT('Ctrl Pts',(-0.00109978090207821,-0.0271787743898752,
-0.0146202643895321));
#39970=CARTESIAN_POINT('Ctrl Pts',(-0.00108278352153522,-0.0271787743898752,
-0.014625733111066));
#39971=CARTESIAN_POINT('Ctrl Pts',(-0.00106571994357321,-0.0271787743898752,
-0.0146310401292033));
#39972=CARTESIAN_POINT('Ctrl Pts',(-0.00104861536807709,-0.0271787743898752,
-0.0146361778513352));
#39973=CARTESIAN_POINT('Ctrl Pts',(-0.000873308221192212,-0.0271787743898749,
-0.0146888350721259));
#39974=CARTESIAN_POINT('Ctrl Pts',(-0.000693203211584065,-0.0271787743898748,
-0.0147239408709482));
#39975=CARTESIAN_POINT('Ctrl Pts',(-0.000511222013638069,-0.0271787743898745,
-0.0147408433458497));
#39976=CARTESIAN_POINT('Ctrl Pts',(-0.000462148710303348,-0.0271787743898744,
-0.0147454012907765));
#39977=CARTESIAN_POINT('Ctrl Pts',(-0.000412939374657768,-0.0271787743898743,
-0.0147486309176275));
#39978=CARTESIAN_POINT('Ctrl Pts',(-0.000363653449390059,-0.0271787743898743,
-0.0147505091750227));
#39979=CARTESIAN_POINT('Ctrl Pts',(-0.000335973747865316,-0.0271787743898743,
-0.0147515640320393));
#39980=CARTESIAN_POINT('Ctrl Pts',(-0.000308269918835363,-0.0271787743898742,
-0.0147521925733346));
#39981=CARTESIAN_POINT('Ctrl Pts',(-0.000280552769976453,-0.0271787743898741,
-0.0147523901087495));
#39982=CARTESIAN_POINT('Ctrl Pts',(-0.000263915086500017,-0.0271787743898741,
-0.0147525086826953));
#39983=CARTESIAN_POINT('Ctrl Pts',(-0.000247272607789491,-0.0271787743898741,
-0.0147524719481251));
#39984=CARTESIAN_POINT('Ctrl Pts',(-0.000230627712965026,-0.027178774389874,
-0.0147522788149046));
#39985=CARTESIAN_POINT('Ctrl Pts',(-0.000216079303444679,-0.027178774389874,
-0.0147521100075187));
#39986=CARTESIAN_POINT('Ctrl Pts',(-0.000201531292573118,-0.027178774389874,
-0.0147518216826401));
#39987=CARTESIAN_POINT('Ctrl Pts',(-0.000186996318757126,-0.027178774389874,
-0.0147514136797492));
#39988=CARTESIAN_POINT('Ctrl Pts',(-9.88498753030835E-5,-0.0271787743898738,
-0.0147489393716279));
#39989=CARTESIAN_POINT('Ctrl Pts',(-1.10664436843476E-5,-0.0271787743898736,
-0.0147420666416071));
#39990=CARTESIAN_POINT('Ctrl Pts',(7.60196322764222E-5,-0.0271787743898741,
-0.014730708327085));
#39991=CARTESIAN_POINT('Ctrl Pts',(0.000165600962475197,-0.0271787743898746,
-0.0147190245657892));
#39992=CARTESIAN_POINT('Ctrl Pts',(0.00025444545205105,-0.0271787743898749,
-0.0147025947256612));
#39993=CARTESIAN_POINT('Ctrl Pts',(0.000342167409581488,-0.027178774389875,
-0.0146812694278629));
#39994=CARTESIAN_POINT('Ctrl Pts',(0.000423588645699061,-0.0271787743898751,
-0.0146614758418989));
#39995=CARTESIAN_POINT('Ctrl Pts',(0.000504043196429721,-0.0271787743898753,
-0.0146374642252552));
#39996=CARTESIAN_POINT('Ctrl Pts',(0.000583194675706476,-0.0271787743898754,
-0.0146090727027793));
#39997=CARTESIAN_POINT('Ctrl Pts',(0.000589319753685136,-0.0271787743898754,
-0.0146068756460636));
#39998=CARTESIAN_POINT('Ctrl Pts',(0.000595437012035837,-0.0271787743898754,
-0.0146046523408536));
#39999=CARTESIAN_POINT('Ctrl Pts',(0.000601546286299641,-0.0271787743898749,
-0.0146024027019753));
#40000=CARTESIAN_POINT('Origin',(0.,-0.0172787743898723,-0.0121758532865581));
#40001=CARTESIAN_POINT('',(0.0028,-0.0171787743898723,-0.0121758532865581));
#40002=CARTESIAN_POINT('',(0.0029,-0.0172787743898723,-0.0121758532865581));
#40003=CARTESIAN_POINT('Origin',(0.,-0.0171787743898623,-0.0121758532865581));
#40004=CARTESIAN_POINT('Origin',(0.,-0.0171787743898723,-0.0121758532865581));
#40005=CARTESIAN_POINT('Ctrl Pts',(0.00176574804943854,-0.0343694510790993,
-0.0139408222827216));
#40006=CARTESIAN_POINT('Ctrl Pts',(0.00117779798543426,-0.0343164323406156,
-0.0145290523617757));
#40007=CARTESIAN_POINT('Ctrl Pts',(-0.000621947546423068,-0.0342104065694797,
-0.0150611744231589));
#40008=CARTESIAN_POINT('Ctrl Pts',(-0.00276742883656761,-0.034051373765692,
-0.0132101082372629));
#40009=CARTESIAN_POINT('Ctrl Pts',(-0.00236482154393933,-0.0338923526677358,
-0.0104096023683696));
#40010=CARTESIAN_POINT('Ctrl Pts',(0.000204910886527884,-0.0337333315697798,
-0.00923059166728955));
#40011=CARTESIAN_POINT('Ctrl Pts',(0.00258846653129079,-0.0335743104718236,
-0.0107552119605033));
#40012=CARTESIAN_POINT('Ctrl Pts',(0.00259485856040026,-0.0334152893738676,
-0.0135839857225452));
#40013=CARTESIAN_POINT('Ctrl Pts',(0.000219742753097404,-0.0332562682759115,
-0.0151201044584147));
#40014=CARTESIAN_POINT('Ctrl Pts',(-0.00235736426033115,-0.0330972471779554,
-0.0139534669866695));
#40015=CARTESIAN_POINT('Ctrl Pts',(-0.00277031546347644,-0.0329382260799993,
-0.0111550102704199));
#40016=CARTESIAN_POINT('Ctrl Pts',(-0.000640244886201917,-0.0327792049820433,
-0.00929366988804862));
#40017=CARTESIAN_POINT('Ctrl Pts',(0.00207759635746219,-0.0326201838840872,
-0.010078116312487));
#40018=CARTESIAN_POINT('Ctrl Pts',(0.00288822476733986,-0.0324611627861311,
-0.0127882449165322));
#40019=CARTESIAN_POINT('Ctrl Pts',(0.00104752965503765,-0.032302141688175,
-0.0149362096781171));
#40020=CARTESIAN_POINT('Ctrl Pts',(-0.00175478257452117,-0.0321431205902189,
-0.0145502212948222));
#40021=CARTESIAN_POINT('Ctrl Pts',(-0.00294623597977783,-0.0319840994922628,
-0.0119846095548743));
#40022=CARTESIAN_POINT('Ctrl Pts',(-0.00143310357258225,-0.0318250783943067,
-0.00959455553988092));
#40023=CARTESIAN_POINT('Ctrl Pts',(0.00139559025190196,-0.0316660572963506,
-0.00957408303108934));
#40024=CARTESIAN_POINT('Ctrl Pts',(0.00294315991374164,-0.0315070361983945,
-0.0119419835692896));
#40025=CARTESIAN_POINT('Ctrl Pts',(0.00178896491918136,-0.0313480151004384,
-0.0145245742798952));
#40026=CARTESIAN_POINT('Ctrl Pts',(-0.00100746200682521,-0.0311889940024823,
-0.0149510805060739));
#40027=CARTESIAN_POINT('Ctrl Pts',(-0.0028790642322956,-0.0310299729045262,
-0.0128299910268252));
#40028=CARTESIAN_POINT('Ctrl Pts',(-0.00210773065532187,-0.0308709518065702,
-0.0101083992625063));
#40029=CARTESIAN_POINT('Ctrl Pts',(0.000598437139890697,-0.0307119307086141,
-0.00928472180902646));
#40030=CARTESIAN_POINT('Ctrl Pts',(0.002755292326791,-0.030552909610658,
-0.0111149852850437));
#40031=CARTESIAN_POINT('Ctrl Pts',(0.0023827642768738,-0.0303938885127019,
-0.0139192225077422));
#40032=CARTESIAN_POINT('Ctrl Pts',(-0.000176943674720605,-0.0302348674147459,
-0.0151228549563469));
#40033=CARTESIAN_POINT('Ctrl Pts',(-0.00257451101079573,-0.0300758463167898,
-0.0136216312142491));
#40034=CARTESIAN_POINT('Ctrl Pts',(-0.00260817017370304,-0.0299168252188337,
-0.0107923783780903));
#40035=CARTESIAN_POINT('Ctrl Pts',(-0.000248651555250166,-0.0297578041208776,
-0.00923473179216972));
#40036=CARTESIAN_POINT('Ctrl Pts',(0.00234119373410808,-0.0295987830229215,
-0.0103738661700957));
#40037=CARTESIAN_POINT('Ctrl Pts',(0.00277780667786063,-0.0294397535098039,
-0.0131736113086904));
#40038=CARTESIAN_POINT('Ctrl Pts',(0.0013745903082445,-0.0293337310293383,
-0.0144197667809647));
#40039=CARTESIAN_POINT('Ctrl Pts',(0.000564492329997462,-0.0292807155815248,
-0.0146077928730744));
#40040=CARTESIAN_POINT('Ctrl Pts',(0.00188614792707067,-0.0342711666745561,
-0.0140611690395707));
#40041=CARTESIAN_POINT('Ctrl Pts',(0.00125810770649936,-0.0342181479360723,
-0.0146895083683901));
#40042=CARTESIAN_POINT('Ctrl Pts',(-0.000664355866515366,-0.0341121221649365,
-0.01525791387978));
#40043=CARTESIAN_POINT('Ctrl Pts',(-0.00295612965001848,-0.0339530893611486,
-0.0132806302857199));
#40044=CARTESIAN_POINT('Ctrl Pts',(-0.00252607004403119,-0.0337940682631925,
-0.0102891682019633));
#40045=CARTESIAN_POINT('Ctrl Pts',(0.000218883007675803,-0.0336350471652364,
-0.00902976508919009));
#40046=CARTESIAN_POINT('Ctrl Pts',(0.00276496456209497,-0.0334760260672803,
-0.0106583436434915));
#40047=CARTESIAN_POINT('Ctrl Pts',(0.00277179244020502,-0.0333170049693242,
-0.0136800011042621));
#40048=CARTESIAN_POINT('Ctrl Pts',(0.000234726204780603,-0.0331579838713681,
-0.0153208621378145));
#40049=CARTESIAN_POINT('Ctrl Pts',(-0.00251810427562861,-0.032998962773412,
-0.0140746759394636));
#40050=CARTESIAN_POINT('Ctrl Pts',(-0.00295921310541975,-0.032839941675456,
-0.0110854027325473));
#40051=CARTESIAN_POINT('Ctrl Pts',(-0.000683900834726285,-0.0326809205774999,
-0.00909714438226979));
#40052=CARTESIAN_POINT('Ctrl Pts',(0.00221926002645898,-0.0325218994795438,
-0.00993507932877742));
#40053=CARTESIAN_POINT('Ctrl Pts',(0.00308516221188206,-0.0323628783815877,
-0.0128300016537604));
#40054=CARTESIAN_POINT('Ctrl Pts',(0.00111895685685313,-0.0322038572836316,
-0.0151244282475049));
#40055=CARTESIAN_POINT('Ctrl Pts',(-0.00187443475667168,-0.0320448361856755,
-0.0147121207332723));
#40056=CARTESIAN_POINT('Ctrl Pts',(-0.00314712899594364,-0.0318858150877194,
-0.0119715693468445));
#40057=CARTESIAN_POINT('Ctrl Pts',(-0.00153082164443737,-0.0317267939897633,
-0.00941854632218373));
#40058=CARTESIAN_POINT('Ctrl Pts',(0.001490750428127,-0.0315677728918073,
-0.0093966778681699));
#40059=CARTESIAN_POINT('Ctrl Pts',(0.00314384318425632,-0.0314087517938512,
-0.0119260368517781));
#40060=CARTESIAN_POINT('Ctrl Pts',(0.00191094786993477,-0.0312497306958951,
-0.0146847249425447));
#40061=CARTESIAN_POINT('Ctrl Pts',(-0.00107615714279284,-0.031090709597939,
-0.015140313062631));
#40062=CARTESIAN_POINT('Ctrl Pts',(-0.0030753770535804,-0.030931688499983,
-0.0128745942780693));
#40063=CARTESIAN_POINT('Ctrl Pts',(-0.00225144907147014,-0.0307726674020269,
-0.00996742716199346));
#40064=CARTESIAN_POINT('Ctrl Pts',(0.000639242371665568,-0.0306136463040708,
-0.0090875861665865));
#40065=CARTESIAN_POINT('Ctrl Pts',(0.00294316559619194,-0.0304546252061146,
-0.0110426485903456));
#40066=CARTESIAN_POINT('Ctrl Pts',(0.00254523622605875,-0.0302956041081586,
-0.0140380964552258));
#40067=CARTESIAN_POINT('Ctrl Pts',(-0.000189008814359819,-0.0301365830102025,
-0.0153238001821038));
#40068=CARTESIAN_POINT('Ctrl Pts',(-0.0027500574658865,-0.0299775619122464,
-0.013720213503853));
#40069=CARTESIAN_POINT('Ctrl Pts',(-0.00278601172355351,-0.0298185408142903,
-0.0106980443026601));
#40070=CARTESIAN_POINT('Ctrl Pts',(-0.000265606192031256,-0.0296595197163342,
-0.00903418751398792));
#40071=CARTESIAN_POINT('Ctrl Pts',(0.00250083114058254,-0.0295004986183781,
-0.0102509952835128));
#40072=CARTESIAN_POINT('Ctrl Pts',(0.00296721511821342,-0.0293414691052605,
-0.013241644765564));
#40073=CARTESIAN_POINT('Ctrl Pts',(0.00146831857539992,-0.029235446624795,
-0.0145727710049986));
#40074=CARTESIAN_POINT('Ctrl Pts',(0.00060298298979322,-0.0291824311769814,
-0.0147736179061069));
#40075=CARTESIAN_POINT('Ctrl Pts',(0.00200654780470278,-0.0341728822700128,
-0.0141815157964198));
#40076=CARTESIAN_POINT('Ctrl Pts',(0.00133841742756444,-0.034119863531529,
-0.0148499643750045));
#40077=CARTESIAN_POINT('Ctrl Pts',(-0.000706764186607663,-0.0340138377603931,
-0.0154546533364009));
#40078=CARTESIAN_POINT('Ctrl Pts',(-0.00314483046346935,-0.0338548049566054,
-0.0133511523341767));
#40079=CARTESIAN_POINT('Ctrl Pts',(-0.00268731854412305,-0.0336957838586492,
-0.0101687340355571));
#40080=CARTESIAN_POINT('Ctrl Pts',(0.000232855128823719,-0.0335367627606931,
-0.00882893851109065));
#40081=CARTESIAN_POINT('Ctrl Pts',(0.00294146259289918,-0.033377741662737,
-0.0105614753264796));
#40082=CARTESIAN_POINT('Ctrl Pts',(0.00294872632000978,-0.0332187205647809,
-0.0137760164859788));
#40083=CARTESIAN_POINT('Ctrl Pts',(0.000249709656463804,-0.0330596994668248,
-0.0155216198172141));
#40084=CARTESIAN_POINT('Ctrl Pts',(-0.00267884429092607,-0.0329006783688689,
-0.0141958848922576));
#40085=CARTESIAN_POINT('Ctrl Pts',(-0.00314811074736304,-0.0327416572709126,
-0.0110157951946748));
#40086=CARTESIAN_POINT('Ctrl Pts',(-0.000727556783250659,-0.0325826361729567,
-0.00890061887649098));
#40087=CARTESIAN_POINT('Ctrl Pts',(0.00236092369545578,-0.0324236150750004,
-0.00979204234506796));
#40088=CARTESIAN_POINT('Ctrl Pts',(0.00328209965642423,-0.0322645939770444,
-0.0128717583909887));
#40089=CARTESIAN_POINT('Ctrl Pts',(0.00119038405866861,-0.0321055728790883,
-0.0153126468168928));
#40090=CARTESIAN_POINT('Ctrl Pts',(-0.00199408693882221,-0.0319465517811322,
-0.0148740201717226));
#40091=CARTESIAN_POINT('Ctrl Pts',(-0.00334802201210944,-0.0317875306831761,
-0.011958529138815));
#40092=CARTESIAN_POINT('Ctrl Pts',(-0.00162853971629248,-0.0316285095852202,
-0.00924253710448655));
#40093=CARTESIAN_POINT('Ctrl Pts',(0.00158591060435204,-0.0314694884872639,
-0.00921927270525046));
#40094=CARTESIAN_POINT('Ctrl Pts',(0.00334452645477101,-0.031310467389308,
-0.0119100901342666));
#40095=CARTESIAN_POINT('Ctrl Pts',(0.00203293082068818,-0.0311514462913518,
-0.0148448756051943));
#40096=CARTESIAN_POINT('Ctrl Pts',(-0.00114485227876049,-0.0309924251933957,
-0.0153295456191882));
#40097=CARTESIAN_POINT('Ctrl Pts',(-0.00327168987486519,-0.0308334040954397,
-0.0129191975293132));
#40098=CARTESIAN_POINT('Ctrl Pts',(-0.00239516748761842,-0.0306743829974836,
-0.00982645506148058));
#40099=CARTESIAN_POINT('Ctrl Pts',(0.000680047603440434,-0.0305153618995274,
-0.00889045052414654));
#40100=CARTESIAN_POINT('Ctrl Pts',(0.0031310388655929,-0.0303563408015715,
-0.0109703118956475));
#40101=CARTESIAN_POINT('Ctrl Pts',(0.00270770817524368,-0.0301973197036154,
-0.0141569704027094));
#40102=CARTESIAN_POINT('Ctrl Pts',(-0.000201073953999031,-0.0300382986056592,
-0.0155247454078606));
#40103=CARTESIAN_POINT('Ctrl Pts',(-0.00292560392097725,-0.0298792775077031,
-0.0138187957934569));
#40104=CARTESIAN_POINT('Ctrl Pts',(-0.00296385327340397,-0.029720256409747,
-0.0106037102272297));
#40105=CARTESIAN_POINT('Ctrl Pts',(-0.000282560828812347,-0.0295612353117909,
-0.00883364323580613));
#40106=CARTESIAN_POINT('Ctrl Pts',(0.002660468547057,-0.0294022142138348,
-0.0101281243969297));
#40107=CARTESIAN_POINT('Ctrl Pts',(0.00315662355856618,-0.0292431847007172,
-0.0133096782224377));
#40108=CARTESIAN_POINT('Ctrl Pts',(0.00156204684255533,-0.0291371622202517,
-0.0147257752290324));
#40109=CARTESIAN_POINT('Ctrl Pts',(0.000641473649588978,-0.0290841467724382,
-0.0149394429391394));
#40110=CARTESIAN_POINT('Ctrl Pts',(0.0021269476823349,-0.0340745978654695,
-0.0143018625532689));
#40111=CARTESIAN_POINT('Ctrl Pts',(0.00141872714862954,-0.0340215791269856,
-0.0150104203816191));
#40112=CARTESIAN_POINT('Ctrl Pts',(-0.000749172506699962,-0.0339155533558498,
-0.0156513927930219));
#40113=CARTESIAN_POINT('Ctrl Pts',(-0.00333353127692023,-0.033756520552062,
-0.0134216743826337));
#40114=CARTESIAN_POINT('Ctrl Pts',(-0.00284856704421491,-0.0335974994541059,
-0.0100482998691509));
#40115=CARTESIAN_POINT('Ctrl Pts',(0.000246827249971632,-0.0334384783561498,
-0.0086281119329912));
#40116=CARTESIAN_POINT('Ctrl Pts',(0.00311796062370337,-0.0332794572581937,
-0.0104646070094678));
#40117=CARTESIAN_POINT('Ctrl Pts',(0.00312566019981454,-0.0331204361602375,
-0.0138720318676957));
#40118=CARTESIAN_POINT('Ctrl Pts',(0.000264693108147008,-0.0329614150622815,
-0.0157223774966138));
#40119=CARTESIAN_POINT('Ctrl Pts',(-0.00283958430622353,-0.0328023939643254,
-0.0143170938450517));
#40120=CARTESIAN_POINT('Ctrl Pts',(-0.00333700838930635,-0.0326433728663693,
-0.0109461876568023));
#40121=CARTESIAN_POINT('Ctrl Pts',(-0.000771212731775031,-0.0324843517684132,
-0.00870409337071217));
#40122=CARTESIAN_POINT('Ctrl Pts',(0.00250258736445257,-0.0323253306704572,
-0.00964900536135851));
#40123=CARTESIAN_POINT('Ctrl Pts',(0.00347903710096643,-0.0321663095725011,
-0.0129135151282171));
#40124=CARTESIAN_POINT('Ctrl Pts',(0.0012618112604841,-0.032007288474545,
-0.0155008653862805));
#40125=CARTESIAN_POINT('Ctrl Pts',(-0.0021137391209727,-0.0318482673765889,
-0.0150359196101727));
#40126=CARTESIAN_POINT('Ctrl Pts',(-0.00354891502827525,-0.0316892462786328,
-0.0119454889307853));
#40127=CARTESIAN_POINT('Ctrl Pts',(-0.00172625778814758,-0.0315302251806767,
-0.00906652788678938));
#40128=CARTESIAN_POINT('Ctrl Pts',(0.00168107078057706,-0.0313712040827206,
-0.00904186754233102));
#40129=CARTESIAN_POINT('Ctrl Pts',(0.0035452097252857,-0.0312121829847645,
-0.0118941434167551));
#40130=CARTESIAN_POINT('Ctrl Pts',(0.00215491377144159,-0.0310531618868085,
-0.0150050262678438));
#40131=CARTESIAN_POINT('Ctrl Pts',(-0.00121354741472812,-0.0308941407888524,
-0.0155187781757453));
#40132=CARTESIAN_POINT('Ctrl Pts',(-0.00346800269614999,-0.0307351196908962,
-0.0129638007805572));
#40133=CARTESIAN_POINT('Ctrl Pts',(-0.0025388859037667,-0.0305760985929401,
-0.00968548296096771));
#40134=CARTESIAN_POINT('Ctrl Pts',(0.000720852835215301,-0.030417077494984,
-0.00869331488170658));
#40135=CARTESIAN_POINT('Ctrl Pts',(0.00331891213499383,-0.030258056397028,
-0.0108979752009492));
#40136=CARTESIAN_POINT('Ctrl Pts',(0.00287018012442863,-0.0300990352990719,
-0.014275844350193));
#40137=CARTESIAN_POINT('Ctrl Pts',(-0.000213139093638245,-0.0299400142011158,
-0.0157256906336175));
#40138=CARTESIAN_POINT('Ctrl Pts',(-0.00310115037606801,-0.0297809931031597,
-0.0139173780830608));
#40139=CARTESIAN_POINT('Ctrl Pts',(-0.00314169482325445,-0.0296219720052037,
-0.0105093761517993));
#40140=CARTESIAN_POINT('Ctrl Pts',(-0.000299515465593438,-0.0294629509072476,
-0.00863309895762433));
#40141=CARTESIAN_POINT('Ctrl Pts',(0.00282010595353146,-0.0293039298092915,
-0.0100052535103467));
#40142=CARTESIAN_POINT('Ctrl Pts',(0.00334603199891895,-0.0291449002961739,
-0.0133777116793113));
#40143=CARTESIAN_POINT('Ctrl Pts',(0.00165577510971075,-0.0290388778157083,
-0.0148787794530662));
#40144=CARTESIAN_POINT('Ctrl Pts',(0.000679964309384735,-0.0289858623678948,
-0.015105267972172));
#40145=CARTESIAN_POINT('Ctrl Pts',(0.00267357255235765,-0.0292787743898725,
-0.0108117659595362));
#40146=CARTESIAN_POINT('Ctrl Pts',(0.00270942158183447,-0.0292787743769101,
-0.0109044263882472));
#40147=CARTESIAN_POINT('Ctrl Pts',(0.00274057340703459,-0.0292787743898644,
-0.0109987720071259));
#40148=CARTESIAN_POINT('Ctrl Pts',(0.00276704473487997,-0.0292787743898645,
-0.0110943957950434));
#40149=CARTESIAN_POINT('Ctrl Pts',(0.00284508802080715,-0.0292787743898647,
-0.0113763157147949));
#40150=CARTESIAN_POINT('Ctrl Pts',(0.0028827204075281,-0.0292787743898651,
-0.0116697038393258));
#40151=CARTESIAN_POINT('Ctrl Pts',(0.00287783547757714,-0.0292787743898655,
-0.011963215493794));
#40152=CARTESIAN_POINT('Ctrl Pts',(0.00287617507520755,-0.0292787743898657,
-0.0120629809871526));
#40153=CARTESIAN_POINT('Ctrl Pts',(0.00286958813063577,-0.029278774389866,
-0.0121623132322861));
#40154=CARTESIAN_POINT('Ctrl Pts',(0.00285803849087999,-0.0292787743898655,
-0.0122608040104835));
#40155=CARTESIAN_POINT('Ctrl Pts',(0.00282980275969606,-0.0292787743898642,
-0.0125015872033864));
#40156=CARTESIAN_POINT('Ctrl Pts',(0.00277204190124365,-0.0292787743898644,
-0.0127374351857662));
#40157=CARTESIAN_POINT('Ctrl Pts',(0.00268282981823786,-0.0292787743898641,
-0.0129617552268038));
#40158=CARTESIAN_POINT('Ctrl Pts',(0.00267753866184219,-0.0292787743898641,
-0.0129750596176421));
#40159=CARTESIAN_POINT('Ctrl Pts',(0.00267213630271764,-0.0292787743898641,
-0.012988323028573));
#40160=CARTESIAN_POINT('Ctrl Pts',(0.00266662212529158,-0.0292787743898641,
-0.013001543904261));
#40161=CARTESIAN_POINT('Ctrl Pts',(0.00266099360072982,-0.0292787743898641,
-0.0130150389403812));
#40162=CARTESIAN_POINT('Ctrl Pts',(0.00265525166642689,-0.0292787743898641,
-0.0130284821681761));
#40163=CARTESIAN_POINT('Ctrl Pts',(0.0026493980102342,-0.0292787743898641,
-0.0130418677383362));
#40164=CARTESIAN_POINT('Ctrl Pts',(0.00263902493206007,-0.0292787743898641,
-0.0130655878819704));
#40165=CARTESIAN_POINT('Ctrl Pts',(0.0026282991561088,-0.029278774389864,
-0.013089131499636));
#40166=CARTESIAN_POINT('Ctrl Pts',(0.00261721939710271,-0.029278774389864,
-0.0131124910242309));
#40167=CARTESIAN_POINT('Ctrl Pts',(0.00248779252520929,-0.0292787743898638,
-0.0133853625005478));
#40168=CARTESIAN_POINT('Ctrl Pts',(0.00231037877727216,-0.0292787743898636,
-0.0136334676728105));
#40169=CARTESIAN_POINT('Ctrl Pts',(0.00209532275943825,-0.0292787743898636,
-0.0138485399734916));
#40170=CARTESIAN_POINT('Ctrl Pts',(0.00208085851571133,-0.0292787743898636,
-0.0138630053123707));
#40171=CARTESIAN_POINT('Ctrl Pts',(0.00206621895014382,-0.0292787743898636,
-0.0138773230384675));
#40172=CARTESIAN_POINT('Ctrl Pts',(0.0020514297876405,-0.0292787743898636,
-0.0138914683166346));
#40173=CARTESIAN_POINT('Ctrl Pts',(0.00188347219527991,-0.0292787743898637,
-0.0140521134419883));
#40174=CARTESIAN_POINT('Ctrl Pts',(0.00169583105268622,-0.0292787743898637,
-0.0141911607834212));
#40175=CARTESIAN_POINT('Ctrl Pts',(0.00149313379990858,-0.0292787743898639,
-0.0143044621723636));
#40176=CARTESIAN_POINT('Ctrl Pts',(0.00146908053839098,-0.0292787743898639,
-0.0143179071890138));
#40177=CARTESIAN_POINT('Ctrl Pts',(0.00144481456590165,-0.0292787743898639,
-0.0143309872340784));
#40178=CARTESIAN_POINT('Ctrl Pts',(0.00142034322819153,-0.029278774389864,
-0.0143436933191354));
#40179=CARTESIAN_POINT('Ctrl Pts',(0.00140470331950154,-0.029278774389864,
-0.0143518139217952));
#40180=CARTESIAN_POINT('Ctrl Pts',(0.00138897952649762,-0.029278774389864,
-0.0143597817659317));
#40181=CARTESIAN_POINT('Ctrl Pts',(0.00137317376994739,-0.029278774389864,
-0.0143675944004388));
#40182=CARTESIAN_POINT('Ctrl Pts',(0.00136117393413807,-0.029278774389864,
-0.0143735258046728));
#40183=CARTESIAN_POINT('Ctrl Pts',(0.0013491292146614,-0.029278774389864,
-0.0143793665313414));
#40184=CARTESIAN_POINT('Ctrl Pts',(0.00133704814932165,-0.029278774389864,
-0.0143851120911698));
#40185=CARTESIAN_POINT('Ctrl Pts',(0.00109928812760478,-0.0292787743898642,
-0.0144981869228298));
#40186=CARTESIAN_POINT('Ctrl Pts',(0.000846613469422695,-0.0292787743898645,
-0.0145751840384429));
#40187=CARTESIAN_POINT('Ctrl Pts',(0.000585792948533347,-0.029278774389865,
-0.0146085347508578));
#40188=CARTESIAN_POINT('Ctrl Pts',(0.000579083537205416,-0.029278774389865,
-0.0146093926727993));
#40189=CARTESIAN_POINT('Ctrl Pts',(0.000572368752880877,-0.029278774389865,
-0.0146102214611691));
#40190=CARTESIAN_POINT('Ctrl Pts',(0.000565648716062883,-0.029278774389865,
-0.0146110209461011));
#40191=CARTESIAN_POINT('Ctrl Pts',(-0.00214342189834001,-0.034078774389864,
-0.0134651256783301));
#40192=CARTESIAN_POINT('Ctrl Pts',(-0.00203881996138949,-0.0340787743898638,
-0.0136859499145821));
#40193=CARTESIAN_POINT('Ctrl Pts',(-0.00190154780260284,-0.0340787743898637,
-0.0138907123562036));
#40194=CARTESIAN_POINT('Ctrl Pts',(-0.00173853782088977,-0.0340787743898637,
-0.014074484164648));
#40195=CARTESIAN_POINT('Ctrl Pts',(-0.00172188027006473,-0.0340787743898637,
-0.014093263310607));
#40196=CARTESIAN_POINT('Ctrl Pts',(-0.00170495136862563,-0.0340787743898636,
-0.0141118225411361));
#40197=CARTESIAN_POINT('Ctrl Pts',(-0.00168775685180314,-0.0340787743898637,
-0.0141301559522264));
#40198=CARTESIAN_POINT('Ctrl Pts',(-0.00167336442387989,-0.0340787743898637,
-0.0141455016755421));
#40199=CARTESIAN_POINT('Ctrl Pts',(-0.00165878196066412,-0.0340787743898637,
-0.0141606930102152));
#40200=CARTESIAN_POINT('Ctrl Pts',(-0.00164403551346177,-0.0340787743898637,
-0.014175703674688));
#40201=CARTESIAN_POINT('Ctrl Pts',(-0.00144997531169396,-0.0340787743898636,
-0.0143732409212044));
#40202=CARTESIAN_POINT('Ctrl Pts',(-0.00122722417391643,-0.0340787743898636,
-0.0145403352498076));
#40203=CARTESIAN_POINT('Ctrl Pts',(-0.000984003088329723,-0.0340787743898639,
-0.0146696633580869));
#40204=CARTESIAN_POINT('Ctrl Pts',(-0.000971343819170138,-0.034078774389864,
-0.0146763946796278));
#40205=CARTESIAN_POINT('Ctrl Pts',(-0.000958629164297646,-0.034078774389864,
-0.0146830225748522));
#40206=CARTESIAN_POINT('Ctrl Pts',(-0.000945871640704679,-0.034078774389864,
-0.0146895401571214));
#40207=CARTESIAN_POINT('Ctrl Pts',(-0.000862042915607934,-0.034078774389864,
-0.014732366698523));
#40208=CARTESIAN_POINT('Ctrl Pts',(-0.000776237932625443,-0.0340787743898641,
-0.0147705018511941));
#40209=CARTESIAN_POINT('Ctrl Pts',(-0.00068878756990034,-0.0340787743898642,
-0.0148036883024632));
#40210=CARTESIAN_POINT('Ctrl Pts',(-0.000652192714614692,-0.0340787743898642,
-0.0148175756477388));
#40211=CARTESIAN_POINT('Ctrl Pts',(-0.000615309219919732,-0.0340787743898643,
-0.0148305960499244));
#40212=CARTESIAN_POINT('Ctrl Pts',(-0.000578159304347232,-0.0340787743898643,
-0.0148427288545622));
#40213=CARTESIAN_POINT('Ctrl Pts',(-0.000405102583540647,-0.0340787743898646,
-0.014899247512881));
#40214=CARTESIAN_POINT('Ctrl Pts',(-0.000226292457930033,-0.0340787743898648,
-0.0149365677617328));
#40215=CARTESIAN_POINT('Ctrl Pts',(-4.4359070532995E-5,-0.034078774389865,
-0.0149557093126185));
#40216=CARTESIAN_POINT('Ctrl Pts',(-2.60444274983421E-5,-0.034078774389865,
-0.0149576362303581));
#40217=CARTESIAN_POINT('Ctrl Pts',(-7.69789496846054E-6,-0.0340787743898651,
-0.0149593782812497));
#40218=CARTESIAN_POINT('Ctrl Pts',(1.06779760546631E-5,-0.0340787743898655,
-0.0149609360713358));
#40219=CARTESIAN_POINT('Ctrl Pts',(2.82810386610846E-5,-0.0340787743898659,
-0.0149624283476137));
#40220=CARTESIAN_POINT('Ctrl Pts',(4.59139311838308E-5,-0.0340787743898658,
-0.0149637516227164));
#40221=CARTESIAN_POINT('Ctrl Pts',(6.35497484007623E-5,-0.0340787743898657,
-0.0149649050553157));
#40222=CARTESIAN_POINT('Ctrl Pts',(0.000405656097217325,-0.0340787743898652,
-0.0149872797834223));
#40223=CARTESIAN_POINT('Ctrl Pts',(0.000750534762719912,-0.0340787743898648,
-0.0149466263762361));
#40224=CARTESIAN_POINT('Ctrl Pts',(0.00108150703137315,-0.0340787743898644,
-0.0148487557072035));
#40225=CARTESIAN_POINT('Ctrl Pts',(0.00109597282815472,-0.0340787743898644,
-0.0148444780762864));
#40226=CARTESIAN_POINT('Ctrl Pts',(0.00111041391370224,-0.0340787743898644,
-0.0148400892861284));
#40227=CARTESIAN_POINT('Ctrl Pts',(0.00112482350330411,-0.0340787743898644,
-0.0148355911496298));
#40228=CARTESIAN_POINT('Ctrl Pts',(0.00140950929982585,-0.034078774389864,
-0.0147467228607084));
#40229=CARTESIAN_POINT('Ctrl Pts',(0.00167901061227646,-0.0340787743898638,
-0.0146164309612491));
#40230=CARTESIAN_POINT('Ctrl Pts',(0.00192310254496218,-0.0340787743898638,
-0.0144476154136012));
#40231=CARTESIAN_POINT('Ctrl Pts',(0.0019912392349424,-0.0340787743898637,
-0.0144004916413922));
#40232=CARTESIAN_POINT('Ctrl Pts',(0.0020573924532646,-0.0340787743898637,
-0.0143503417818491));
#40233=CARTESIAN_POINT('Ctrl Pts',(0.00212132034355962,-0.0340787743898724,
-0.0142971736301177));
#40234=CARTESIAN_POINT('Origin',(3.47714923605922E-19,-0.0340787743898723,
-0.0121758532865581));
#40235=CARTESIAN_POINT('',(-0.00300000000001,-0.0340787743898623,-0.0121758532865581));
#40236=CARTESIAN_POINT('Origin',(0.,-0.0340787743898623,-0.0121758532865581));
#40237=CARTESIAN_POINT('Ctrl Pts',(0.00299997408502258,-0.0340787743898722,
-0.0121633837535663));
#40238=CARTESIAN_POINT('Ctrl Pts',(0.00298983422017737,-0.0340787745628727,
-0.0120688605133317));
#40239=CARTESIAN_POINT('Ctrl Pts',(0.00297516577473772,-0.0340787743898748,
-0.0119748920917585));
#40240=CARTESIAN_POINT('Ctrl Pts',(0.00295613328802263,-0.0340787743898749,
-0.0118817936805995));
#40241=CARTESIAN_POINT('Ctrl Pts',(0.00291449826526791,-0.0340787743898751,
-0.011678133773985));
#40242=CARTESIAN_POINT('Ctrl Pts',(0.00285202694145493,-0.0340787743898755,
-0.0114785958149418));
#40243=CARTESIAN_POINT('Ctrl Pts',(0.00276980767921813,-0.0340787743898755,
-0.0112867975378626));
#40244=CARTESIAN_POINT('Ctrl Pts',(0.00276313869579095,-0.0340787743898755,
-0.011271240361887));
#40245=CARTESIAN_POINT('Ctrl Pts',(0.00275633938651183,-0.0340787743898755,
-0.0112557344634974));
#40246=CARTESIAN_POINT('Ctrl Pts',(0.00274941013017219,-0.0340787743898755,
-0.0112402819807807));
#40247=CARTESIAN_POINT('Ctrl Pts',(0.00274257548204977,-0.0340787743898755,
-0.01122504047768));
#40248=CARTESIAN_POINT('Ctrl Pts',(0.00273561765327543,-0.0340787743898756,
-0.0112098582491205));
#40249=CARTESIAN_POINT('Ctrl Pts',(0.00272853986062164,-0.0340787743898756,
-0.0111947423811783));
#40250=CARTESIAN_POINT('Ctrl Pts',(0.00261926295131071,-0.0340787743898758,
-0.0109613623697716));
#40251=CARTESIAN_POINT('Ctrl Pts',(0.0024813567361139,-0.0340787743898759,
-0.0107432447506426));
#40252=CARTESIAN_POINT('Ctrl Pts',(0.00231681416997636,-0.0340787743898759,
-0.0105475950993701));
#40253=CARTESIAN_POINT('Ctrl Pts',(0.00229331961457605,-0.0340787743898759,
-0.0105196588535781));
#40254=CARTESIAN_POINT('Ctrl Pts',(0.00226927930088061,-0.0340787743898759,
-0.0104921842003603));
#40255=CARTESIAN_POINT('Ctrl Pts',(0.00224469656570801,-0.0340787743898759,
-0.0104651960118044));
#40256=CARTESIAN_POINT('Ctrl Pts',(0.00214084894393267,-0.0340787743898759,
-0.0103511867619029));
#40257=CARTESIAN_POINT('Ctrl Pts',(0.00202796472163855,-0.0340787743898759,
-0.0102465484986737));
#40258=CARTESIAN_POINT('Ctrl Pts',(0.00190673318272766,-0.0340787743898759,
-0.0101531055610276));
#40259=CARTESIAN_POINT('Ctrl Pts',(0.00175487922115659,-0.0340787743898758,
-0.0100360594491834));
#40260=CARTESIAN_POINT('Ctrl Pts',(0.00158979661873312,-0.0340787743898757,
-0.00993641896279302));
#40261=CARTESIAN_POINT('Ctrl Pts',(0.00141474219894874,-0.0340787743898755,
-0.0098549840709787));
#40262=CARTESIAN_POINT('Ctrl Pts',(0.00140014729757205,-0.0340787743898755,
-0.00984819455823109));
#40263=CARTESIAN_POINT('Ctrl Pts',(0.00138548304086077,-0.0340787743898755,
-0.00984153210814379));
#40264=CARTESIAN_POINT('Ctrl Pts',(0.00137075131632936,-0.0340787743898755,
-0.00983499746591276));
#40265=CARTESIAN_POINT('Ctrl Pts',(0.00135722807646553,-0.0340787743898755,
-0.00982899887870553));
#40266=CARTESIAN_POINT('Ctrl Pts',(0.00134365490868854,-0.0340787743898755,
-0.00982311109996221));
#40267=CARTESIAN_POINT('Ctrl Pts',(0.00133003924889329,-0.0340787743898755,
-0.0098173367535274));
#40268=CARTESIAN_POINT('Ctrl Pts',(0.00105134533856905,-0.0340787743898752,
-0.00969914378956656));
#40269=CARTESIAN_POINT('Ctrl Pts',(0.000754090522326119,-0.0340787743898749,
-0.00962763092554494));
#40270=CARTESIAN_POINT('Ctrl Pts',(0.000451492268503984,-0.0340787743898744,
-0.00960616484366454));
#40271=CARTESIAN_POINT('Ctrl Pts',(0.000428385096958881,-0.0340787743898744,
-0.00960452563910818));
#40272=CARTESIAN_POINT('Ctrl Pts',(0.000405247230892682,-0.0340787743898743,
-0.00960318119938207));
#40273=CARTESIAN_POINT('Ctrl Pts',(0.000382084954837052,-0.0340787743898743,
-0.00960213448339256));
#40274=CARTESIAN_POINT('Ctrl Pts',(0.000279580069589831,-0.0340787743898742,
-0.00959750223127132));
#40275=CARTESIAN_POINT('Ctrl Pts',(0.000177094560444756,-0.0340787743898738,
-0.00959872195292196));
#40276=CARTESIAN_POINT('Ctrl Pts',(7.52901806218787E-5,-0.0340787743898741,
-0.00960590461313921));
#40277=CARTESIAN_POINT('Ctrl Pts',(-9.57122147715958E-5,-0.0340787743898747,
-0.00961796943888233));
#40278=CARTESIAN_POINT('Ctrl Pts',(-0.000264954695593333,-0.0340787743898749,
-0.00964681365331277));
#40279=CARTESIAN_POINT('Ctrl Pts',(-0.00042980566833564,-0.0340787743898751,
-0.00969349766606961));
#40280=CARTESIAN_POINT('Ctrl Pts',(-0.000487639239516593,-0.0340787743898752,
-0.00970987550800693));
#40281=CARTESIAN_POINT('Ctrl Pts',(-0.000544928777483045,-0.0340787743898753,
-0.00972845541296338));
#40282=CARTESIAN_POINT('Ctrl Pts',(-0.000601546286299631,-0.0340787743898749,
-0.00974930387114081));
#40283=CARTESIAN_POINT('Origin',(0.,-0.0340787743898623,-0.0121758532865581));
#40284=CARTESIAN_POINT('Ctrl Pts',(-0.000724274042549492,-0.0343719489147863,
-0.00925661861704697));
#40285=CARTESIAN_POINT('Ctrl Pts',(0.000248170763243804,-0.034318931779031,
-0.00901533557115846));
#40286=CARTESIAN_POINT('Ctrl Pts',(0.00243605023693017,-0.0342129076106235,
-0.00958549404345891));
#40287=CARTESIAN_POINT('Ctrl Pts',(0.00349868472071628,-0.0340538764095642,
-0.0128296735919113));
#40288=CARTESIAN_POINT('Ctrl Pts',(0.00134170352018559,-0.033894855311608,
-0.0154689316834747));
#40289=CARTESIAN_POINT('Ctrl Pts',(-0.0020430070581503,-0.033735834213652,
-0.0150874279970315));
#40290=CARTESIAN_POINT('Ctrl Pts',(-0.0035543079777708,-0.0335768131156959,
-0.0120320136823328));
#40291=CARTESIAN_POINT('Ctrl Pts',(-0.00180176699430847,-0.0334177920177398,
-0.00910923480492393));
#40292=CARTESIAN_POINT('Ctrl Pts',(0.00160421041412461,-0.0332587709197837,
-0.00900124265134754));
#40293=CARTESIAN_POINT('Ctrl Pts',(0.00353784086413984,-0.0330997498218276,
-0.0118076421117317));
#40294=CARTESIAN_POINT('Ctrl Pts',(0.00222365303830162,-0.0329407287238715,
-0.0149519682884868));
#40295=CARTESIAN_POINT('Ctrl Pts',(-0.00113172692687037,-0.0327817076259155,
-0.0155479188897315));
#40296=CARTESIAN_POINT('Ctrl Pts',(-0.00344824427242963,-0.0326226865279594,
-0.0130483563484526));
#40297=CARTESIAN_POINT('Ctrl Pts',(-0.00259931962519099,-0.0324636654300033,
-0.00974786494194555));
#40298=CARTESIAN_POINT('Ctrl Pts',(0.000635718683001802,-0.0323046443320472,
-0.0086762131723468));
#40299=CARTESIAN_POINT('Ctrl Pts',(0.00328718528952945,-0.0321456232340911,
-0.0108171659297137));
#40300=CARTESIAN_POINT('Ctrl Pts',(0.00292107726441006,-0.031986602136135,
-0.0142053653426598));
#40301=CARTESIAN_POINT('Ctrl Pts',(-0.000126521491820488,-0.0318275810381789,
-0.0157305134276381));
#40302=CARTESIAN_POINT('Ctrl Pts',(-0.0030579759603136,-0.0316685599402228,
-0.013992552104926));
#40303=CARTESIAN_POINT('Ctrl Pts',(-0.00318226944401077,-0.0315095388422667,
-0.0105868977657637));
#40304=CARTESIAN_POINT('Ctrl Pts',(-0.000385298871985522,-0.0313505177443106,
-0.00863987195853032));
#40305=CARTESIAN_POINT('Ctrl Pts',(0.00276536268907811,-0.0311914966463545,
-0.0099388107940399));
#40306=CARTESIAN_POINT('Ctrl Pts',(0.00337748671553294,-0.0310324755483984,
-0.013291305500576));
#40307=CARTESIAN_POINT('Ctrl Pts',(0.000889122011464058,-0.0308734544504424,
-0.0156198472351357));
#40308=CARTESIAN_POINT('Ctrl Pts',(-0.00241539722144602,-0.0307144333524863,
-0.0147868499547505));
#40309=CARTESIAN_POINT('Ctrl Pts',(-0.00350270981497701,-0.0305554122545302,
-0.0115570468537307));
#40310=CARTESIAN_POINT('Ctrl Pts',(-0.00137444815928839,-0.0303963911565741,
-0.00889522286003844));
#40311=CARTESIAN_POINT('Ctrl Pts',(0.00201523246796173,-0.0302373700586181,
-0.00924509377514259));
#40312=CARTESIAN_POINT('Ctrl Pts',(0.00355554012085794,-0.030078348960662,
-0.0122850754526157));
#40313=CARTESIAN_POINT('Ctrl Pts',(0.00183083526626607,-0.0299193278627059,
-0.015225310182813));
#40314=CARTESIAN_POINT('Ctrl Pts',(-0.00157243363987404,-0.0297603067647498,
-0.0153652084114242));
#40315=CARTESIAN_POINT('Ctrl Pts',(-0.00353631530869309,-0.0296012856667937,
-0.0125792758989247));
#40316=CARTESIAN_POINT('Ctrl Pts',(-0.00224571395583235,-0.0294422535936614,
-0.00941883780444782));
#40317=CARTESIAN_POINT('Ctrl Pts',(-2.28054016345844E-5,-0.0293362285531812,
-0.00900568258223235));
#40318=CARTESIAN_POINT('Ctrl Pts',(0.000930034741678471,-0.0292832105453529,
-0.00931551426486963));
#40319=CARTESIAN_POINT('Ctrl Pts',(-0.000683227961914626,-0.0342735368066846,
-0.00942205757329488));
#40320=CARTESIAN_POINT('Ctrl Pts',(0.000234106422178279,-0.0342205196709293,
-0.00919444852754381));
#40321=CARTESIAN_POINT('Ctrl Pts',(0.00229799432358602,-0.0341144955025218,
-0.00973229496150817));
#40322=CARTESIAN_POINT('Ctrl Pts',(0.00330040715348911,-0.0339554643014624,
-0.0127926202676201));
#40323=CARTESIAN_POINT('Ctrl Pts',(0.00126566645735814,-0.0337964432035063,
-0.0152823062441023));
#40324=CARTESIAN_POINT('Ctrl Pts',(-0.00192722569982459,-0.0336374221055502,
-0.0149224231462159));
#40325=CARTESIAN_POINT('Ctrl Pts',(-0.00335287812762294,-0.0334784010075941,
-0.0120401653647717));
#40326=CARTESIAN_POINT('Ctrl Pts',(-0.00169965720024032,-0.033319379909638,
-0.00928302630106875));
#40327=CARTESIAN_POINT('Ctrl Pts',(0.00151329655259554,-0.0331603588116819,
-0.00918115428211436));
#40328=CARTESIAN_POINT('Ctrl Pts',(0.00333734423875804,-0.0330013377137258,
-0.0118285093866645));
#40329=CARTESIAN_POINT('Ctrl Pts',(0.00209763410547778,-0.0328423166157698,
-0.0147946402144062));
#40330=CARTESIAN_POINT('Ctrl Pts',(-0.00106758966394507,-0.0326832955178137,
-0.0153568170849966));
#40331=CARTESIAN_POINT('Ctrl Pts',(-0.00325282526782655,-0.0325242744198576,
-0.0129989098283113));
#40332=CARTESIAN_POINT('Ctrl Pts',(-0.00245201090409445,-0.0323652533219015,
-0.00988546397148232));
#40333=CARTESIAN_POINT('Ctrl Pts',(0.000599691214404787,-0.0322062322239454,
-0.00887454488366325));
#40334=CARTESIAN_POINT('Ctrl Pts',(0.00310089382451873,-0.0320472111259893,
-0.0108941655010505));
#40335=CARTESIAN_POINT('Ctrl Pts',(0.00275553388456782,-0.0318881900280332,
-0.0140903487735019));
#40336=CARTESIAN_POINT('Ctrl Pts',(-0.000119351261976234,-0.0317291689300771,
-0.0155290636196804));
#40337=CARTESIAN_POINT('Ctrl Pts',(-0.00288467425340072,-0.0315701478321211,
-0.0138895960940694));
#40338=CARTESIAN_POINT('Ctrl Pts',(-0.00300192377299798,-0.031411126734165,
-0.0106769471015127));
#40339=CARTESIAN_POINT('Ctrl Pts',(-0.000363463202558005,-0.0312521056362089,
-0.00884026320022485));
#40340=CARTESIAN_POINT('Ctrl Pts',(0.00260864397039946,-0.0310930845382528,
-0.0100655885344216));
#40341=CARTESIAN_POINT('Ctrl Pts',(0.00318607768535292,-0.0309340634402968,
-0.013228090558674));
#40342=CARTESIAN_POINT('Ctrl Pts',(0.000838733661705831,-0.0307750423423407,
-0.0154246691050157));
#40343=CARTESIAN_POINT('Ctrl Pts',(-0.00227851175642546,-0.0306160212443846,
-0.0146388794719168));
#40344=CARTESIAN_POINT('Ctrl Pts',(-0.0033042041374851,-0.0304570001464284,
-0.01159211587077));
#40345=CARTESIAN_POINT('Ctrl Pts',(-0.00129655539127476,-0.0302979790484724,
-0.00908114284765269));
#40346=CARTESIAN_POINT('Ctrl Pts',(0.00190102515205851,-0.0301389579505163,
-0.0094111858675825));
#40347=CARTESIAN_POINT('Ctrl Pts',(0.00335404044265945,-0.0299799368525602,
-0.0122788856106888));
#40348=CARTESIAN_POINT('Ctrl Pts',(0.00172707811420276,-0.0298209157546041,
-0.0150524912685583));
#40349=CARTESIAN_POINT('Ctrl Pts',(-0.00148332063266471,-0.029661894656648,
-0.0151844611804898));
#40350=CARTESIAN_POINT('Ctrl Pts',(-0.0033359051396361,-0.0295028735586919,
-0.0125564131203294));
#40351=CARTESIAN_POINT('Ctrl Pts',(-0.00211844478601719,-0.0293438414855596,
-0.00957508346995853));
#40352=CARTESIAN_POINT('Ctrl Pts',(-2.15129732174238E-5,-0.0292378164450794,
-0.00918534259310061));
#40353=CARTESIAN_POINT('Ctrl Pts',(0.000877327784425402,-0.0291847984372511,
-0.00947761548516741));
#40354=CARTESIAN_POINT('Ctrl Pts',(-0.00064218188127976,-0.0341751246985829,
-0.00958749652954282));
#40355=CARTESIAN_POINT('Ctrl Pts',(0.000220042081112754,-0.0341221075628275,
-0.00937356148392917));
#40356=CARTESIAN_POINT('Ctrl Pts',(0.00215993841024188,-0.03401608339442,
-0.00987909587955745));
#40357=CARTESIAN_POINT('Ctrl Pts',(0.00310212958626195,-0.0338570521933608,
-0.0127555669433291));
#40358=CARTESIAN_POINT('Ctrl Pts',(0.00118962939453071,-0.0336980310954046,
-0.0150956808047299));
#40359=CARTESIAN_POINT('Ctrl Pts',(-0.00181144434149887,-0.0335390099974485,
-0.0147574182954002));
#40360=CARTESIAN_POINT('Ctrl Pts',(-0.00315144827747508,-0.0333799888994924,
-0.0120483170472104));
#40361=CARTESIAN_POINT('Ctrl Pts',(-0.00159754740617219,-0.0332209678015363,
-0.00945681779721357));
#40362=CARTESIAN_POINT('Ctrl Pts',(0.00142238269106645,-0.0330619467035802,
-0.00936106591288119));
#40363=CARTESIAN_POINT('Ctrl Pts',(0.00313684761337623,-0.0329029256056242,
-0.0118493766615973));
#40364=CARTESIAN_POINT('Ctrl Pts',(0.00197161517265394,-0.032743904507668,
-0.0146373121403257));
#40365=CARTESIAN_POINT('Ctrl Pts',(-0.00100345240101975,-0.032584883409712,
-0.0151657152802616));
#40366=CARTESIAN_POINT('Ctrl Pts',(-0.00305740626322348,-0.0324258623117559,
-0.0129494633081701));
#40367=CARTESIAN_POINT('Ctrl Pts',(-0.00230470218299792,-0.0322668412137998,
-0.0100230630010191));
#40368=CARTESIAN_POINT('Ctrl Pts',(0.000563663745807771,-0.0321078201158437,
-0.00907287659497971));
#40369=CARTESIAN_POINT('Ctrl Pts',(0.00291460235950802,-0.0319487990178876,
-0.0109711650723872));
#40370=CARTESIAN_POINT('Ctrl Pts',(0.00258999050472557,-0.0317897779199315,
-0.0139753322043438));
#40371=CARTESIAN_POINT('Ctrl Pts',(-0.000112181032131976,-0.0316307568219755,
-0.0153276138117228));
#40372=CARTESIAN_POINT('Ctrl Pts',(-0.00271137254648784,-0.0314717357240193,
-0.0137866400832125));
#40373=CARTESIAN_POINT('Ctrl Pts',(-0.00282157810198519,-0.0313127146260633,
-0.0107669964372615));
#40374=CARTESIAN_POINT('Ctrl Pts',(-0.000341627533130492,-0.0311536935281072,
-0.00904065444191939));
#40375=CARTESIAN_POINT('Ctrl Pts',(0.00245192525172084,-0.0309946724301511,
-0.0101923662748032));
#40376=CARTESIAN_POINT('Ctrl Pts',(0.00299466865517291,-0.030835651332195,
-0.0131648756167719));
#40377=CARTESIAN_POINT('Ctrl Pts',(0.000788345311947609,-0.0306766302342389,
-0.0152294909748955));
#40378=CARTESIAN_POINT('Ctrl Pts',(-0.0021416262914049,-0.0305176091362828,
-0.014490908989083));
#40379=CARTESIAN_POINT('Ctrl Pts',(-0.0031056984599932,-0.0303585880383268,
-0.0116271848878091));
#40380=CARTESIAN_POINT('Ctrl Pts',(-0.00121866262326115,-0.0301995669403707,
-0.00926706283526693));
#40381=CARTESIAN_POINT('Ctrl Pts',(0.00178681783615527,-0.0300405458424146,
-0.00957727796002242));
#40382=CARTESIAN_POINT('Ctrl Pts',(0.00315254076446096,-0.0298815247444585,
-0.012272695768762));
#40383=CARTESIAN_POINT('Ctrl Pts',(0.00162332096213945,-0.0297225036465024,
-0.0148796723543037));
#40384=CARTESIAN_POINT('Ctrl Pts',(-0.00139420762545537,-0.0295634825485463,
-0.0150037139495554));
#40385=CARTESIAN_POINT('Ctrl Pts',(-0.00313549497057911,-0.0294044614505902,
-0.012533550341734));
#40386=CARTESIAN_POINT('Ctrl Pts',(-0.00199117561620204,-0.0292454293774579,
-0.00973132913546924));
#40387=CARTESIAN_POINT('Ctrl Pts',(-2.02205448002642E-5,-0.0291394043369777,
-0.00936500260396888));
#40388=CARTESIAN_POINT('Ctrl Pts',(0.000824620827172333,-0.0290863863291494,
-0.00963971670546519));
#40389=CARTESIAN_POINT('Ctrl Pts',(-0.000601135800644895,-0.0340767125904812,
-0.00975293548579074));
#40390=CARTESIAN_POINT('Ctrl Pts',(0.000205977740047228,-0.0340236954547259,
-0.00955267444031453));
#40391=CARTESIAN_POINT('Ctrl Pts',(0.00202188249689775,-0.0339176712863184,
-0.0100258967976067));
#40392=CARTESIAN_POINT('Ctrl Pts',(0.00290385201903478,-0.033758640085259,
-0.012718513619038));
#40393=CARTESIAN_POINT('Ctrl Pts',(0.00111359233170327,-0.033599618987303,
-0.0149090553653577));
#40394=CARTESIAN_POINT('Ctrl Pts',(-0.00169566298317314,-0.0334405978893469,
-0.0145924134445845));
#40395=CARTESIAN_POINT('Ctrl Pts',(-0.00295001842732721,-0.0332815767913908,
-0.0120564687296492));
#40396=CARTESIAN_POINT('Ctrl Pts',(-0.00149543761210405,-0.0331225556934346,
-0.00963060929335837));
#40397=CARTESIAN_POINT('Ctrl Pts',(0.00133146882953737,-0.0329635345954786,
-0.009540977543648));
#40398=CARTESIAN_POINT('Ctrl Pts',(0.00293635098799442,-0.0328045134975225,
-0.0118702439365301));
#40399=CARTESIAN_POINT('Ctrl Pts',(0.0018455962398301,-0.0326454923995664,
-0.0144799840662451));
#40400=CARTESIAN_POINT('Ctrl Pts',(-0.000939315138094445,-0.0324864713016103,
-0.0149746134755266));
#40401=CARTESIAN_POINT('Ctrl Pts',(-0.0028619872586204,-0.0323274502036543,
-0.0129000167880288));
#40402=CARTESIAN_POINT('Ctrl Pts',(-0.00215739346190139,-0.0321684291056982,
-0.0101606620305559));
#40403=CARTESIAN_POINT('Ctrl Pts',(0.000527636277210757,-0.0320094080077421,
-0.00927120830629617));
#40404=CARTESIAN_POINT('Ctrl Pts',(0.00272831089449731,-0.031850386909786,
-0.0110481646437239));
#40405=CARTESIAN_POINT('Ctrl Pts',(0.00242444712488331,-0.0316913658118299,
-0.013860315635186));
#40406=CARTESIAN_POINT('Ctrl Pts',(-0.000105010802287719,-0.0315323447138738,
-0.0151261640037651));
#40407=CARTESIAN_POINT('Ctrl Pts',(-0.00253807083957495,-0.0313733236159177,
-0.0136836840723558));
#40408=CARTESIAN_POINT('Ctrl Pts',(-0.00264123243097238,-0.0312143025179616,
-0.0108570457730104));
#40409=CARTESIAN_POINT('Ctrl Pts',(-0.000319791863702978,-0.0310552814200056,
-0.00924104568361391));
#40410=CARTESIAN_POINT('Ctrl Pts',(0.00229520653304219,-0.0308962603220495,
-0.0103191440151849));
#40411=CARTESIAN_POINT('Ctrl Pts',(0.00280325962499289,-0.0307372392240933,
-0.0131016606748699));
#40412=CARTESIAN_POINT('Ctrl Pts',(0.000737956962189381,-0.0305782181261372,
-0.0150343128447755));
#40413=CARTESIAN_POINT('Ctrl Pts',(-0.00200474082638433,-0.0304191970281811,
-0.0143429385062493));
#40414=CARTESIAN_POINT('Ctrl Pts',(-0.0029071927825013,-0.0302601759302251,
-0.0116622539048482));
#40415=CARTESIAN_POINT('Ctrl Pts',(-0.00114076985524752,-0.030101154832269,
-0.00945298282288118));
#40416=CARTESIAN_POINT('Ctrl Pts',(0.00167261052025204,-0.0299421337343129,
-0.00974337005246235));
#40417=CARTESIAN_POINT('Ctrl Pts',(0.00295104108626248,-0.0297831126363568,
-0.012266505926835));
#40418=CARTESIAN_POINT('Ctrl Pts',(0.00151956381007614,-0.0296240915384008,
-0.014706853440049));
#40419=CARTESIAN_POINT('Ctrl Pts',(-0.00130509461824602,-0.0294650704404447,
-0.014822966718621));
#40420=CARTESIAN_POINT('Ctrl Pts',(-0.00293508480152213,-0.0293060493424886,
-0.0125106875631388));
#40421=CARTESIAN_POINT('Ctrl Pts',(-0.00186390644638689,-0.0291470172693563,
-0.00988757480097995));
#40422=CARTESIAN_POINT('Ctrl Pts',(-1.89281163831043E-5,-0.029040992228876,
-0.00954466261483715));
#40423=CARTESIAN_POINT('Ctrl Pts',(0.000771913869919264,-0.0289879742210478,
-0.00980181792576297));
#40424=CARTESIAN_POINT('Ctrl Pts',(-0.00249512019792405,-0.029278774389874,
-0.0120001969329541));
#40425=CARTESIAN_POINT('Ctrl Pts',(-0.00250451942578934,-0.0292787743898746,
-0.0116746048596339));
#40426=CARTESIAN_POINT('Ctrl Pts',(-0.00244956820908934,-0.029278774389875,
-0.0113485528346615));
#40427=CARTESIAN_POINT('Ctrl Pts',(-0.00233887355507737,-0.0292787743898753,
-0.0110396898663454));
#40428=CARTESIAN_POINT('Ctrl Pts',(-0.0023342889065707,-0.0292787743898753,
-0.011026897666405));
#40429=CARTESIAN_POINT('Ctrl Pts',(-0.00232960758938224,-0.0292787743898754,
-0.0110141358510404));
#40430=CARTESIAN_POINT('Ctrl Pts',(-0.00232483460901268,-0.0292787743898754,
-0.0110014176248355));
#40431=CARTESIAN_POINT('Ctrl Pts',(-0.00222580382029312,-0.0292787743898756,
-0.0107375372241906));
#40432=CARTESIAN_POINT('Ctrl Pts',(-0.00208719432964695,-0.0292787743898758,
-0.0104910173381353));
#40433=CARTESIAN_POINT('Ctrl Pts',(-0.00191326911752999,-0.0292787743898759,
-0.0102724976348523));
#40434=CARTESIAN_POINT('Ctrl Pts',(-0.00189637749193036,-0.0292787743898759,
-0.0102512749899633));
#40435=CARTESIAN_POINT('Ctrl Pts',(-0.00187914941593776,-0.0292787743898759,
-0.0102303172981295));
#40436=CARTESIAN_POINT('Ctrl Pts',(-0.00186158669131192,-0.0292787743898759,
-0.0102096351284549));
#40437=CARTESIAN_POINT('Ctrl Pts',(-0.00184648594129761,-0.0292787743898759,
-0.01019185222286));
#40438=CARTESIAN_POINT('Ctrl Pts',(-0.00183113778395428,-0.0292787743898759,
-0.010174273010336));
#40439=CARTESIAN_POINT('Ctrl Pts',(-0.00181554315970928,-0.0292787743898759,
-0.0101569043754393));
#40440=CARTESIAN_POINT('Ctrl Pts',(-0.00180724793405888,-0.0292787743898759,
-0.0101476655028994));
#40441=CARTESIAN_POINT('Ctrl Pts',(-0.00179888407649718,-0.0292787743898759,
-0.0101384875200101));
#40442=CARTESIAN_POINT('Ctrl Pts',(-0.00179045824703803,-0.0292787743898759,
-0.0101293782351649));
#40443=CARTESIAN_POINT('Ctrl Pts',(-0.00176932982413912,-0.0292787743898759,
-0.0101065359947126));
#40444=CARTESIAN_POINT('Ctrl Pts',(-0.00174780084142207,-0.0292787743898759,
-0.0100841134776088));
#40445=CARTESIAN_POINT('Ctrl Pts',(-0.0017258778551185,-0.0292787743898759,
-0.0100621241575538));
#40446=CARTESIAN_POINT('Ctrl Pts',(-0.00129914862071067,-0.029278774389876,
-0.00963410374179902));
#40447=CARTESIAN_POINT('Ctrl Pts',(-0.00072150280878173,-0.0292787743898755,
-0.00936613739934554));
#40448=CARTESIAN_POINT('Ctrl Pts',(-0.000116750728983814,-0.0292787743898747,
-0.00928163047214553));
#40449=CARTESIAN_POINT('Ctrl Pts',(-9.8096741933677E-5,-0.0292787743898747,
-0.00927902379880236));
#40450=CARTESIAN_POINT('Ctrl Pts',(-7.94118191834939E-5,-0.0292787743898746,
-0.00927659177262819));
#40451=CARTESIAN_POINT('Ctrl Pts',(-6.06985211378466E-5,-0.0292787743898746,
-0.00927433533713099));
#40452=CARTESIAN_POINT('Ctrl Pts',(-4.47341024448895E-5,-0.0292787743898746,
-0.00927241035945239));
#40453=CARTESIAN_POINT('Ctrl Pts',(-2.87488940363722E-5,-0.0292787743898746,
-0.00927061324069165));
#40454=CARTESIAN_POINT('Ctrl Pts',(-1.27594804140441E-5,-0.0292787743898745,
-0.0092689459349433));
#40455=CARTESIAN_POINT('Ctrl Pts',(8.69557107774587E-5,-0.0292787743898736,
-0.00925854807324565));
#40456=CARTESIAN_POINT('Ctrl Pts',(0.000186975259284375,-0.029278774389874,
-0.00925317714695822));
#40457=CARTESIAN_POINT('Ctrl Pts',(0.000286891956576391,-0.0292787743898741,
-0.00925288394665933));
#40458=CARTESIAN_POINT('Ctrl Pts',(0.000484391186557055,-0.0292787743898744,
-0.00925230439554493));
#40459=CARTESIAN_POINT('Ctrl Pts',(0.000681486279184165,-0.0292787743898747,
-0.00927151228708075));
#40460=CARTESIAN_POINT('Ctrl Pts',(0.000875206702308309,-0.0292787743898749,
-0.0093114725913186));
#40461=CARTESIAN_POINT('Ctrl Pts',(0.000892515753144813,-0.0292787743898749,
-0.00931504307153096));
#40462=CARTESIAN_POINT('Ctrl Pts',(0.000909797888585897,-0.029278774389875,
-0.00931877977997034));
#40463=CARTESIAN_POINT('Ctrl Pts',(0.000927050983124846,-0.0292787743898723,
-0.00932268373767265));
#40464=CARTESIAN_POINT('Origin',(0.,-0.0292787743898723,-0.0121758532865581));
#40465=CARTESIAN_POINT('',(0.001475,-0.0292787743898623,-0.0121758532865581));
#40466=CARTESIAN_POINT('Origin',(0.,-0.0292787743898623,-0.0121758532865581));
#40467=CARTESIAN_POINT('Origin',(0.,-0.0341787743898723,-0.0121758532865581));
#40468=CARTESIAN_POINT('',(-0.0029,-0.0341787743898723,-0.0121758532865581));
#40469=CARTESIAN_POINT('Origin',(0.,-0.0271787743898723,-0.0121758532865581));
#40470=CARTESIAN_POINT('',(0.001475,-0.0271787743898623,-0.0121758532865581));
#40471=CARTESIAN_POINT('Origin',(0.,-0.0271787743898623,-0.0121758532865581));
#40472=CARTESIAN_POINT('Origin',(0.,-0.0292787743898723,-0.0121758532865581));
#40473=CARTESIAN_POINT('',(0.001475,-0.0292787743898723,-0.0121758532865581));
#40474=CARTESIAN_POINT('',(0.,0.,0.));
#40475=CARTESIAN_POINT('Origin',(-0.0065,-0.0372787743898723,-0.00237585328655808));
#40476=CARTESIAN_POINT('',(-0.00597905546699748,-0.0343243511308258,-0.00257585328656808));
#40477=CARTESIAN_POINT('Origin',(-0.0065,-0.0372787743898723,-0.00257585328656808));
#40478=CARTESIAN_POINT('',(-0.00604851473806512,-0.0347182742320356,-0.00217585328656308));
#40479=CARTESIAN_POINT('',(-0.0060137851025326,-0.0345213126814381,-0.00237585328655808));
#40480=CARTESIAN_POINT('Origin',(-0.0065,-0.0372787743898723,-0.00217585328655808));
#40481=CARTESIAN_POINT('Origin',(-0.0065,-0.0372787743898723,-0.00217585328655808));
#40482=CARTESIAN_POINT('',(-0.00597905546699935,-0.0343243511308356,-0.0217758532865681));
#40483=CARTESIAN_POINT('Origin',(-0.00650000000000013,-0.0372787743898722,
-0.0217758532865681));
#40484=CARTESIAN_POINT('',(-0.00597905546699922,-0.0343243511308357,-0.00217585328655808));
#40485=CARTESIAN_POINT('Origin',(-0.0065,-0.0372787743898723,-0.00217585328655808));
#40486=CARTESIAN_POINT('Origin',(-0.00650000000000013,-0.0372787743898722,
-0.0219758532865581));
#40487=CARTESIAN_POINT('',(-0.00604851473806612,-0.0347182742320405,-0.0221758532865581));
#40488=CARTESIAN_POINT('',(-0.00601378510253273,-0.034521312681438,-0.0219758532865581));
#40489=CARTESIAN_POINT('Origin',(-0.00650000000000013,-0.0372787743898722,
-0.0221758532865681));
#40490=CARTESIAN_POINT('Origin',(-0.00650000000000013,-0.0372787743898722,
-0.0221758532865581));
#40491=CARTESIAN_POINT('',(0.,0.,0.));
#40492=CARTESIAN_POINT('Origin',(0.,-0.0397787743898723,-0.0121758532865581));
#40493=CARTESIAN_POINT('',(0.0025,-0.0342786793591244,-0.0121758532865055));
#40494=CARTESIAN_POINT('',(0.0025,-0.0341527041915604,-0.0121758532865581));
#40495=CARTESIAN_POINT('',(0.0025,-0.0397787743898723,-0.0121758532865581));
#40496=CARTESIAN_POINT('',(-0.000771312791324951,-0.0339793475320778,-0.0145540428435752));
#40497=CARTESIAN_POINT('Ctrl Pts',(0.0025,-0.0342786793591244,-0.0121758532864529));
#40498=CARTESIAN_POINT('Ctrl Pts',(0.00250000000000589,-0.0342689904458182,
-0.012315775198942));
#40499=CARTESIAN_POINT('Ctrl Pts',(0.0024882531961583,-0.03425938869533,
-0.0124554668616244));
#40500=CARTESIAN_POINT('Ctrl Pts',(0.00245824343412142,-0.0342474763671746,
-0.0126325974120151));
#40501=CARTESIAN_POINT('Ctrl Pts',(0.00245068049935161,-0.0342448700864197,
-0.0126715763414618));
#40502=CARTESIAN_POINT('Ctrl Pts',(0.00243407926704808,-0.0342398266543392,
-0.0127474282739024));
#40503=CARTESIAN_POINT('Ctrl Pts',(0.0024251232527868,-0.0342373877758851,
-0.0127843081361286));
#40504=CARTESIAN_POINT('Ctrl Pts',(0.0024062581256887,-0.0342327386782671,
-0.012854939410854));
#40505=CARTESIAN_POINT('Ctrl Pts',(0.00239646964780489,-0.0342305253471382,
-0.012888713407758));
#40506=CARTESIAN_POINT('Ctrl Pts',(0.00237353483867019,-0.0342257364384091,
-0.0129620259747392));
#40507=CARTESIAN_POINT('Ctrl Pts',(0.00236010594404936,-0.0342231702677575,
-0.0130014653944082));
#40508=CARTESIAN_POINT('Ctrl Pts',(0.00228201403663924,-0.0342094074385763,
-0.0132133077892516));
#40509=CARTESIAN_POINT('Ctrl Pts',(0.00219944277765854,-0.0341988025597235,
-0.0133784991150409));
#40510=CARTESIAN_POINT('Ctrl Pts',(0.00205806083183455,-0.0341835935557079,
-0.0135971921576275));
#40511=CARTESIAN_POINT('Ctrl Pts',(0.00201373970870775,-0.0341791135405407,
-0.0136593187322613));
#40512=CARTESIAN_POINT('Ctrl Pts',(0.0019362578023308,-0.0341715671202833,
-0.0137580445391356));
#40513=CARTESIAN_POINT('Ctrl Pts',(0.00190472966789206,-0.0341685641590388,
-0.0137958618265926));
#40514=CARTESIAN_POINT('Ctrl Pts',(0.0018566129956555,-0.0341640369097395,
-0.0138502292345201));
#40515=CARTESIAN_POINT('Ctrl Pts',(0.00184087370293039,-0.0341625642386274,
-0.0138675183084103));
#40516=CARTESIAN_POINT('Ctrl Pts',(0.00181091273694596,-0.0341597704547133,
-0.0138995161157817));
#40517=CARTESIAN_POINT('Ctrl Pts',(0.00179674876761949,-0.0341584531897357,
-0.0139142756312608));
#40518=CARTESIAN_POINT('Ctrl Pts',(0.00175949581676491,-0.0341550009644654,
-0.013952153369971));
#40519=CARTESIAN_POINT('Ctrl Pts',(0.00173613226008321,-0.034152848006073,
-0.0139749953224846));
#40520=CARTESIAN_POINT('Ctrl Pts',(0.00163589223795456,-0.0341436854154029,
-0.0140692265481607));
#40521=CARTESIAN_POINT('Ctrl Pts',(0.001555013442751,-0.034136476184694,
-0.014136194036011));
#40522=CARTESIAN_POINT('Ctrl Pts',(0.0013291054312484,-0.0341172236228441,
-0.0143004472511144));
#40523=CARTESIAN_POINT('Ctrl Pts',(0.00117766921487138,-0.0341052282652209,
-0.0143879862814541));
#40524=CARTESIAN_POINT('Ctrl Pts',(0.000979632848000693,-0.0340909598460285,
-0.0144763131149805));
#40525=CARTESIAN_POINT('Ctrl Pts',(0.000940495075546564,-0.034088201164009,
-0.0144925891993804));
#40526=CARTESIAN_POINT('Ctrl Pts',(0.000867704679218025,-0.0340831794288103,
-0.0145207114094512));
#40527=CARTESIAN_POINT('Ctrl Pts',(0.0008341765775287,-0.0340809077905754,
-0.0145328472763923));
#40528=CARTESIAN_POINT('Ctrl Pts',(0.000763952075201242,-0.0340762311916867,
-0.0145565795024953));
#40529=CARTESIAN_POINT('Ctrl Pts',(0.000727224320919134,-0.0340738305391452,
-0.0145680541811659));
#40530=CARTESIAN_POINT('Ctrl Pts',(0.000625046771656675,-0.0340672651317129,
-0.0145974061125373));
#40531=CARTESIAN_POINT('Ctrl Pts',(0.000559110111740278,-0.0340631556915915,
-0.0146134747813474));
#40532=CARTESIAN_POINT('Ctrl Pts',(0.000401109210603117,-0.0340535311559656,
-0.0146452296313665));
#40533=CARTESIAN_POINT('Ctrl Pts',(0.000308660024066335,-0.0340480770336272,
-0.014658480624984));
#40534=CARTESIAN_POINT('Ctrl Pts',(5.58935546999585E-5,-0.0340333072623739,
-0.0146803692307144));
#40535=CARTESIAN_POINT('Ctrl Pts',(-0.000104838370947314,-0.0340240796632803,
-0.0146787958023007));
#40536=CARTESIAN_POINT('Ctrl Pts',(-0.000294387272717696,-0.0340123627511266,
-0.0146586444962111));
#40537=CARTESIAN_POINT('Ctrl Pts',(-0.000324421993547556,-0.0340104803134344,
-0.014654898715805));
#40538=CARTESIAN_POINT('Ctrl Pts',(-0.000373766720059421,-0.03400733424197,
-0.0146478326555677));
#40539=CARTESIAN_POINT('Ctrl Pts',(-0.000393119631909072,-0.0340060867513739,
-0.0146448288749355));
#40540=CARTESIAN_POINT('Ctrl Pts',(-0.000429560748455838,-0.0340037086988993,
-0.014638733526942));
#40541=CARTESIAN_POINT('Ctrl Pts',(-0.000446656034600929,-0.0340025809444483,
-0.0146356906499663));
#40542=CARTESIAN_POINT('Ctrl Pts',(-0.00048558309599664,-0.0339999873585239,
-0.0146283426737115));
#40543=CARTESIAN_POINT('Ctrl Pts',(-0.000507391694341714,-0.0339985158478622,
-0.0146239236953516));
#40544=CARTESIAN_POINT('Ctrl Pts',(-0.000610902259790336,-0.0339914527156919,
-0.01460150731064));
#40545=CARTESIAN_POINT('Ctrl Pts',(-0.000691719849745892,-0.033985704795299,
-0.0145797085697862));
#40546=CARTESIAN_POINT('Ctrl Pts',(-0.00077128512462153,-0.0339799013909928,
-0.0145539027512534));
#40547=CARTESIAN_POINT('',(0.00113497624934891,-0.0339787743898723,-0.014403369597029));
#40548=CARTESIAN_POINT('Origin',(0.,-0.0339787743898823,-0.0121758532865581));
#40549=CARTESIAN_POINT('Ctrl Pts',(0.00113497624934886,-0.0339787743898723,
-0.014403369597029));
#40550=CARTESIAN_POINT('Ctrl Pts',(0.00115174305302593,-0.0339799723697356,
-0.0143948264838489));
#40551=CARTESIAN_POINT('Ctrl Pts',(0.00116840353974554,-0.033981179169348,
-0.0143860992538718));
#40552=CARTESIAN_POINT('Ctrl Pts',(0.00120623568276769,-0.0339839550642577,
-0.0143657342481842));
#40553=CARTESIAN_POINT('Ctrl Pts',(0.00122733150122625,-0.0339855287333036,
-0.0143539810279024));
#40554=CARTESIAN_POINT('Ctrl Pts',(0.00136073400405712,-0.0339956332509063,
-0.0142771044776625));
#40555=CARTESIAN_POINT('Ctrl Pts',(0.00146798869649448,-0.034004448180033,
-0.0142036252280775));
#40556=CARTESIAN_POINT('Ctrl Pts',(0.00167396607523132,-0.0340223545464033,
-0.01403757293468));
#40557=CARTESIAN_POINT('Ctrl Pts',(0.00177188415327335,-0.0340314110851452,
-0.0139446369443402));
#40558=CARTESIAN_POINT('Ctrl Pts',(0.00189306870728335,-0.0340432617355753,
-0.0138094017792567));
#40559=CARTESIAN_POINT('Ctrl Pts',(0.00192331473162106,-0.0340462837571465,
-0.0137736801397658));
#40560=CARTESIAN_POINT('Ctrl Pts',(0.00197664900583011,-0.0340517359007246,
-0.0137069799400376));
#40561=CARTESIAN_POINT('Ctrl Pts',(0.00200005576914848,-0.0340541762926233,
-0.0136762756519943));
#40562=CARTESIAN_POINT('Ctrl Pts',(0.00205136640329276,-0.0340596418664449,
-0.0136056323496693));
#40563=CARTESIAN_POINT('Ctrl Pts',(0.00207883326513204,-0.0340626516850083,
-0.0135653945751912));
#40564=CARTESIAN_POINT('Ctrl Pts',(0.00217624493939696,-0.0340736790003726,
-0.0134133305290349));
#40565=CARTESIAN_POINT('Ctrl Pts',(0.00223848717160619,-0.0340814420427912,
-0.0132968227129049));
#40566=CARTESIAN_POINT('Ctrl Pts',(0.00235851704548095,-0.0340988979417139,
-0.0130218272845133));
#40567=CARTESIAN_POINT('Ctrl Pts',(0.0024100572343524,-0.0341084849121217,
-0.0128613378466486));
#40568=CARTESIAN_POINT('Ctrl Pts',(0.0024545293322669,-0.0341213685515389,
-0.0126526484567885));
#40569=CARTESIAN_POINT('Ctrl Pts',(0.00246275705248113,-0.0341241409621192,
-0.0126081437409061));
#40570=CARTESIAN_POINT('Ctrl Pts',(0.00247331312517072,-0.0341283990194741,
-0.0125408791313476));
#40571=CARTESIAN_POINT('Ctrl Pts',(0.00247654466224529,-0.0341298417895595,
-0.0125182684277932));
#40572=CARTESIAN_POINT('Ctrl Pts',(0.00248195972464071,-0.034132547103682,
-0.0124762798085279));
#40573=CARTESIAN_POINT('Ctrl Pts',(0.0024842270701644,-0.0341338054021254,
-0.0124569154713321));
#40574=CARTESIAN_POINT('Ctrl Pts',(0.00248947277206638,-0.0341370706641842,
-0.0124070738843198));
#40575=CARTESIAN_POINT('Ctrl Pts',(0.00249211791730572,-0.0341390940066405,
-0.0123765663429026));
#40576=CARTESIAN_POINT('Ctrl Pts',(0.00249806805641862,-0.0341449339347089,
-0.0122893525724859));
#40577=CARTESIAN_POINT('Ctrl Pts',(0.0025,-0.0341488010148688,-0.0122325976807982));
#40578=CARTESIAN_POINT('Ctrl Pts',(0.0025,-0.0341527041915604,-0.0121758532865581));
#40579=CARTESIAN_POINT('Origin',(0.,-0.0397787743898723,-0.0121758532865581));
#40580=CARTESIAN_POINT('',(0.0025,-0.0352796511099541,-0.0121758532865581));
#40581=CARTESIAN_POINT('',(0.0025,-0.0351559292844039,-0.0121758532867805));
#40582=CARTESIAN_POINT('',(0.0025,-0.0397787743898723,-0.0121758532865581));
#40583=CARTESIAN_POINT('',(0.00249999913488366,-0.0342788233790735,-0.0121737734834589));
#40584=CARTESIAN_POINT('Ctrl Pts',(0.0025,-0.0352796511099541,-0.0121758532865581));
#40585=CARTESIAN_POINT('Ctrl Pts',(0.0025,-0.0352737283576379,-0.0122771833963633));
#40586=CARTESIAN_POINT('Ctrl Pts',(0.00249383929029918,-0.0352677434542228,
-0.0123784711776437));
#40587=CARTESIAN_POINT('Ctrl Pts',(0.00247798453785767,-0.0352596957712184,
-0.0125081910504146));
#40588=CARTESIAN_POINT('Ctrl Pts',(0.0024739263012976,-0.0352578733696817,
-0.0125371623558298));
#40589=CARTESIAN_POINT('Ctrl Pts',(0.00246625181006756,-0.0352547661812909,
-0.012585729857012));
#40590=CARTESIAN_POINT('Ctrl Pts',(0.00246290802346204,-0.0352534952910727,
-0.0126053656031181));
#40591=CARTESIAN_POINT('Ctrl Pts',(0.00245492731469495,-0.0352506316714374,
-0.0126490683004793));
#40592=CARTESIAN_POINT('Ctrl Pts',(0.00245017084734073,-0.0352490333102353,
-0.0126731090348513));
#40593=CARTESIAN_POINT('Ctrl Pts',(0.00243316671274258,-0.0352436613680692,
-0.0127528758109736));
#40594=CARTESIAN_POINT('Ctrl Pts',(0.00241936555138658,-0.0352398204035837,
-0.0128082492058634));
#40595=CARTESIAN_POINT('Ctrl Pts',(0.00237669656419295,-0.0352292423937706,
-0.0129574868825818));
#40596=CARTESIAN_POINT('Ctrl Pts',(0.00234417392000077,-0.035222425284202,
-0.0130502017176979));
#40597=CARTESIAN_POINT('Ctrl Pts',(0.0022507778016247,-0.0352056799802343,
-0.0132734335079112));
#40598=CARTESIAN_POINT('Ctrl Pts',(0.00218391902487044,-0.0351958229917732,
-0.0134010841390569));
#40599=CARTESIAN_POINT('Ctrl Pts',(0.00207961062791622,-0.0351830183298481,
-0.0135642704148632));
#40600=CARTESIAN_POINT('Ctrl Pts',(0.00205152600405622,-0.0351797661256388,
-0.0136054420740379));
#40601=CARTESIAN_POINT('Ctrl Pts',(0.00200149225271985,-0.0351742874609104,
-0.0136742766385462));
#40602=CARTESIAN_POINT('Ctrl Pts',(0.00198015446319433,-0.0351720395367643,
-0.0137023631235021));
#40603=CARTESIAN_POINT('Ctrl Pts',(0.00193462116135819,-0.035167417151577,
-0.0137597355675134));
#40604=CARTESIAN_POINT('Ctrl Pts',(0.00191033808636,-0.0351650468422292,
-0.0137889406221594));
#40605=CARTESIAN_POINT('Ctrl Pts',(0.00184171873199297,-0.0351585918204036,
-0.0138677446077711));
#40606=CARTESIAN_POINT('Ctrl Pts',(0.00179605271034649,-0.0351545604975022,
-0.0139161463236));
#40607=CARTESIAN_POINT('Ctrl Pts',(0.00168346872446355,-0.0351451479767051,
-0.0140263163891485));
#40608=CARTESIAN_POINT('Ctrl Pts',(0.00161500103908194,-0.0351398245317568,
-0.0140863646356792));
#40609=CARTESIAN_POINT('Ctrl Pts',(0.00141402858550948,-0.0351249456416134,
-0.0142440824138003));
#40610=CARTESIAN_POINT('Ctrl Pts',(0.00127496011407219,-0.0351154935490178,
-0.0143325897878295));
#40611=CARTESIAN_POINT('Ctrl Pts',(0.00110211596984762,-0.035103566079878,
-0.0144200005206734));
#40612=CARTESIAN_POINT('Ctrl Pts',(0.00107577231503863,-0.0351017429892431,
-0.0144327472083214));
#40613=CARTESIAN_POINT('Ctrl Pts',(0.00103112294808702,-0.035098634490036,
-0.0144533920129587));
#40614=CARTESIAN_POINT('Ctrl Pts',(0.00101293599230588,-0.035097362978955,
-0.0144615387040784));
#40615=CARTESIAN_POINT('Ctrl Pts',(0.000972145703499203,-0.0350944971059487,
-0.0144792278873622));
#40616=CARTESIAN_POINT('Ctrl Pts',(0.00094949746231122,-0.0350928970920234,
-0.0144886559759031));
#40617=CARTESIAN_POINT('Ctrl Pts',(0.000873621012950118,-0.0350875161348841,
-0.0145189397930628));
#40618=CARTESIAN_POINT('Ctrl Pts',(0.000819819391895106,-0.0350836676083418,
-0.0145383018546116));
#40619=CARTESIAN_POINT('Ctrl Pts',(0.00067160987331214,-0.0350730578694784,
-0.0145859669385363));
#40620=CARTESIAN_POINT('Ctrl Pts',(0.000576115457086386,-0.0350662162401795,
-0.0146105601551931));
#40621=CARTESIAN_POINT('Ctrl Pts',(0.000338965597307982,-0.0350494977406898,
-0.0146568981415619));
#40622=CARTESIAN_POINT('Ctrl Pts',(0.00019639562575315,-0.0350396915727571,
-0.0146722346199108));
#40623=CARTESIAN_POINT('Ctrl Pts',(3.48141957141785E-6,-0.0350269350471675,
-0.0146763470457643));
#40624=CARTESIAN_POINT('Ctrl Pts',(-4.63416875190967E-5,-0.0350236838617148,
-0.0146759201192626));
#40625=CARTESIAN_POINT('Ctrl Pts',(-0.00013137431303332,-0.0350182055133934,
-0.0146726483072451));
#40626=CARTESIAN_POINT('Ctrl Pts',(-0.000166595580792309,-0.0350159569371864,
-0.0146705457924425));
#40627=CARTESIAN_POINT('Ctrl Pts',(-0.000239647539862756,-0.0350113318197795,
-0.0146646308536982));
#40628=CARTESIAN_POINT('Ctrl Pts',(-0.000277459625399993,-0.0350089594621896,
-0.0146606995831));
#40629=CARTESIAN_POINT('Ctrl Pts',(-0.000381286172679116,-0.0350024942746665,
-0.0146475051500353));
#40630=CARTESIAN_POINT('Ctrl Pts',(-0.000447044344062764,-0.0349984550887338,
-0.0146364618499308));
#40631=CARTESIAN_POINT('Ctrl Pts',(-0.000601625458324209,-0.0349890187403755,
-0.0146040991616407));
#40632=CARTESIAN_POINT('Ctrl Pts',(-0.000689876192816882,-0.0349836797591199,
-0.0145805161311376));
#40633=CARTESIAN_POINT('Ctrl Pts',(-0.000932425387999368,-0.0349688188016036,
-0.0145012443159997));
#40634=CARTESIAN_POINT('Ctrl Pts',(-0.00108280541376209,-0.0349593977567418,
-0.0144351408233916));
#40635=CARTESIAN_POINT('Ctrl Pts',(-0.00125118423705539,-0.0349475026601224,
-0.0143404314239675));
#40636=CARTESIAN_POINT('Ctrl Pts',(-0.0012764952656036,-0.0349456754142555,
-0.01432560214918));
#40637=CARTESIAN_POINT('Ctrl Pts',(-0.00131855085643177,-0.034942562968225,
-0.0142999579646947));
#40638=CARTESIAN_POINT('Ctrl Pts',(-0.0013354371943393,-0.0349412917973962,
-0.0142893822109742));
#40639=CARTESIAN_POINT('Ctrl Pts',(-0.00137275373997812,-0.0349384322130194,
-0.0142653854200478));
#40640=CARTESIAN_POINT('Ctrl Pts',(-0.0013931152808018,-0.0349368382684344,
-0.014251865587376));
#40641=CARTESIAN_POINT('Ctrl Pts',(-0.00146001580243708,-0.0349314968683617,
-0.0142060170070799));
#40642=CARTESIAN_POINT('Ctrl Pts',(-0.00150565126222838,-0.0349276829321327,
-0.0141724063642376));
#40643=CARTESIAN_POINT('Ctrl Pts',(-0.00162619100530393,-0.0349172144971981,
-0.0140771445083684));
#40644=CARTESIAN_POINT('Ctrl Pts',(-0.00169871417846689,-0.0349104814565078,
-0.0140126370325997));
#40645=CARTESIAN_POINT('Ctrl Pts',(-0.0018702580661283,-0.0348936947865843,
-0.0138411828317261));
#40646=CARTESIAN_POINT('Ctrl Pts',(-0.00196404013687724,-0.0348837131726053,
-0.0137294762447948));
#40647=CARTESIAN_POINT('Ctrl Pts',(-0.00207615499489246,-0.0348707937864232,
-0.0135694320090113));
#40648=CARTESIAN_POINT('Ctrl Pts',(-0.00210351034160456,-0.0348675423799178,
-0.0135277874646796));
#40649=CARTESIAN_POINT('Ctrl Pts',(-0.0021480636276629,-0.0348620662428828,
-0.0134553315183505));
#40650=CARTESIAN_POINT('Ctrl Pts',(-0.00216588647483754,-0.0348598200184832,
-0.0134249240903401));
#40651=CARTESIAN_POINT('Ctrl Pts',(-0.00220154332330296,-0.0348552024123791,
-0.0133610306533227));
#40652=CARTESIAN_POINT('Ctrl Pts',(-0.00221927013416792,-0.0348528351504397,
-0.0133274950296997));
#40653=CARTESIAN_POINT('Ctrl Pts',(-0.00226589133500932,-0.0348463933289219,
-0.013234219293502));
#40654=CARTESIAN_POINT('Ctrl Pts',(-0.00229318207892717,-0.0348423718817109,
-0.0131737105690229));
#40655=CARTESIAN_POINT('Ctrl Pts',(-0.00235198570859494,-0.0348329897712581,
-0.0130281328476765));
#40656=CARTESIAN_POINT('Ctrl Pts',(-0.0023813413657695,-0.0348276863615184,
-0.0129422943152839));
#40657=CARTESIAN_POINT('Ctrl Pts',(-0.00245089171485022,-0.0348127771057478,
-0.0126959199882142));
#40658=CARTESIAN_POINT('Ctrl Pts',(-0.00247990987111939,-0.0348032782901581,
-0.0125327474543379));
#40659=CARTESIAN_POINT('Ctrl Pts',(-0.00249485035638801,-0.0347913016097072,
-0.012338861396878));
#40660=CARTESIAN_POINT('Ctrl Pts',(-0.00249658151021034,-0.0347894851826981,
-0.0123097582443375));
#40661=CARTESIAN_POINT('Ctrl Pts',(-0.00249863727622723,-0.0347863853039192,
-0.0122607516109443));
#40662=CARTESIAN_POINT('Ctrl Pts',(-0.00249923381653334,-0.0347851156123171,
-0.012240862990334));
#40663=CARTESIAN_POINT('Ctrl Pts',(-0.00250003567650427,-0.0347822511558717,
-0.0121964359270043));
#40664=CARTESIAN_POINT('Ctrl Pts',(-0.00250011725465795,-0.0347806506849812,
-0.0121718995581665));
#40665=CARTESIAN_POINT('Ctrl Pts',(-0.00249918491759101,-0.0347752606909682,
-0.0120900812205439));
#40666=CARTESIAN_POINT('Ctrl Pts',(-0.00249656323300301,-0.0347714031510676,
-0.0120328388236775));
#40667=CARTESIAN_POINT('Ctrl Pts',(-0.00248406381804999,-0.0347607589941701,
-0.0118771843812791));
#40668=CARTESIAN_POINT('Ctrl Pts',(-0.00247030979190908,-0.0347538912629718,
-0.0117791864073395));
#40669=CARTESIAN_POINT('Ctrl Pts',(-0.00242253787305385,-0.0347371464752765,
-0.0115419875563959));
#40670=CARTESIAN_POINT('Ctrl Pts',(-0.00238229176058288,-0.0347273403432799,
-0.0114043798598893));
#40671=CARTESIAN_POINT('Ctrl Pts',(-0.0023124426663361,-0.034714581181683,
-0.0112244890987779));
#40672=CARTESIAN_POINT('Ctrl Pts',(-0.00229301275046583,-0.0347113272335813,
-0.0111785679759999));
#40673=CARTESIAN_POINT('Ctrl Pts',(-0.00225750900482489,-0.0347058460402081,
-0.011101191635245));
#40674=CARTESIAN_POINT('Ctrl Pts',(-0.00224211888896316,-0.0347035973048026,
-0.0110694412202372));
#40675=CARTESIAN_POINT('Ctrl Pts',(-0.00220877457923461,-0.0346989736008557,
-0.0110042059535001));
#40676=CARTESIAN_POINT('Ctrl Pts',(-0.0021907187591027,-0.0346966027780981,
-0.0109707830927261));
#40677=CARTESIAN_POINT('Ctrl Pts',(-0.00213896637873289,-0.0346901468490987,
-0.0108799955127675));
#40678=CARTESIAN_POINT('Ctrl Pts',(-0.00210373030650426,-0.0346861151041094,
-0.010823542523949));
#40679=CARTESIAN_POINT('Ctrl Pts',(-0.00201504598976053,-0.0346767004594844,
-0.0106933304108255));
#40680=CARTESIAN_POINT('Ctrl Pts',(-0.00195973785539656,-0.0346713753060738,
-0.0106209535195878));
#40681=CARTESIAN_POINT('Ctrl Pts',(-0.00179391365990515,-0.0346565070988832,
-0.0104268978815339));
#40682=CARTESIAN_POINT('Ctrl Pts',(-0.00167519341524708,-0.0346470665395916,
-0.0103128757264084));
#40683=CARTESIAN_POINT('Ctrl Pts',(-0.00152315075834697,-0.0346351516612502,
-0.0101932111141045));
#40684=CARTESIAN_POINT('Ctrl Pts',(-0.00149981465869832,-0.034633326671725,
-0.0101754998091879));
#40685=CARTESIAN_POINT('Ctrl Pts',(-0.00146005539847901,-0.034630213585713,
-0.0101464107249192));
#40686=CARTESIAN_POINT('Ctrl Pts',(-0.00144379775285785,-0.0346289393583023,
-0.0101348126469914));
#40687=CARTESIAN_POINT('Ctrl Pts',(-0.00140715559342006,-0.0346260624641363,
-0.0101093293173079));
#40688=CARTESIAN_POINT('Ctrl Pts',(-0.00138670289505513,-0.0346244540307896,
-0.0100955496669878));
#40689=CARTESIAN_POINT('Ctrl Pts',(-0.00131767199853158,-0.0346190252680089,
-0.0100505116017802));
#40690=CARTESIAN_POINT('Ctrl Pts',(-0.00126821736329774,-0.0346151362338775,
-0.0100206362456736));
#40691=CARTESIAN_POINT('Ctrl Pts',(-0.00113005790033621,-0.0346043556512447,
-0.00994357699891012));
#40692=CARTESIAN_POINT('Ctrl Pts',(-0.00103947295709561,-0.0345973817149763,
-0.00989998351372832));
#40693=CARTESIAN_POINT('Ctrl Pts',(-0.000817317040240532,-0.0345807880205129,
-0.00980910915411257));
#40694=CARTESIAN_POINT('Ctrl Pts',(-0.000683906107050634,-0.0345712359493515,
-0.00976716765936511));
#40695=CARTESIAN_POINT('Ctrl Pts',(-0.000499157737457075,-0.0345587217490452,
-0.00972568710585009));
#40696=CARTESIAN_POINT('Ctrl Pts',(-0.000450322081987992,-0.0345554768339693,
-0.00971624288290118));
#40697=CARTESIAN_POINT('Ctrl Pts',(-0.000366359927380762,-0.0345500014398331,
-0.00970259050555726));
#40698=CARTESIAN_POINT('Ctrl Pts',(-0.000331367910254513,-0.0345477498223317,
-0.00969765961177541));
#40699=CARTESIAN_POINT('Ctrl Pts',(-0.00025836570147237,-0.0345431109971148,
-0.00968894652041296));
#40700=CARTESIAN_POINT('Ctrl Pts',(-0.000220349580041532,-0.0345407281429581,
-0.00968529021697187));
#40701=CARTESIAN_POINT('Ctrl Pts',(-0.000115083207838991,-0.0345342096616183,
-0.00967759527502233));
#40702=CARTESIAN_POINT('Ctrl Pts',(-4.77289176190029E-5,-0.034530129033425,
-0.00967540127058989));
#40703=CARTESIAN_POINT('Ctrl Pts',(0.000112395044014337,-0.0345205656371134,
-0.00967665899731326));
#40704=CARTESIAN_POINT('Ctrl Pts',(0.000205045019048902,-0.0345151433717406,
-0.0096825497271631));
#40705=CARTESIAN_POINT('Ctrl Pts',(0.000456794418630767,-0.0345003804972055,
-0.00971268695829775));
#40706=CARTESIAN_POINT('Ctrl Pts',(0.000614197895265314,-0.0344911282724244,
-0.00974715027266843));
#40707=CARTESIAN_POINT('Ctrl Pts',(0.000795455547349672,-0.0344794091892002,
-0.0098055931852241));
#40708=CARTESIAN_POINT('Ctrl Pts',(0.000823562568213125,-0.0344775597722573,
-0.00981521206143733));
#40709=CARTESIAN_POINT('Ctrl Pts',(0.000870229185463951,-0.0344744247707291,
-0.00983211729452332));
#40710=CARTESIAN_POINT('Ctrl Pts',(0.000888884696183502,-0.0344731538804419,
-0.00983912882522668));
#40711=CARTESIAN_POINT('Ctrl Pts',(0.000929847402013366,-0.0344703214682339,
-0.00985508589381992));
#40712=CARTESIAN_POINT('Ctrl Pts',(0.000952111331147731,-0.0344687549775865,
-0.00986413068409234));
#40713=CARTESIAN_POINT('Ctrl Pts',(0.00102435125151682,-0.0344635913345055,
-0.00989469892168406));
#40714=CARTESIAN_POINT('Ctrl Pts',(0.0010737529249031,-0.034459932618979,
-0.0099175321172254));
#40715=CARTESIAN_POINT('Ctrl Pts',(0.00120309491152283,-0.0344500783895446,
-0.00998251682775234));
#40716=CARTESIAN_POINT('Ctrl Pts',(0.00128156241638059,-0.0344438125132599,
-0.0100274215797191));
#40717=CARTESIAN_POINT('Ctrl Pts',(0.00148927752055119,-0.0344266722724442,
-0.0101617266769406));
#40718=CARTESIAN_POINT('Ctrl Pts',(0.00161282305172891,-0.034415869697555,
-0.0102592239452315));
#40719=CARTESIAN_POINT('Ctrl Pts',(0.00176215409281682,-0.0344022211451491,
-0.0104018029790606));
#40720=CARTESIAN_POINT('Ctrl Pts',(0.0017968745929216,-0.034398996343267,
-0.0104369789987399));
#40721=CARTESIAN_POINT('Ctrl Pts',(0.00185438199177565,-0.0343935609645254,
-0.01049880417321));
#40722=CARTESIAN_POINT('Ctrl Pts',(0.00187769182175053,-0.0343913291775538,
-0.0105249444700266));
#40723=CARTESIAN_POINT('Ctrl Pts',(0.00192494248141358,-0.0343867401775118,
-0.0105802286361311));
#40724=CARTESIAN_POINT('Ctrl Pts',(0.0019487886479754,-0.0343843870709691,
-0.0106094419030752));
#40725=CARTESIAN_POINT('Ctrl Pts',(0.00201246984772701,-0.0343779877183206,
-0.0106911622899306));
#40726=CARTESIAN_POINT('Ctrl Pts',(0.00205090501795098,-0.0343739940692101,
-0.0107447237002124));
#40727=CARTESIAN_POINT('Ctrl Pts',(0.0021366190938103,-0.0343646899409113,
-0.0108747285746264));
#40728=CARTESIAN_POINT('Ctrl Pts',(0.00218198220270771,-0.0343594357387127,
-0.0109523249243086));
#40729=CARTESIAN_POINT('Ctrl Pts',(0.00229942111359487,-0.0343444900436488,
-0.0111806061415237));
#40730=CARTESIAN_POINT('Ctrl Pts',(0.00236070736120421,-0.0343349134514614,
-0.0113362691455636));
#40731=CARTESIAN_POINT('Ctrl Pts',(0.00241391784569683,-0.0343228479597993,
-0.011524819440807));
#40732=CARTESIAN_POINT('Ctrl Pts',(0.00242132170961338,-0.0343210374697997,
-0.0115529203501193));
#40733=CARTESIAN_POINT('Ctrl Pts',(0.00243295361025697,-0.0343179471798899,
-0.0116004139777165));
#40734=CARTESIAN_POINT('Ctrl Pts',(0.00243744344825402,-0.034316681104037,
-0.0116197390274582));
#40735=CARTESIAN_POINT('Ctrl Pts',(0.0024469583218066,-0.0343138240267315,
-0.0116630237408342));
#40736=CARTESIAN_POINT('Ctrl Pts',(0.00245186197514166,-0.0343122273176846,
-0.0116870057467782));
#40737=CARTESIAN_POINT('Ctrl Pts',(0.00246160256896688,-0.0343087760115555,
-0.0117384837852018));
#40738=CARTESIAN_POINT('Ctrl Pts',(0.00246633264409253,-0.0343069169375645,
-0.0117659966725079));
#40739=CARTESIAN_POINT('Ctrl Pts',(0.00249006680650221,-0.034296491498923,
-0.011919389326348));
#40740=CARTESIAN_POINT('Ctrl Pts',(0.00249989323900895,-0.0342876380916422,
-0.0120464827820831));
#40741=CARTESIAN_POINT('Ctrl Pts',(0.00249999913488366,-0.0342788233790734,
-0.0121737734834593));
#40742=CARTESIAN_POINT('Ctrl Pts',(0.00249999913488366,-0.0342788233790735,
-0.0121737734834589));
#40743=CARTESIAN_POINT('Ctrl Pts',(0.00249999971163259,-0.0342787753708198,
-0.0121744667566923));
#40744=CARTESIAN_POINT('Ctrl Pts',(0.00249999999999997,-0.0342787273641556,
-0.0121751600244162));
#40745=CARTESIAN_POINT('Ctrl Pts',(0.0025,-0.0342786793591244,-0.0121758532864529));
#40746=CARTESIAN_POINT('Ctrl Pts',(0.0025,-0.0341527041915604,-0.0121758532865581));
#40747=CARTESIAN_POINT('Ctrl Pts',(0.0025,-0.0341588066255373,-0.0120871360834245));
#40748=CARTESIAN_POINT('Ctrl Pts',(0.00249527753979069,-0.0341649953633893,
-0.0119984444073263));
#40749=CARTESIAN_POINT('Ctrl Pts',(0.00247527802227061,-0.0341780560342344,
-0.0118113307178051));
#40750=CARTESIAN_POINT('Ctrl Pts',(0.0024588306282862,-0.034184905362994,
-0.0117132164488123));
#40751=CARTESIAN_POINT('Ctrl Pts',(0.00242104579703883,-0.034196288560602,
-0.0115486714482207));
#40752=CARTESIAN_POINT('Ctrl Pts',(0.002402695164542,-0.0342008942560627,
-0.0114816794736156));
#40753=CARTESIAN_POINT('Ctrl Pts',(0.00237028452718894,-0.0342078267516067,
-0.0113801585393498));
#40754=CARTESIAN_POINT('Ctrl Pts',(0.00235820408642621,-0.0342102163424318,
-0.0113450388630887));
#40755=CARTESIAN_POINT('Ctrl Pts',(0.00233392831921142,-0.0342146782956228,
-0.0112792676887648));
#40756=CARTESIAN_POINT('Ctrl Pts',(0.0023219002592204,-0.0342167557500717,
-0.0112485634233305));
#40757=CARTESIAN_POINT('Ctrl Pts',(0.00229279761930796,-0.0342214953478311,
-0.0111783928168259));
#40758=CARTESIAN_POINT('Ctrl Pts',(0.00227530506476294,-0.0342241424844795,
-0.0111391105392396));
#40759=CARTESIAN_POINT('Ctrl Pts',(0.00220319579794283,-0.0342343399942572,
-0.0109878058473953));
#40760=CARTESIAN_POINT('Ctrl Pts',(0.00214124627572804,-0.0342416334892694,
-0.0108794746021455));
#40761=CARTESIAN_POINT('Ctrl Pts',(0.00197772515517029,-0.0342585269327383,
-0.0106374644220687));
#40762=CARTESIAN_POINT('Ctrl Pts',(0.00187028961638902,-0.0342680078613533,
-0.0105085073887182));
#40763=CARTESIAN_POINT('Ctrl Pts',(0.00172324388897944,-0.0342804657353731,
-0.0103642464392609));
#40764=CARTESIAN_POINT('Ctrl Pts',(0.00169507978659403,-0.0342828329444561,
-0.0103378671573889));
#40765=CARTESIAN_POINT('Ctrl Pts',(0.0016508484689062,-0.0342865435359199,
-0.0102983203408101));
#40766=CARTESIAN_POINT('Ctrl Pts',(0.00163520732566602,-0.0342878544559937,
-0.0102846823249714));
#40767=CARTESIAN_POINT('Ctrl Pts',(0.00160554463223583,-0.0342903419211229,
-0.0102594615979602));
#40768=CARTESIAN_POINT('Ctrl Pts',(0.00159156337863107,-0.0342915146022978,
-0.0102478344500988));
#40769=CARTESIAN_POINT('Ctrl Pts',(0.00155272924514236,-0.0342947695793796,
-0.0102162492836129));
#40770=CARTESIAN_POINT('Ctrl Pts',(0.00152762036526226,-0.0342968716373137,
-0.0101966130894075));
#40771=CARTESIAN_POINT('Ctrl Pts',(0.0013900000871955,-0.0343083502253584,
-0.0100931670484586));
#40772=CARTESIAN_POINT('Ctrl Pts',(0.00127096671351649,-0.0343181124927171,
-0.0100184657936914));
#40773=CARTESIAN_POINT('Ctrl Pts',(0.00105454468871803,-0.0343349655484827,
-0.00990680122130327));
#40774=CARTESIAN_POINT('Ctrl Pts',(0.000959931804580723,-0.0343420692047618,
-0.0098651833277424));
#40775=CARTESIAN_POINT('Ctrl Pts',(0.000795326128183773,-0.0343538827462664,
-0.00980463899732866));
#40776=CARTESIAN_POINT('Ctrl Pts',(0.000726592220849624,-0.0343586643515419,
-0.0097826825447444));
#40777=CARTESIAN_POINT('Ctrl Pts',(0.000619092573203952,-0.0343659122134982,
-0.00975340247814949));
#40778=CARTESIAN_POINT('Ctrl Pts',(0.000580946012781767,-0.0343684407216593,
-0.00974397221660094));
#40779=CARTESIAN_POINT('Ctrl Pts',(0.000507803718102459,-0.0343732109216152,
-0.00972771003510177));
#40780=CARTESIAN_POINT('Ctrl Pts',(0.000472853504121802,-0.0343754568773819,
-0.00972071993818531));
#40781=CARTESIAN_POINT('Ctrl Pts',(0.00038938266601959,-0.0343807484171251,
-0.00970587434504571));
#40782=CARTESIAN_POINT('Ctrl Pts',(0.000340755663290763,-0.0343837732703598,
-0.00969869748261892));
#40783=CARTESIAN_POINT('Ctrl Pts',(0.000139091650495084,-0.0343961245379447,
-0.00967498522396319));
#40784=CARTESIAN_POINT('Ctrl Pts',(-1.50987334682496E-5,-0.0344050872759136,
-0.00967116483158575));
#40785=CARTESIAN_POINT('Ctrl Pts',(-0.000255412828585984,-0.0344191739210142,
-0.00968741544892404));
#40786=CARTESIAN_POINT('Ctrl Pts',(-0.00034178566742747,-0.0344242673917242,
-0.00969780170210138));
#40787=CARTESIAN_POINT('Ctrl Pts',(-0.000479858556137154,-0.0344326814562363,
-0.00972176149651209));
#40788=CARTESIAN_POINT('Ctrl Pts',(-0.000531972596123756,-0.0344359214382035,
-0.00973252868328095));
#40789=CARTESIAN_POINT('Ctrl Pts',(-0.000607322494260492,-0.0344407505742914,
-0.00975062142143391));
#40790=CARTESIAN_POINT('Ctrl Pts',(-0.00063086034652542,-0.0344422799766202,
-0.00975663743600475));
#40791=CARTESIAN_POINT('Ctrl Pts',(-0.00067408836425521,-0.0344451336154259,
-0.00976835977515811));
#40792=CARTESIAN_POINT('Ctrl Pts',(-0.000693802337755741,-0.0344464529108768,
-0.00977396687385435));
#40793=CARTESIAN_POINT('Ctrl Pts',(-0.000743847697447611,-0.0344498460801814,
-0.00978886838748338));
#40794=CARTESIAN_POINT('Ctrl Pts',(-0.000774074200212703,-0.0344519364745488,
-0.00979849861727811));
#40795=CARTESIAN_POINT('Ctrl Pts',(-0.000938846434620175,-0.0344635285834141,
-0.00985447076540195));
#40796=CARTESIAN_POINT('Ctrl Pts',(-0.00106942247211225,-0.0344734257907555,
-0.00991165807024596));
#40797=CARTESIAN_POINT('Ctrl Pts',(-0.00128262330724824,-0.0344901991988712,
-0.0100276076658194));
#40798=CARTESIAN_POINT('Ctrl Pts',(-0.00136786615463089,-0.0344970962365445,
-0.0100808528759677));
#40799=CARTESIAN_POINT('Ctrl Pts',(-0.00150714199903529,-0.0345085989724635,
-0.0101799831754404));
#40800=CARTESIAN_POINT('Ctrl Pts',(-0.00156285087249957,-0.0345132718793386,
-0.0102232977412049));
#40801=CARTESIAN_POINT('Ctrl Pts',(-0.00164617099831743,-0.0345203744222644,
-0.0102939345548012));
#40802=CARTESIAN_POINT('Ctrl Pts',(-0.00167510067844966,-0.0345228636463663,
-0.0103196380375233));
#40803=CARTESIAN_POINT('Ctrl Pts',(-0.00172916345075504,-0.0345275643055618,
-0.010369965562069));
#40804=CARTESIAN_POINT('Ctrl Pts',(-0.00175439601091676,-0.0345297798551923,
-0.0103944685599831));
#40805=CARTESIAN_POINT('Ctrl Pts',(-0.0018131129180065,-0.034534994059562,
-0.0104539459477249));
#40806=CARTESIAN_POINT('Ctrl Pts',(-0.00184611539207541,-0.0345379722942296,
-0.0104893771510893));
#40807=CARTESIAN_POINT('Ctrl Pts',(-0.00200734640564339,-0.034552819072591,
-0.0106728822769819));
#40808=CARTESIAN_POINT('Ctrl Pts',(-0.00211888257719614,-0.034564020584709,
-0.0108346963237527));
#40809=CARTESIAN_POINT('Ctrl Pts',(-0.00224218962433326,-0.0345794601199705,
-0.0110680544964574));
#40810=CARTESIAN_POINT('Ctrl Pts',(-0.00227151524080403,-0.0345834730057849,
-0.0111295024965632));
#40811=CARTESIAN_POINT('Ctrl Pts',(-0.00231633471788838,-0.0345903399083541,
-0.0112342085440858));
#40812=CARTESIAN_POINT('Ctrl Pts',(-0.0023332099359214,-0.0345931434377555,
-0.0112768359419936));
#40813=CARTESIAN_POINT('Ctrl Pts',(-0.00235669728837949,-0.0345974275935937,
-0.0113412898294623));
#40814=CARTESIAN_POINT('Ctrl Pts',(-0.00236419893875982,-0.0345988636594737,
-0.011362784063289));
#40815=CARTESIAN_POINT('Ctrl Pts',(-0.00237775615393995,-0.034601596563785,
-0.0114034039150018));
#40816=CARTESIAN_POINT('Ctrl Pts',(-0.00238387686492832,-0.0346028899322269,
-0.0114225051975321));
#40817=CARTESIAN_POINT('Ctrl Pts',(-0.00239926615506288,-0.0346063003020619,
-0.0114725978206038));
#40818=CARTESIAN_POINT('Ctrl Pts',(-0.00240816401635497,-0.034608435783106,
-0.0115036984121756));
#40819=CARTESIAN_POINT('Ctrl Pts',(-0.00245776525168612,-0.0346213505499705,
-0.0116907176672835));
#40820=CARTESIAN_POINT('Ctrl Pts',(-0.00248391695972193,-0.0346326314314633,
-0.0118500947594906));
#40821=CARTESIAN_POINT('Ctrl Pts',(-0.00250043972836219,-0.0346499134687464,
-0.0120999208994485));
#40822=CARTESIAN_POINT('Ctrl Pts',(-0.0025015570929233,-0.034656018967385,
-0.012189227968466));
#40823=CARTESIAN_POINT('Ctrl Pts',(-0.00249520360204096,-0.0346664103715346,
-0.0123439756892704));
#40824=CARTESIAN_POINT('Ctrl Pts',(-0.00248993102487983,-0.0346707468517693,
-0.0124094146122461));
#40825=CARTESIAN_POINT('Ctrl Pts',(-0.00247759270724932,-0.0346774501245827,
-0.0125119340443495));
#40826=CARTESIAN_POINT('Ctrl Pts',(-0.00247225347343839,-0.0346798672544537,
-0.0125491881345538));
#40827=CARTESIAN_POINT('Ctrl Pts',(-0.00246033089218614,-0.0346844824373551,
-0.0126208206288806));
#40828=CARTESIAN_POINT('Ctrl Pts',(-0.00245386274308029,-0.0346866834371846,
-0.0126552089642862));
#40829=CARTESIAN_POINT('Ctrl Pts',(-0.00243652122789473,-0.0346919419128282,
-0.0127378203036215));
#40830=CARTESIAN_POINT('Ctrl Pts',(-0.00242493529230502,-0.0346949767860079,
-0.0127858794660014));
#40831=CARTESIAN_POINT('Ctrl Pts',(-0.00237079009253734,-0.034707458746439,
-0.0129844380386911));
#40832=CARTESIAN_POINT('Ctrl Pts',(-0.00231558321647399,-0.0347165164253347,
-0.0131311200080114));
#40833=CARTESIAN_POINT('Ctrl Pts',(-0.00220725574056772,-0.0347308826707438,
-0.0133532466730315));
#40834=CARTESIAN_POINT('Ctrl Pts',(-0.00216307428721633,-0.0347361646808396,
-0.0134325716319483));
#40835=CARTESIAN_POINT('Ctrl Pts',(-0.00208559301979993,-0.034744849175532,
-0.0135554459739408));
#40836=CARTESIAN_POINT('Ctrl Pts',(-0.00205500448363599,-0.0347481590617163,
-0.0136006093793495));
#40837=CARTESIAN_POINT('Ctrl Pts',(-0.00200884604631038,-0.0347530455716281,
-0.0136641795636465));
#40838=CARTESIAN_POINT('Ctrl Pts',(-0.00199444686028728,-0.0347545560259131,
-0.0136834205863111));
#40839=CARTESIAN_POINT('Ctrl Pts',(-0.00196762282415661,-0.0347573509393794,
-0.013718207443292));
#40840=CARTESIAN_POINT('Ctrl Pts',(-0.00195528590681365,-0.0347586298962244,
-0.0137338176126994));
#40841=CARTESIAN_POINT('Ctrl Pts',(-0.00192413681585118,-0.0347618413164208,
-0.0137722785161897));
#40842=CARTESIAN_POINT('Ctrl Pts',(-0.00190510312411324,-0.0347637876592029,
-0.0137949449783718));
#40843=CARTESIAN_POINT('Ctrl Pts',(-0.00177957163424077,-0.0347764947088792,
-0.0139391568136953));
#40844=CARTESIAN_POINT('Ctrl Pts',(-0.001661909235318,-0.0347877922504112,
-0.0140504643252598));
#40845=CARTESIAN_POINT('Ctrl Pts',(-0.00146138727552628,-0.0348053310502105,
-0.0142063421343996));
#40846=CARTESIAN_POINT('Ctrl Pts',(-0.0013853439671957,-0.0348116592925567,
-0.0142589668650018));
#40847=CARTESIAN_POINT('Ctrl Pts',(-0.00124927825710126,-0.034822375789468,
-0.0143423752518866));
#40848=CARTESIAN_POINT('Ctrl Pts',(-0.00119060441940622,-0.0348268186772828,
-0.014375165912033));
#40849=CARTESIAN_POINT('Ctrl Pts',(-0.00109667301561655,-0.0348336589888785,
-0.0144227982865496));
#40850=CARTESIAN_POINT('Ctrl Pts',(-0.00106227844854788,-0.0348361091690161,
-0.0144392618418728));
#40851=CARTESIAN_POINT('Ctrl Pts',(-0.000995346579244765,-0.0348407773540105,
-0.014469437960957));
#40852=CARTESIAN_POINT('Ctrl Pts',(-0.000962869248225981,-0.0348429985456148,
-0.014483260593093));
#40853=CARTESIAN_POINT('Ctrl Pts',(-0.000883991768261539,-0.0348482948092699,
-0.0145148759477198));
#40854=CARTESIAN_POINT('Ctrl Pts',(-0.000837331887679209,-0.0348513474180882,
-0.0145319823697533));
#40855=CARTESIAN_POINT('Ctrl Pts',(-0.000658411478654128,-0.0348627929143484,
-0.0145915907667689));
#40856=CARTESIAN_POINT('Ctrl Pts',(-0.000523198611056358,-0.0348708971700031,
-0.0146244367467287));
#40857=CARTESIAN_POINT('Ctrl Pts',(-0.000286185470567523,-0.0348848647081733,
-0.0146614705853953));
#40858=CARTESIAN_POINT('Ctrl Pts',(-0.000185575366755641,-0.0348907277122509,
-0.0146709996317674));
#40859=CARTESIAN_POINT('Ctrl Pts',(-2.67850317323729E-5,-0.0349002124437143,
-0.0146763806565578));
#40860=CARTESIAN_POINT('Ctrl Pts',(3.11468071411945E-5,-0.0349037218853999,
-0.0146763299281411));
#40861=CARTESIAN_POINT('Ctrl Pts',(0.000113669102529428,-0.0349088548135483,
-0.0146733896095488));
#40862=CARTESIAN_POINT('Ctrl Pts',(0.00013830275365594,-0.0349104041086912,
-0.014672146656456));
#40863=CARTESIAN_POINT('Ctrl Pts',(0.000182810386925665,-0.0349132406345279,
-0.0146692401322728));
#40864=CARTESIAN_POINT('Ctrl Pts',(0.000202689664399399,-0.0349145215382621,
-0.0146677028817972));
#40865=CARTESIAN_POINT('Ctrl Pts',(0.000251617838013116,-0.0349177074934655,
-0.0146633299731633));
#40866=CARTESIAN_POINT('Ctrl Pts',(0.000280638455603433,-0.0349196255971715,
-0.014660223163764));
#40867=CARTESIAN_POINT('Ctrl Pts',(0.000473358686122774,-0.034932524723535,
-0.0146361718211618));
#40868=CARTESIAN_POINT('Ctrl Pts',(0.000634684462408655,-0.0349440698286065,
-0.0145995706082129));
#40869=CARTESIAN_POINT('Ctrl Pts',(0.000877230163152631,-0.0349617170482116,
-0.014518648403471));
#40870=CARTESIAN_POINT('Ctrl Pts',(0.000961623538307123,-0.0349679219629098,
-0.014485291346347));
#40871=CARTESIAN_POINT('Ctrl Pts',(0.00110430817594107,-0.0349784602585224,
-0.0144197127726436));
#40872=CARTESIAN_POINT('Ctrl Pts',(0.00116346999585728,-0.0349828457527284,
-0.0143896149681043));
#40873=CARTESIAN_POINT('Ctrl Pts',(0.00125445804353623,-0.0349896165763571,
-0.0143386693166316));
#40874=CARTESIAN_POINT('Ctrl Pts',(0.00128712287594484,-0.0349920531056776,
-0.014319390810375));
#40875=CARTESIAN_POINT('Ctrl Pts',(0.00134926931571013,-0.0349967039092671,
-0.0142807794191611));
#40876=CARTESIAN_POINT('Ctrl Pts',(0.00137880529019818,-0.0349989211753236,
-0.0142615517013248));
#40877=CARTESIAN_POINT('Ctrl Pts',(0.00144908291609466,-0.0350042202873406,
-0.0142136558653951));
#40878=CARTESIAN_POINT('Ctrl Pts',(0.00148939418751574,-0.0350072793149464,
-0.0141843816280446));
#40879=CARTESIAN_POINT('Ctrl Pts',(0.00164112625355554,-0.0350189125261958,
-0.0140671111735574));
#40880=CARTESIAN_POINT('Ctrl Pts',(0.00174585202455605,-0.0350271814890667,
-0.0139708900980514));
#40881=CARTESIAN_POINT('Ctrl Pts',(0.00190927271030721,-0.0350412409457035,
-0.0137928319113384));
#40882=CARTESIAN_POINT('Ctrl Pts',(0.00197223586600247,-0.0350470293269974,
-0.013715407077957));
#40883=CARTESIAN_POINT('Ctrl Pts',(0.00206397662559593,-0.035056414587606,
-0.0135877001800061));
#40884=CARTESIAN_POINT('Ctrl Pts',(0.00209592289932448,-0.0350599010652843,
-0.0135398244610649));
#40885=CARTESIAN_POINT('Ctrl Pts',(0.0021391025049762,-0.0350650034463417,
-0.0134700106846962));
#40886=CARTESIAN_POINT('Ctrl Pts',(0.00215170936165408,-0.0350665457260261,
-0.0134489399342518));
#40887=CARTESIAN_POINT('Ctrl Pts',(0.00217395034764177,-0.0350693703485281,
-0.0134104927094573));
#40888=CARTESIAN_POINT('Ctrl Pts',(0.00218369114775571,-0.0350706464090404,
-0.0133931813009595));
#40889=CARTESIAN_POINT('Ctrl Pts',(0.00220715464695614,-0.035073816863557,
-0.0133502938921162));
#40890=CARTESIAN_POINT('Ctrl Pts',(0.00222063971208916,-0.0350757241727262,
-0.013324592364697));
#40891=CARTESIAN_POINT('Ctrl Pts',(0.00230837111307789,-0.035088696793558,
-0.0131500629978429));
#40892=CARTESIAN_POINT('Ctrl Pts',(0.00236804885050966,-0.0351003376094888,
-0.0129943889731383));
#40893=CARTESIAN_POINT('Ctrl Pts',(0.00243557924095236,-0.0351180438994538,
-0.0127469014541685));
#40894=CARTESIAN_POINT('Ctrl Pts',(0.00245460364213349,-0.0351242181989909,
-0.0126586218181295));
#40895=CARTESIAN_POINT('Ctrl Pts',(0.00247922918477262,-0.0351347128073175,
-0.0125041793623759));
#40896=CARTESIAN_POINT('Ctrl Pts',(0.00248704867823636,-0.0351390846953079,
-0.0124384661183763));
#40897=CARTESIAN_POINT('Ctrl Pts',(0.00249523125352792,-0.0351458381559335,
-0.0123347700737067));
#40898=CARTESIAN_POINT('Ctrl Pts',(0.00249735195341803,-0.0351482706356105,
-0.0122969607783721));
#40899=CARTESIAN_POINT('Ctrl Pts',(0.00249953761635375,-0.0351524419826498,
-0.0122313718280536));
#40900=CARTESIAN_POINT('Ctrl Pts',(0.00249999999999506,-0.0351541924015739,
-0.0122036137105421));
#40901=CARTESIAN_POINT('Ctrl Pts',(0.0025,-0.0351559292844039,-0.0121758532870029));
#40902=CARTESIAN_POINT('Origin',(0.,-0.0397787743898723,-0.0121758532865581));
#40903=CARTESIAN_POINT('',(0.0025,-0.0362767501454997,-0.0121758532853817));
#40904=CARTESIAN_POINT('',(0.0025,-0.0361517921417372,-0.0121758532874351));
#40905=CARTESIAN_POINT('',(0.0025,-0.0397787743898723,-0.0121758532865581));
#40906=CARTESIAN_POINT('Ctrl Pts',(0.0025,-0.0362767501454997,-0.0121758532842053));
#40907=CARTESIAN_POINT('Ctrl Pts',(0.00250000000003539,-0.0362742798368169,
-0.012213451230406));
#40908=CARTESIAN_POINT('Ctrl Pts',(0.00249915183964461,-0.036271833829592,
-0.012251047489016));
#40909=CARTESIAN_POINT('Ctrl Pts',(0.00249586502308434,-0.0362671423022065,
-0.0123238451097689));
#40910=CARTESIAN_POINT('Ctrl Pts',(0.00249352892036452,-0.0362648943823479,
-0.0123590403969366));
#40911=CARTESIAN_POINT('Ctrl Pts',(0.00248713228653339,-0.0362602718961515,
-0.0124320080354312));
#40912=CARTESIAN_POINT('Ctrl Pts',(0.00248295402812442,-0.0362579014839455,
-0.0124697610933965));
#40913=CARTESIAN_POINT('Ctrl Pts',(0.00246909473769026,-0.0362514458748145,
-0.0125733409410715));
#40914=CARTESIAN_POINT('Ctrl Pts',(0.00245764382194434,-0.0362474140866701,
-0.0126389009802414));
#40915=CARTESIAN_POINT('Ctrl Pts',(0.00242436584690413,-0.0362380003315025,
-0.0127928893667135));
#40916=CARTESIAN_POINT('Ctrl Pts',(0.00240029697529597,-0.0362326761439758,
-0.0128807355787434));
#40917=CARTESIAN_POINT('Ctrl Pts',(0.00231943916770289,-0.0362177967447705,
-0.0131230862230201));
#40918=CARTESIAN_POINT('Ctrl Pts',(0.00225212683118324,-0.0362083448600165,
-0.0132735600266043));
#40919=CARTESIAN_POINT('Ctrl Pts',(0.00215602120519229,-0.0361964175200519,
-0.0134417241289305));
#40920=CARTESIAN_POINT('Ctrl Pts',(0.00214105616598809,-0.0361945944312331,
-0.0134668741033465));
#40921=CARTESIAN_POINT('Ctrl Pts',(0.00211516712920496,-0.0361914863336613,
-0.0135086942177314));
#40922=CARTESIAN_POINT('Ctrl Pts',(0.00210447930295857,-0.0361902152349852,
-0.0135255064880057));
#40923=CARTESIAN_POINT('Ctrl Pts',(0.00208019706886413,-0.036187351384371,
-0.0135627133196155));
#40924=CARTESIAN_POINT('Ctrl Pts',(0.00206650264918606,-0.0361857530052879,
-0.0135830374564709));
#40925=CARTESIAN_POINT('Ctrl Pts',(0.00201994219183921,-0.0361803815135176,
-0.0136499930560305));
#40926=CARTESIAN_POINT('Ctrl Pts',(0.00198578075629083,-0.0361765410478188,
-0.0136956981243938));
#40927=CARTESIAN_POINT('Ctrl Pts',(0.0018886691428119,-0.0361659647451942,
-0.0138167565458728));
#40928=CARTESIAN_POINT('Ctrl Pts',(0.00182279533272519,-0.0361591488909438,
-0.0138896358640562));
#40929=CARTESIAN_POINT('Ctrl Pts',(0.00165028818866548,-0.0361424075153059,
-0.0140592603107328));
#40930=CARTESIAN_POINT('Ctrl Pts',(0.00153924892779323,-0.036132553152112,
-0.0141510484031478));
#40931=CARTESIAN_POINT('Ctrl Pts',(0.00137993077660253,-0.0361197512957352,
-0.0142611045970387));
#40932=CARTESIAN_POINT('Ctrl Pts',(0.0013381012702414,-0.0361164994641448,
-0.0142881902689378));
#40933=CARTESIAN_POINT('Ctrl Pts',(0.00126532526474961,-0.0361110212028333,
-0.0143322845357926));
#40934=CARTESIAN_POINT('Ctrl Pts',(0.00123477829368026,-0.036108773319183,
-0.0143499201035272));
#40935=CARTESIAN_POINT('Ctrl Pts',(0.00117058220422291,-0.0361041508053646,
-0.0143851924752899));
#40936=CARTESIAN_POINT('Ctrl Pts',(0.00113688360032603,-0.0361017803314408,
-0.0144027206525344));
#40937=CARTESIAN_POINT('Ctrl Pts',(0.00104309055690354,-0.0360953242551307,
-0.0144488223243292));
#40938=CARTESIAN_POINT('Ctrl Pts',(0.000982233098250018,-0.0360912920756931,
-0.0144757761897292));
#40939=CARTESIAN_POINT('Ctrl Pts',(0.000835734274614518,-0.0360818770585062,
-0.0145337833658971));
#40940=CARTESIAN_POINT('Ctrl Pts',(0.000749329330506343,-0.0360765520245548,
-0.014562648820967));
#40941=CARTESIAN_POINT('Ctrl Pts',(0.000502973206773787,-0.0360616738905954,
-0.014630248183925));
#40942=CARTESIAN_POINT('Ctrl Pts',(0.000340520377472886,-0.0360522239677828,
-0.0146580034234385));
#40943=CARTESIAN_POINT('Ctrl Pts',(0.000147346921735369,-0.0360402986902551,
-0.0146716789118213));
#40944=CARTESIAN_POINT('Ctrl Pts',(0.000118118522926962,-0.0360384753567975,
-0.0146732328151908));
#40945=CARTESIAN_POINT('Ctrl Pts',(6.89599105717247E-5,-0.0360353669758907,
-0.0146749814319072));
#40946=CARTESIAN_POINT('Ctrl Pts',(4.90429610993991E-5,-0.0360340958447883,
-0.0146754515968087));
#40947=CARTESIAN_POINT('Ctrl Pts',(4.61775067226181E-6,-0.0360312320843629,
-0.0146759691206749));
#40948=CARTESIAN_POINT('Ctrl Pts',(-1.98876176675432E-5,-0.0360296338314264,
-0.0146758942623929));
#40949=CARTESIAN_POINT('Ctrl Pts',(-0.000101411416379767,-0.0360242634596296,
-0.0146744466026542));
#40950=CARTESIAN_POINT('Ctrl Pts',(-0.000158380604390681,-0.0360204240261645,
-0.0146714829554495));
#40951=CARTESIAN_POINT('Ctrl Pts',(-0.000312940110943239,-0.0360098519690956,
-0.0146581292788499));
#40952=CARTESIAN_POINT('Ctrl Pts',(-0.000410101335124589,-0.036003039393073,
-0.0146439378515311));
#40953=CARTESIAN_POINT('Ctrl Pts',(-0.000647037732160346,-0.0359862969155427,
-0.0145949508310812));
#40954=CARTESIAN_POINT('Ctrl Pts',(-0.000785141392585863,-0.0359764382009579,
-0.0145537207444458));
#40955=CARTESIAN_POINT('Ctrl Pts',(-0.000965278266506552,-0.035963632264159,
-0.0144825218564019));
#40956=CARTESIAN_POINT('Ctrl Pts',(-0.00101105504778219,-0.0359603804027877,
-0.0144628273296399));
#40957=CARTESIAN_POINT('Ctrl Pts',(-0.0010881806630824,-0.0359549020845861,
-0.0144268767500522));
#40958=CARTESIAN_POINT('Ctrl Pts',(-0.00111982828435481,-0.0359526541738741,
-0.014411301474992));
#40959=CARTESIAN_POINT('Ctrl Pts',(-0.00118485030569796,-0.0359480315930496,
-0.0143775735571073));
#40960=CARTESIAN_POINT('Ctrl Pts',(-0.00121816195650317,-0.0359456610794981,
-0.014359319357517));
#40961=CARTESIAN_POINT('Ctrl Pts',(-0.00130864788004727,-0.0359392048471741,
-0.0143070189622278));
#40962=CARTESIAN_POINT('Ctrl Pts',(-0.00136490058654355,-0.035935172554497,
-0.0142714376593029));
#40963=CARTESIAN_POINT('Ctrl Pts',(-0.00149460010370507,-0.0359257572057223,
-0.0141819582813932));
#40964=CARTESIAN_POINT('Ctrl Pts',(-0.00156665336028348,-0.0359204319588141,
-0.0141262084595669));
#40965=CARTESIAN_POINT('Ctrl Pts',(-0.00175986139117141,-0.0359055540571048,
-0.0139590867851481));
#40966=CARTESIAN_POINT('Ctrl Pts',(-0.00187328553768628,-0.035896104546535,
-0.0138395305970088));
#40967=CARTESIAN_POINT('Ctrl Pts',(-0.00199209951218874,-0.0358841796984165,
-0.013686613446243));
#40968=CARTESIAN_POINT('Ctrl Pts',(-0.00200964984411278,-0.0358823563041242,
-0.0136631878350116));
#40969=CARTESIAN_POINT('Ctrl Pts',(-0.00203844820398308,-0.0358792478622715,
-0.0136233082515866));
#40970=CARTESIAN_POINT('Ctrl Pts',(-0.00204991778651283,-0.0358779767328549,
-0.0136070185436724));
#40971=CARTESIAN_POINT('Ctrl Pts',(-0.00207505884702381,-0.0358751130527538,
-0.013570389492645));
#40972=CARTESIAN_POINT('Ctrl Pts',(-0.00208862718096007,-0.0358735148801182,
-0.0135499845896847));
#40973=CARTESIAN_POINT('Ctrl Pts',(-0.00213276806177369,-0.0358681450113287,
-0.0134814384070232));
#40974=CARTESIAN_POINT('Ctrl Pts',(-0.00216199154365445,-0.0358643060142999,
-0.0134324533434562));
#40975=CARTESIAN_POINT('Ctrl Pts',(-0.00223685756843397,-0.0358537357269175,
-0.0132966075180066));
#40976=CARTESIAN_POINT('Ctrl Pts',(-0.00227910406805199,-0.0358469245073912,
-0.0132079896077078));
#40977=CARTESIAN_POINT('Ctrl Pts',(-0.00237020292568441,-0.0358301812583886,
-0.0129838367762815));
#40978=CARTESIAN_POINT('Ctrl Pts',(-0.00241277157008422,-0.0358203204328534,
-0.0128461088212256));
#40979=CARTESIAN_POINT('Ctrl Pts',(-0.00245381173849764,-0.0358075125512418,
-0.0126567794304275));
#40980=CARTESIAN_POINT('Ctrl Pts',(-0.00246290864222748,-0.03580426070058,
-0.0126077833554056));
#40981=CARTESIAN_POINT('Ctrl Pts',(-0.00247593425567407,-0.0357987824382894,
-0.012523694199589));
#40982=CARTESIAN_POINT('Ctrl Pts',(-0.00248059492029272,-0.0357965345717058,
-0.0124887315081));
#40983=CARTESIAN_POINT('Ctrl Pts',(-0.00248873492754618,-0.0357919121216361,
-0.0124159381709361));
#40984=CARTESIAN_POINT('Ctrl Pts',(-0.00249209500409768,-0.035789541693736,
-0.0123781031826441));
#40985=CARTESIAN_POINT('Ctrl Pts',(-0.00249896535964855,-0.0357830858424721,
-0.0122738221572908));
#40986=CARTESIAN_POINT('Ctrl Pts',(-0.00250068764272604,-0.0357790538369016,
-0.012207288060753));
#40987=CARTESIAN_POINT('Ctrl Pts',(-0.00249847599515115,-0.0357696393713747,
-0.012049747895681));
#40988=CARTESIAN_POINT('Ctrl Pts',(-0.0024922287946029,-0.0357643147058106,
-0.0119588697962729));
#40989=CARTESIAN_POINT('Ctrl Pts',(-0.00246082382976147,-0.0357494359607489,
-0.0117053343378756));
#40990=CARTESIAN_POINT('Ctrl Pts',(-0.0024245586070309,-0.0357399851284444,
-0.0115445493743673));
#40991=CARTESIAN_POINT('Ctrl Pts',(-0.00236356409660929,-0.0357280588907157,
-0.0113607328619742));
#40992=CARTESIAN_POINT('Ctrl Pts',(-0.00235386028875028,-0.0357262356822809,
-0.0113331207579026));
#40993=CARTESIAN_POINT('Ctrl Pts',(-0.00233673996969483,-0.035723127472226,
-0.0112870095198973));
#40994=CARTESIAN_POINT('Ctrl Pts',(-0.00232958311796028,-0.0357218563846345,
-0.0112684176731279));
#40995=CARTESIAN_POINT('Ctrl Pts',(-0.00231312842250273,-0.0357189927008714,
-0.0112271502869139));
#40996=CARTESIAN_POINT('Ctrl Pts',(-0.00230371869008368,-0.0357173944807205,
-0.0112045240076565));
#40997=CARTESIAN_POINT('Ctrl Pts',(-0.00227130619100571,-0.0357120241559889,
-0.0111297075121592));
#40998=CARTESIAN_POINT('Ctrl Pts',(-0.00224685145687106,-0.03570818473348,
-0.0110781692014115));
#40999=CARTESIAN_POINT('Ctrl Pts',(-0.00217559331369965,-0.0356976127653918,
-0.010940369967551));
#41000=CARTESIAN_POINT('Ctrl Pts',(-0.0021254391976599,-0.0356908002626232,
-0.0108559546446451));
#41001=CARTESIAN_POINT('Ctrl Pts',(-0.0019898306636158,-0.0356740567926241,
-0.0106555675341315));
#41002=CARTESIAN_POINT('Ctrl Pts',(-0.00189906250214117,-0.0356641970266547,
-0.0105435952334376));
#41003=CARTESIAN_POINT('Ctrl Pts',(-0.00176456351026726,-0.0356513900662507,
-0.0104041880502071));
#41004=CARTESIAN_POINT('Ctrl Pts',(-0.00172890604034565,-0.0356481381518676,
-0.0103693742372358));
#41005=CARTESIAN_POINT('Ctrl Pts',(-0.00166627049053323,-0.0356426598097454,
-0.0103117753893409));
#41006=CARTESIAN_POINT('Ctrl Pts',(-0.00163980793770195,-0.0356404119257114,
-0.0102884545785825));
#41007=CARTESIAN_POINT('Ctrl Pts',(-0.00158384268185474,-0.0356357894651906,
-0.0102411996644271));
#41008=CARTESIAN_POINT('Ctrl Pts',(-0.00155427004074099,-0.0356334190437703,
-0.010217362245588));
#41009=CARTESIAN_POINT('Ctrl Pts',(-0.00147143279599603,-0.0356269632742615,
-0.0101536487678609));
#41010=CARTESIAN_POINT('Ctrl Pts',(-0.00141710052301308,-0.0356229313404055,
-0.0101152095135281));
#41011=CARTESIAN_POINT('Ctrl Pts',(-0.00128495398481078,-0.0356135170682256,
-0.0100294195715061));
#41012=CARTESIAN_POINT('Ctrl Pts',(-0.00120595941157477,-0.0356081925194984,
-0.00998406231443595));
#41013=CARTESIAN_POINT('Ctrl Pts',(-0.000977800071622283,-0.0355933138902623,
-0.00986913509743623));
#41014=CARTESIAN_POINT('Ctrl Pts',(-0.000824012815343339,-0.0355838630581899,
-0.00980983728253009));
#41015=CARTESIAN_POINT('Ctrl Pts',(-0.000637330312100262,-0.035571936837129,
-0.00975827875267805));
#41016=CARTESIAN_POINT('Ctrl Pts',(-0.000608986284533946,-0.035570113618245,
-0.00975098378753445));
#41017=CARTESIAN_POINT('Ctrl Pts',(-0.000561142507623278,-0.0355670053188939,
-0.00973956182958314));
#41018=CARTESIAN_POINT('Ctrl Pts',(-0.000541710140536657,-0.0355657341502486,
-0.0097351675080811));
#41019=CARTESIAN_POINT('Ctrl Pts',(-0.000498257495023248,-0.0355628700836613,
-0.00972588590340469));
#41020=CARTESIAN_POINT('Ctrl Pts',(-0.000474215893425129,-0.0355612715571717,
-0.00972111910811612));
#41021=CARTESIAN_POINT('Ctrl Pts',(-0.000393985943292631,-0.0355558994479853,
-0.00970643424078383));
#41022=CARTESIAN_POINT('Ctrl Pts',(-0.000337531478998195,-0.035552058503816,
-0.00969808677768321));
#41023=CARTESIAN_POINT('Ctrl Pts',(-0.000183288186653136,-0.0355414802182338,
-0.0096806489841735));
#41024=CARTESIAN_POINT('Ctrl Pts',(-8.51688573928007E-5,-0.0355346628439944,
-0.00967537648262942));
#41025=CARTESIAN_POINT('Ctrl Pts',(0.000156730123925787,-0.0355179238096782,
-0.009676634668049));
#41026=CARTESIAN_POINT('Ctrl Pts',(0.000300141709513632,-0.035508073266911,
-0.00968977547925869));
#41027=CARTESIAN_POINT('Ctrl Pts',(0.000490679471344255,-0.0354952749840797,
-0.00972397327593038));
#41028=CARTESIAN_POINT('Ctrl Pts',(0.000539443418733203,-0.0354920231967573,
-0.00973423839298679));
#41029=CARTESIAN_POINT('Ctrl Pts',(0.000622150905097135,-0.0354865448540481,
-0.00975424800276134));
#41030=CARTESIAN_POINT('Ctrl Pts',(0.000656252858193686,-0.0354842968498632,
-0.0097632662339819));
#41031=CARTESIAN_POINT('Ctrl Pts',(0.000726660925783979,-0.0354796739271464,
-0.00978348905775959));
#41032=CARTESIAN_POINT('Ctrl Pts',(0.000762925550661222,-0.0354773031686589,
-0.00979480571308437));
#41033=CARTESIAN_POINT('Ctrl Pts',(0.000861976948827517,-0.0354708457606185,
-0.00982821102320259));
#41034=CARTESIAN_POINT('Ctrl Pts',(0.000924163142924798,-0.0354668125653466,
-0.009851987540393));
#41035=CARTESIAN_POINT('Ctrl Pts',(0.00106902259016853,-0.035457394463237,
-0.0099141098788852));
#41036=CARTESIAN_POINT('Ctrl Pts',(0.00115069444666908,-0.0354520674139331,
-0.00995454822799694));
#41037=CARTESIAN_POINT('Ctrl Pts',(0.00137306282325345,-0.0354371918028122,
-0.0100802127853202));
#41038=CARTESIAN_POINT('Ctrl Pts',(0.00150780583625054,-0.0354277460887824,
-0.0101749736609747));
#41039=CARTESIAN_POINT('Ctrl Pts',(0.00165443749127167,-0.0354158252131631,
-0.0103013683383368));
#41040=CARTESIAN_POINT('Ctrl Pts',(0.0016762756203987,-0.0354140013013983,
-0.010320871586817));
#41041=CARTESIAN_POINT('Ctrl Pts',(0.00171239035777612,-0.0354108923045119,
-0.0103542835675033));
#41042=CARTESIAN_POINT('Ctrl Pts',(0.00172685190792062,-0.0354096211519043,
-0.0103679872971774));
#41043=CARTESIAN_POINT('Ctrl Pts',(0.00175872769575892,-0.0354067579332773,
-0.0103989241994791));
#41044=CARTESIAN_POINT('Ctrl Pts',(0.00177605393037219,-0.0354051602564452,
-0.0104162418478012));
#41045=CARTESIAN_POINT('Ctrl Pts',(0.00183282929455883,-0.035399793802733,
-0.010474681950104));
#41046=CARTESIAN_POINT('Ctrl Pts',(0.00187112462385743,-0.0353959578255314,
-0.0105168961417131));
#41047=CARTESIAN_POINT('Ctrl Pts',(0.00197124035714185,-0.0353853998316306,
-0.0106351368726826));
#41048=CARTESIAN_POINT('Ctrl Pts',(0.00203008880682895,-0.0353785980558163,
-0.0107135489551092));
#41049=CARTESIAN_POINT('Ctrl Pts',(0.002163746215651,-0.0353618501330064,
-0.0109153145172044));
#41050=CARTESIAN_POINT('Ctrl Pts',(0.00223278743846951,-0.0353519752945608,
-0.0110420870544471));
#41051=CARTESIAN_POINT('Ctrl Pts',(0.00231049099123751,-0.0353391544457537,
-0.0112197605476901));
#41052=CARTESIAN_POINT('Ctrl Pts',(0.00232908545824077,-0.035335902625978,
-0.0112659942674584));
#41053=CARTESIAN_POINT('Ctrl Pts',(0.00235846134782538,-0.0353304245824456,
-0.0113458511149229));
#41054=CARTESIAN_POINT('Ctrl Pts',(0.00236993463776702,-0.0353281768989369,
-0.0113792018272071));
#41055=CARTESIAN_POINT('Ctrl Pts',(0.00239228894420847,-0.0353235549985508,
-0.0114489451401146));
#41056=CARTESIAN_POINT('Ctrl Pts',(0.00240305403993767,-0.0353211849330625,
-0.011485365512862));
#41057=CARTESIAN_POINT('Ctrl Pts',(0.00243037926343884,-0.0353147307057141,
-0.0115862096129212));
#41058=CARTESIAN_POINT('Ctrl Pts',(0.00244520534939592,-0.0353106999261971,
-0.0116510724868956));
#41059=CARTESIAN_POINT('Ctrl Pts',(0.00247414595144908,-0.0353012892458527,
-0.0118058820223453));
#41060=CARTESIAN_POINT('Ctrl Pts',(0.00248597059139312,-0.0352959670760043,
-0.0118961597482336));
#41061=CARTESIAN_POINT('Ctrl Pts',(0.00249761723666546,-0.0352869934099935,
-0.0120498004510097));
#41062=CARTESIAN_POINT('Ctrl Pts',(0.0025,-0.0352833345293618,-0.0121128350691632));
#41063=CARTESIAN_POINT('Ctrl Pts',(0.0025,-0.0352796511099541,-0.0121758532865581));
#41064=CARTESIAN_POINT('Ctrl Pts',(0.0025,-0.0351559292844039,-0.0121758532870029));
#41065=CARTESIAN_POINT('Ctrl Pts',(0.00250000000000132,-0.0351563949541079,
-0.0121684105349698));
#41066=CARTESIAN_POINT('Ctrl Pts',(0.00249996676327267,-0.0351568596530242,
-0.0121609676173145));
#41067=CARTESIAN_POINT('Ctrl Pts',(0.00249945563224408,-0.0351604252519763,
-0.0121037414352842));
#41068=CARTESIAN_POINT('Ctrl Pts',(0.00249752398131161,-0.0351634828049984,
-0.0120539802566494));
#41069=CARTESIAN_POINT('Ctrl Pts',(0.00248417584769355,-0.0351752826153707,
-0.0118599116843188));
#41070=CARTESIAN_POINT('Ctrl Pts',(0.00246172365287784,-0.0351837048321569,
-0.0117166472795673));
#41071=CARTESIAN_POINT('Ctrl Pts',(0.00240359142092288,-0.0351978012676244,
-0.011481397620577));
#41072=CARTESIAN_POINT('Ctrl Pts',(0.00237466026504458,-0.035203470028303,
-0.0113881305486763));
#41073=CARTESIAN_POINT('Ctrl Pts',(0.00232036759136451,-0.0352126903552338,
-0.0112435843160812));
#41074=CARTESIAN_POINT('Ctrl Pts',(0.00229857248667062,-0.0352161360438733,
-0.0111910717120396));
#41075=CARTESIAN_POINT('Ctrl Pts',(0.00226487208409575,-0.0352211894268369,
-0.0111171029889639));
#41076=CARTESIAN_POINT('Ctrl Pts',(0.00225441016863284,-0.0352227253709667,
-0.01109500527027));
#41077=CARTESIAN_POINT('Ctrl Pts',(0.00223485120237666,-0.0352255454814689,
-0.0110552124706219));
#41078=CARTESIAN_POINT('Ctrl Pts',(0.0022258641541744,-0.0352268235574635,
-0.0110374665313088));
#41079=CARTESIAN_POINT('Ctrl Pts',(0.0022031559284935,-0.0352300088783028,
-0.0109939236615293));
#41080=CARTESIAN_POINT('Ctrl Pts',(0.00218919286850779,-0.03523192932776,
-0.0109682572885822));
#41081=CARTESIAN_POINT('Ctrl Pts',(0.00209352430275947,-0.0352448140888636,
-0.0107995170592295));
#41082=CARTESIAN_POINT('Ctrl Pts',(0.00199830057539474,-0.0352563406702599,
-0.0106645841139374));
#41083=CARTESIAN_POINT('Ctrl Pts',(0.00183102350259616,-0.0352739873557177,
-0.0104712665222593));
#41084=CARTESIAN_POINT('Ctrl Pts',(0.00176783438139355,-0.0352802088729795,
-0.01040581741614));
#41085=CARTESIAN_POINT('Ctrl Pts',(0.00165251240364309,-0.0352907716238003,
-0.0102987223685377));
#41086=CARTESIAN_POINT('Ctrl Pts',(0.00160202124309784,-0.0352951653377304,
-0.0102554504786439));
#41087=CARTESIAN_POINT('Ctrl Pts',(0.00152008518961002,-0.0353019458751378,
-0.0101907132115773));
#41088=CARTESIAN_POINT('Ctrl Pts',(0.00148977592009498,-0.0353043841466608,
-0.0101678672158307));
#41089=CARTESIAN_POINT('Ctrl Pts',(0.00143034112872585,-0.0353090367980789,
-0.0101251543753234));
#41090=CARTESIAN_POINT('Ctrl Pts',(0.00140129271959162,-0.0353112542025186,
-0.0101051962220878));
#41091=CARTESIAN_POINT('Ctrl Pts',(0.00133021990096038,-0.0353165516001159,
-0.0100585454518144));
#41092=CARTESIAN_POINT('Ctrl Pts',(0.00128780065812075,-0.0353196088451457,
-0.0100324803810824));
#41093=CARTESIAN_POINT('Ctrl Pts',(0.00112127729252926,-0.0353312577349212,
-0.00993688767448848));
#41094=CARTESIAN_POINT('Ctrl Pts',(0.000992104147321659,-0.0353395429594198,
-0.0098767308884868));
#41095=CARTESIAN_POINT('Ctrl Pts',(0.000765359196507202,-0.0353535905513078,
-0.00979382437928423));
#41096=CARTESIAN_POINT('Ctrl Pts',(0.000670272116732628,-0.035359350249661,
-0.00976534094291586));
#41097=CARTESIAN_POINT('Ctrl Pts',(0.000517919142949801,-0.0353686952236813,
-0.00972941706779019));
#41098=CARTESIAN_POINT('Ctrl Pts',(0.000461655641987034,-0.0353721714424997,
-0.00971817887930309));
#41099=CARTESIAN_POINT('Ctrl Pts',(0.000380842526593096,-0.0353772623090306,
-0.00970490989068861));
#41100=CARTESIAN_POINT('Ctrl Pts',(0.000356568932833508,-0.0353788039382319,
-0.00970129054060954));
#41101=CARTESIAN_POINT('Ctrl Pts',(0.000312527065379535,-0.0353816299620092,
-0.00969538504345239));
#41102=CARTESIAN_POINT('Ctrl Pts',(0.000292778126937727,-0.0353829081395409,
-0.00969297657919998));
#41103=CARTESIAN_POINT('Ctrl Pts',(0.000244031635842235,-0.0353860887645381,
-0.00968762137815184));
#41104=CARTESIAN_POINT('Ctrl Pts',(0.000215008280882003,-0.0353880042806885,
-0.00968494567372648));
#41105=CARTESIAN_POINT('Ctrl Pts',(2.10568285708737E-5,-0.0354009219605038,
-0.00967047978151122));
#41106=CARTESIAN_POINT('Ctrl Pts',(-0.000144635598741956,-0.0354124912163048,
-0.00967457069291537));
#41107=CARTESIAN_POINT('Ctrl Pts',(-0.000398625926296231,-0.0354301576349027,
-0.00970617534028667));
#41108=CARTESIAN_POINT('Ctrl Pts',(-0.000487882207660514,-0.0354363590074527,
-0.00972224675691553));
#41109=CARTESIAN_POINT('Ctrl Pts',(-0.000640618188577008,-0.0354468925933814,
-0.00975841501196895));
#41110=CARTESIAN_POINT('Ctrl Pts',(-0.000704532122699878,-0.0354512768861299,
-0.00977626264724338));
#41111=CARTESIAN_POINT('Ctrl Pts',(-0.000803747658189741,-0.0354580459161638,
-0.00980827495116807));
#41112=CARTESIAN_POINT('Ctrl Pts',(-0.00083956193405003,-0.0354604818534231,
-0.00982073683892129));
#41113=CARTESIAN_POINT('Ctrl Pts',(-0.000908079630434014,-0.0354651314129944,
-0.00984633995201143));
#41114=CARTESIAN_POINT('Ctrl Pts',(-0.000940815643358329,-0.0354673480290801,
-0.0098593673462336));
#41115=CARTESIAN_POINT('Ctrl Pts',(-0.00101912801234922,-0.0354726454485083,
-0.00989246609554668));
#41116=CARTESIAN_POINT('Ctrl Pts',(-0.00106440209258983,-0.0354757034503298,
-0.0099132159646103));
#41117=CARTESIAN_POINT('Ctrl Pts',(-0.00123708373798894,-0.0354873919919925,
-0.00999869009301758));
#41118=CARTESIAN_POINT('Ctrl Pts',(-0.00135947302964417,-0.0354957125265262,
-0.0100729378051985));
#41119=CARTESIAN_POINT('Ctrl Pts',(-0.00155467588182124,-0.0355097771927162,
-0.0102155586805669));
#41120=CARTESIAN_POINT('Ctrl Pts',(-0.00163096160039099,-0.0355155180835879,
-0.0102785566945272));
#41121=CARTESIAN_POINT('Ctrl Pts',(-0.0017452270509599,-0.035524837603733,
-0.0103849146161293));
#41122=CARTESIAN_POINT('Ctrl Pts',(-0.00178578494218066,-0.0355283077406332,
-0.0104253533759202));
#41123=CARTESIAN_POINT('Ctrl Pts',(-0.00184167326752474,-0.0355333908288594,
-0.0104850426232389));
#41124=CARTESIAN_POINT('Ctrl Pts',(-0.0018581658477028,-0.0355349309641914,
-0.0105031845512746));
#41125=CARTESIAN_POINT('Ctrl Pts',(-0.00188754741012638,-0.0355377548397322,
-0.0105364752802042));
#41126=CARTESIAN_POINT('Ctrl Pts',(-0.00190052694648923,-0.0355390323817366,
-0.0105515402925441));
#41127=CARTESIAN_POINT('Ctrl Pts',(-0.00193207562071363,-0.035542211483126,
-0.0105890538428911));
#41128=CARTESIAN_POINT('Ctrl Pts',(-0.00195043406240697,-0.0355441261073228,
-0.0106116744367565));
#41129=CARTESIAN_POINT('Ctrl Pts',(-0.00207039464085095,-0.0355570500151963,
-0.0107648815084589));
#41130=CARTESIAN_POINT('Ctrl Pts',(-0.00215920659424629,-0.0355686273779125,
-0.0109049494785052));
#41131=CARTESIAN_POINT('Ctrl Pts',(-0.00227422460617676,-0.0355862994637495,
-0.0111336877263112));
#41132=CARTESIAN_POINT('Ctrl Pts',(-0.00231049485649044,-0.0355924988893119,
-0.0112167795692172));
#41133=CARTESIAN_POINT('Ctrl Pts',(-0.00236536582511525,-0.0356030297507572,
-0.0113637927026489));
#41134=CARTESIAN_POINT('Ctrl Pts',(-0.00238607533183011,-0.0356074132363114,
-0.0114268248076432));
#41135=CARTESIAN_POINT('Ctrl Pts',(-0.0024146460863224,-0.0356141811957685,
-0.0115270687056863));
#41136=CARTESIAN_POINT('Ctrl Pts',(-0.00242420686796078,-0.0356166168562833,
-0.0115637597752124));
#41137=CARTESIAN_POINT('Ctrl Pts',(-0.00244103429876844,-0.0356212659311039,
-0.0116349352548848));
#41138=CARTESIAN_POINT('Ctrl Pts',(-0.00244841362374765,-0.0356234823380514,
-0.0116693834580102));
#41139=CARTESIAN_POINT('Ctrl Pts',(-0.00246445984132205,-0.0356287793193002,
-0.0117528682945953));
#41140=CARTESIAN_POINT('Ctrl Pts',(-0.00247239480275534,-0.0356318370935566,
-0.011802031072305));
#41141=CARTESIAN_POINT('Ctrl Pts',(-0.00249743895460319,-0.0356435434805143,
-0.01199337135211));
#41142=CARTESIAN_POINT('Ctrl Pts',(-0.00250379135426237,-0.0356518805237512,
-0.0121366800145431));
#41143=CARTESIAN_POINT('Ctrl Pts',(-0.00249374192974491,-0.0356659482009488,
-0.0123782737762828));
#41144=CARTESIAN_POINT('Ctrl Pts',(-0.00248381899150705,-0.0356716752257176,
-0.0124764595943251));
#41145=CARTESIAN_POINT('Ctrl Pts',(-0.00245902330571661,-0.0356809755889593,
-0.0126302471783816));
#41146=CARTESIAN_POINT('Ctrl Pts',(-0.00244798839926214,-0.0356844409758035,
-0.0126863640542578));
#41147=CARTESIAN_POINT('Ctrl Pts',(-0.00242949036189544,-0.0356895184138586,
-0.0127659186665383));
#41148=CARTESIAN_POINT('Ctrl Pts',(-0.00242358972925878,-0.0356910578760154,
-0.0127897044799358));
#41149=CARTESIAN_POINT('Ctrl Pts',(-0.00241226803343798,-0.0356938813899903,
-0.012832632243649));
#41150=CARTESIAN_POINT('Ctrl Pts',(-0.00240696653778475,-0.035695159266899,
-0.0128518027321222));
#41151=CARTESIAN_POINT('Ctrl Pts',(-0.00239333009357419,-0.0356983405009161,
-0.0128989171330397));
#41152=CARTESIAN_POINT('Ctrl Pts',(-0.00238473416433873,-0.035700256961596,
-0.0129267814158173));
#41153=CARTESIAN_POINT('Ctrl Pts',(-0.00232419002330921,-0.0357131684996653,
-0.0131115047219413));
#41154=CARTESIAN_POINT('Ctrl Pts',(-0.00225729013692594,-0.0357247297952758,
-0.0132630231864623));
#41155=CARTESIAN_POINT('Ctrl Pts',(-0.00213128747458824,-0.0357423933445719,
-0.0134857528895373));
#41156=CARTESIAN_POINT('Ctrl Pts',(-0.00208237238712282,-0.0357485992660666,
-0.0135621976802002));
#41157=CARTESIAN_POINT('Ctrl Pts',(-0.00199065437542108,-0.0357591394836901,
-0.0136896890876594));
#41158=CARTESIAN_POINT('Ctrl Pts',(-0.0019497689239674,-0.0357635259532333,
-0.0137419969878766));
#41159=CARTESIAN_POINT('Ctrl Pts',(-0.0018823230063378,-0.0357702976110055,
-0.0138215440671646));
#41160=CARTESIAN_POINT('Ctrl Pts',(-0.00185714294379729,-0.03577273405962,
-0.0138499077608157));
#41161=CARTESIAN_POINT('Ctrl Pts',(-0.00180734432003623,-0.0357773842517837,
-0.0139034955005437));
#41162=CARTESIAN_POINT('Ctrl Pts',(-0.00178281876809443,-0.0357796009967991,
-0.0139287932588103));
#41163=CARTESIAN_POINT('Ctrl Pts',(-0.00172236512650647,-0.03578489824693,
-0.0139885686002121));
#41164=CARTESIAN_POINT('Ctrl Pts',(-0.00168592529284494,-0.0357879559651933,
-0.014022508327387));
#41165=CARTESIAN_POINT('Ctrl Pts',(-0.00154111465971355,-0.0357996412149966,
-0.0141495215312965));
#41166=CARTESIAN_POINT('Ctrl Pts',(-0.00142585847314525,-0.0358079590661767,
-0.0142343316172787));
#41167=CARTESIAN_POINT('Ctrl Pts',(-0.00121965447240412,-0.0358220203089604,
-0.0143603925353188));
#41168=CARTESIAN_POINT('Ctrl Pts',(-0.00113234839836963,-0.0358277604684135,
-0.014406896524174));
#41169=CARTESIAN_POINT('Ctrl Pts',(-0.00099048595430555,-0.0358370788396377,
-0.0144719838534337));
#41170=CARTESIAN_POINT('Ctrl Pts',(-0.00093764677714252,-0.0358405486336832,
-0.0144940628422152));
#41171=CARTESIAN_POINT('Ctrl Pts',(-0.000861165423813789,-0.0358456314624628,
-0.0145229781923017));
#41172=CARTESIAN_POINT('Ctrl Pts',(-0.000838104951708319,-0.035847171721613,
-0.0145313110323709));
#41173=CARTESIAN_POINT('Ctrl Pts',(-0.000796121931715857,-0.0358499960293268,
-0.0145457869419733));
#41174=CARTESIAN_POINT('Ctrl Pts',(-0.000777242311018188,-0.0358512738843371,
-0.0145520456093274));
#41175=CARTESIAN_POINT('Ctrl Pts',(-0.000730516408837936,-0.0358544542942129,
-0.0145669190184823));
#41176=CARTESIAN_POINT('Ctrl Pts',(-0.000702591252722598,-0.035856369931203,
-0.0145752729907218));
#41177=CARTESIAN_POINT('Ctrl Pts',(-0.000515325747385473,-0.0358692869605858,
-0.0146277453429846));
#41178=CARTESIAN_POINT('Ctrl Pts',(-0.000352101138185912,-0.035880855383117,
-0.0146564488502266));
#41179=CARTESIAN_POINT('Ctrl Pts',(-9.68669164623152E-5,-0.0358985223478047,
-0.0146756196352032));
#41180=CARTESIAN_POINT('Ctrl Pts',(-6.17677745407344E-6,-0.0359047250243374,
-0.0146774885736422));
#41181=CARTESIAN_POINT('Ctrl Pts',(0.00015072089068347,-0.0359152605467985,
-0.0146721873896958));
#41182=CARTESIAN_POINT('Ctrl Pts',(0.000216910013586982,-0.0359196455022932,
-0.01466730909817));
#41183=CARTESIAN_POINT('Ctrl Pts',(0.000320504201698942,-0.0359264153028654,
-0.0146555134792521));
#41184=CARTESIAN_POINT('Ctrl Pts',(0.000358075737165516,-0.0359288513690887,
-0.0146503673058786));
#41185=CARTESIAN_POINT('Ctrl Pts',(0.00043030114824313,-0.0359335010444259,
-0.0146387950019428));
#41186=CARTESIAN_POINT('Ctrl Pts',(0.000464964516071402,-0.0359357176501853,
-0.0146324869926315));
#41187=CARTESIAN_POINT('Ctrl Pts',(0.000548266533117582,-0.0359410148640837,
-0.014615501303359));
#41188=CARTESIAN_POINT('Ctrl Pts',(0.000596742851522922,-0.0359440726772972,
-0.0146040989705843));
#41189=CARTESIAN_POINT('Ctrl Pts',(0.000782961132498546,-0.0359557650983978,
-0.0145543835955347));
#41190=CARTESIAN_POINT('Ctrl Pts',(0.000917660488111485,-0.0359640893766176,
-0.0145057327874343));
#41191=CARTESIAN_POINT('Ctrl Pts',(0.00113715701687981,-0.0359781534616333,
-0.0144044470026523));
#41192=CARTESIAN_POINT('Ctrl Pts',(0.00122430588180622,-0.0359838899235319,
-0.0143577857336156));
#41193=CARTESIAN_POINT('Ctrl Pts',(0.00135722981399037,-0.0359932032659589,
-0.0142761396728781));
#41194=CARTESIAN_POINT('Ctrl Pts',(0.00140495166513847,-0.0359966718463788,
-0.0142445208550007));
#41195=CARTESIAN_POINT('Ctrl Pts',(0.00147150257022165,-0.0360017531454617,
-0.0141970611387035));
#41196=CARTESIAN_POINT('Ctrl Pts',(0.00149125094538757,-0.0360032931326325,
-0.0141825350016581));
#41197=CARTESIAN_POINT('Ctrl Pts',(0.00152662888027616,-0.0360061170838302,
-0.0141557017332193));
#41198=CARTESIAN_POINT('Ctrl Pts',(0.00154233056835375,-0.0360073948585694,
-0.014143494496561));
#41199=CARTESIAN_POINT('Ctrl Pts',(0.00158068010730316,-0.0360105751504573,
-0.0141129387059224));
#41200=CARTESIAN_POINT('Ctrl Pts',(0.00160315512244763,-0.0360124907513033,
-0.0140943795449346));
#41201=CARTESIAN_POINT('Ctrl Pts',(0.00175092877958355,-0.0360254080664405,
-0.0139679429082744));
#41202=CARTESIAN_POINT('Ctrl Pts',(0.00186557731151984,-0.0360369768609485,
-0.0138482624403817));
#41203=CARTESIAN_POINT('Ctrl Pts',(0.00202348288254117,-0.0360546442363876,
-0.0136468162847873));
#41204=CARTESIAN_POINT('Ctrl Pts',(0.00207548166271109,-0.0360608469707916,
-0.0135724896926553));
#41205=CARTESIAN_POINT('Ctrl Pts',(0.00215834924311046,-0.0360713825906825,
-0.013439154265334));
#41206=CARTESIAN_POINT('Ctrl Pts',(0.00219111239163233,-0.036075767587884,
-0.0133814355439498));
#41207=CARTESIAN_POINT('Ctrl Pts',(0.00223893312397356,-0.0360825374315269,
-0.0132887845890405));
#41208=CARTESIAN_POINT('Ctrl Pts',(0.00225555521490443,-0.0360849735010654,
-0.0132546992167139));
#41209=CARTESIAN_POINT('Ctrl Pts',(0.0022861127219348,-0.0360896231694473,
-0.0131882413457559));
#41210=CARTESIAN_POINT('Ctrl Pts',(0.00230015158766458,-0.0360918397652216,
-0.0131559266659638));
#41211=CARTESIAN_POINT('Ctrl Pts',(0.00233237146583091,-0.0360971369383572,
-0.0130772532706332));
#41212=CARTESIAN_POINT('Ctrl Pts',(0.00234986000222167,-0.0361001947216171,
-0.0130306263859647));
#41213=CARTESIAN_POINT('Ctrl Pts',(0.0024121387699056,-0.0361118893788775,
-0.0128481863567145));
#41214=CARTESIAN_POINT('Ctrl Pts',(0.00244663952748377,-0.0361202157318824,
-0.012709149564717));
#41215=CARTESIAN_POINT('Ctrl Pts',(0.00248455077588863,-0.0361342800876291,
-0.0124703984729227));
#41216=CARTESIAN_POINT('Ctrl Pts',(0.00249424391780315,-0.0361400146975396,
-0.0123720541215961));
#41217=CARTESIAN_POINT('Ctrl Pts',(0.00249936542594825,-0.0361478511771709,
-0.0122408961514366));
#41218=CARTESIAN_POINT('Ctrl Pts',(0.00249999999997718,-0.0361498099347429,
-0.0122083743989067));
#41219=CARTESIAN_POINT('Ctrl Pts',(0.0025,-0.0361517921417372,-0.0121758532883121));
#41220=CARTESIAN_POINT('Origin',(0.,-0.0397787743898723,-0.0121758532865581));
#41221=CARTESIAN_POINT('',(0.0025,-0.0372809459012698,-0.0121758532870403));
#41222=CARTESIAN_POINT('',(0.0025,-0.0371551761478877,-0.0121758532865581));
#41223=CARTESIAN_POINT('',(0.0025,-0.0397787743898723,-0.0121758532865581));
#41224=CARTESIAN_POINT('Ctrl Pts',(0.0025,-0.0372809459012698,-0.0121758532875225));
#41225=CARTESIAN_POINT('Ctrl Pts',(0.00249999999999826,-0.0372806546811033,
-0.0121803528786627));
#41226=CARTESIAN_POINT('Ctrl Pts',(0.00249998785222117,-0.0372803628467704,
-0.0121848524327188));
#41227=CARTESIAN_POINT('Ctrl Pts',(0.00249979491297204,-0.0372780405125425,
-0.012220585046315));
#41228=CARTESIAN_POINT('Ctrl Pts',(0.00249904097763098,-0.0372759821757314,
-0.0122518106556588));
#41229=CARTESIAN_POINT('Ctrl Pts',(0.00249141738934109,-0.037264133550365,
-0.0124295042276286));
#41230=CARTESIAN_POINT('Ctrl Pts',(0.00247225739487052,-0.0372539157741499,
-0.0125751496023748));
#41231=CARTESIAN_POINT('Ctrl Pts',(0.00241897661960846,-0.0372369329524492,
-0.0128148728429871));
#41232=CARTESIAN_POINT('Ctrl Pts',(0.00239178608095105,-0.0372301350622787,
-0.0129101256705615));
#41233=CARTESIAN_POINT('Ctrl Pts',(0.0023358517734136,-0.0372187671655393,
-0.0130695494378505));
#41234=CARTESIAN_POINT('Ctrl Pts',(0.00230992232089387,-0.037214131712778,
-0.0131345798746825));
#41235=CARTESIAN_POINT('Ctrl Pts',(0.00226553425745776,-0.0372070763977103,
-0.0132336053574228));
#41236=CARTESIAN_POINT('Ctrl Pts',(0.0022489606948044,-0.0372045976597058,
-0.0132684012130409));
#41237=CARTESIAN_POINT('Ctrl Pts',(0.0022157801777306,-0.037199913974546,
-0.0133341054345397));
#41238=CARTESIAN_POINT('Ctrl Pts',(0.00219931429537779,-0.037197704980789,
-0.0133650743164107));
#41239=CARTESIAN_POINT('Ctrl Pts',(0.00215861569823421,-0.0371925021572555,
-0.0134378813613273));
#41240=CARTESIAN_POINT('Ctrl Pts',(0.00213380997413948,-0.0371895288001224,
-0.0134793838947029));
#41241=CARTESIAN_POINT('Ctrl Pts',(0.00200365535702628,-0.0371748198049943,
-0.0136834632903798));
#41242=CARTESIAN_POINT('Ctrl Pts',(0.00188087033881847,-0.0371637343348594,
-0.0138341214708739));
#41243=CARTESIAN_POINT('Ctrl Pts',(0.00169308628104789,-0.0371484181459929,
-0.0140165306544881));
#41244=CARTESIAN_POINT('Ctrl Pts',(0.00164234107884988,-0.037144404425019,
-0.014061946896773));
#41245=CARTESIAN_POINT('Ctrl Pts',(0.00155445320821453,-0.0371375386082975,
-0.0141343664989117));
#41246=CARTESIAN_POINT('Ctrl Pts',(0.00151830554132067,-0.0371347369840929,
-0.0141625204727291));
#41247=CARTESIAN_POINT('Ctrl Pts',(0.00146306701981392,-0.0371304547336446,
-0.0142031552592165));
#41248=CARTESIAN_POINT('Ctrl Pts',(0.00144454398665757,-0.0371290186029304,
-0.0142163951200463));
#41249=CARTESIAN_POINT('Ctrl Pts',(0.00140924341705303,-0.0371262760850975,
-0.0142409056844498));
#41250=CARTESIAN_POINT('Ctrl Pts',(0.0013925054517009,-0.037124973005608,
-0.0142522291851827));
#41251=CARTESIAN_POINT('Ctrl Pts',(0.00134826588070653,-0.0371215250172291,
-0.0142813825125378));
#41252=CARTESIAN_POINT('Ctrl Pts',(0.00132054821017414,-0.0371193611075894,
-0.0142988762246454));
#41253=CARTESIAN_POINT('Ctrl Pts',(0.00119218362771139,-0.0371093504729853,
-0.0143764058496733));
#41254=CARTESIAN_POINT('Ctrl Pts',(0.00108774217604955,-0.0371012422149654,
-0.014429860032106));
#41255=CARTESIAN_POINT('Ctrl Pts',(0.000873866457429997,-0.0370851441176888,
-0.0145209872269158));
#41256=CARTESIAN_POINT('Ctrl Pts',(0.000764779457276776,-0.0370771741690067,
-0.0145587951108632));
#41257=CARTESIAN_POINT('Ctrl Pts',(0.000579813914917926,-0.0370642273627232,
-0.0146088839571667));
#41258=CARTESIAN_POINT('Ctrl Pts',(0.000505282094828397,-0.0370591545566314,
-0.0146254480109019));
#41259=CARTESIAN_POINT('Ctrl Pts',(0.000391182189236705,-0.0370516090473155,
-0.0146453750044895));
#41260=CARTESIAN_POINT('Ctrl Pts',(0.00035210422655215,-0.0370490630008536,
-0.0146512489959077));
#41261=CARTESIAN_POINT('Ctrl Pts',(0.000278343736747567,-0.0370443250435151,
-0.0146605540765496));
#41262=CARTESIAN_POINT('Ctrl Pts',(0.000243697272084421,-0.0370421274216141,
-0.0146641911015208));
#41263=CARTESIAN_POINT('Ctrl Pts',(0.000163686157660349,-0.0370371107344305,
-0.0146709030335588));
#41264=CARTESIAN_POINT('Ctrl Pts',(0.000118290461412279,-0.0370343075948691,
-0.0146734669779745));
#41265=CARTESIAN_POINT('Ctrl Pts',(-0.000116565283842468,-0.0370199869260898,
-0.0146803133806776));
#41266=CARTESIAN_POINT('Ctrl Pts',(-0.000305990309238362,-0.0370091029457028,
-0.0146642831645918));
#41267=CARTESIAN_POINT('Ctrl Pts',(-0.000564558233591509,-0.0369937077781957,
-0.0146124044464048));
#41268=CARTESIAN_POINT('Ctrl Pts',(-0.000636631090722892,-0.0369893480618895,
-0.0145945734484314));
#41269=CARTESIAN_POINT('Ctrl Pts',(-0.000754204479724711,-0.0369819752793467,
-0.0145598660050422));
#41270=CARTESIAN_POINT('Ctrl Pts',(-0.000800198539011744,-0.0369790228788128,
-0.0145448240966522));
#41271=CARTESIAN_POINT('Ctrl Pts',(-0.000867554337385341,-0.0369745584985715,
-0.0145206107627216));
#41272=CARTESIAN_POINT('Ctrl Pts',(-0.000889273459909068,-0.0369730968291128,
-0.0145124599651095));
#41273=CARTESIAN_POINT('Ctrl Pts',(-0.000929534223632692,-0.0369703404143629,
-0.014496708212092));
#41274=CARTESIAN_POINT('Ctrl Pts',(-0.00094810336952257,-0.0369690497778317,
-0.0144891845102255));
#41275=CARTESIAN_POINT('Ctrl Pts',(-0.00099577709507874,-0.0369656888467966,
-0.0144691980782198));
#41276=CARTESIAN_POINT('Ctrl Pts',(-0.00102473835286799,-0.0369636013152733,
-0.0144564044150624));
#41277=CARTESIAN_POINT('Ctrl Pts',(-0.00118234216581179,-0.0369520171889592,
-0.0143831746833694));
#41278=CARTESIAN_POINT('Ctrl Pts',(-0.00130588642945272,-0.0369421227216923,
-0.0143124057243385));
#41279=CARTESIAN_POINT('Ctrl Pts',(-0.00150590312048323,-0.0369252946900534,
-0.0141739735551446));
#41280=CARTESIAN_POINT('Ctrl Pts',(-0.0015855018253225,-0.0369183412091915,
-0.0141114192519402));
#41281=CARTESIAN_POINT('Ctrl Pts',(-0.00171406350900674,-0.0369067593774612,
-0.0139971191472443));
#41282=CARTESIAN_POINT('Ctrl Pts',(-0.0017650074598079,-0.0369020618501485,
-0.0139477938189828));
#41283=CARTESIAN_POINT('Ctrl Pts',(-0.00184040823604885,-0.0368949365726642,
-0.013868305191199));
#41284=CARTESIAN_POINT('Ctrl Pts',(-0.0018663724053138,-0.0368924479739349,
-0.0138396291836528));
#41285=CARTESIAN_POINT('Ctrl Pts',(-0.00191456237588379,-0.03688775679489,
-0.0137838575673963));
#41286=CARTESIAN_POINT('Ctrl Pts',(-0.00193690415489454,-0.0368855499164958,
-0.0137568749011753));
#41287=CARTESIAN_POINT('Ctrl Pts',(-0.00198850037393263,-0.0368803695701905,
-0.0136918249708031));
#41288=CARTESIAN_POINT('Ctrl Pts',(-0.00201724043616705,-0.036877416045971,
-0.013653366520541));
#41289=CARTESIAN_POINT('Ctrl Pts',(-0.00215749318834099,-0.0368625952633362,
-0.0134539596241547));
#41290=CARTESIAN_POINT('Ctrl Pts',(-0.00225092607795201,-0.0368513970927537,
-0.013281144317455));
#41291=CARTESIAN_POINT('Ctrl Pts',(-0.00234810262601651,-0.0368359988845671,
-0.0130366351344967));
#41292=CARTESIAN_POINT('Ctrl Pts',(-0.00237042646227637,-0.0368320281218455,
-0.0129731040245538));
#41293=CARTESIAN_POINT('Ctrl Pts',(-0.00240349211014895,-0.0368252258398617,
-0.0128652692260529));
#41294=CARTESIAN_POINT('Ctrl Pts',(-0.00241563576422337,-0.0368224435814232,
-0.0128214320749274));
#41295=CARTESIAN_POINT('Ctrl Pts',(-0.00243204017488845,-0.0368181847744732,
-0.0127552464268947));
#41296=CARTESIAN_POINT('Ctrl Pts',(-0.00243720316374131,-0.036816751998145,
-0.012733129226598));
#41297=CARTESIAN_POINT('Ctrl Pts',(-0.00244639496721373,-0.036814011094812,
-0.0126911795184535));
#41298=CARTESIAN_POINT('Ctrl Pts',(-0.0024504855641188,-0.0368127061679313,
-0.0126713629756497));
#41299=CARTESIAN_POINT('Ctrl Pts',(-0.00246060112265457,-0.0368092456332954,
-0.0126191667481233));
#41300=CARTESIAN_POINT('Ctrl Pts',(-0.00246622739419459,-0.0368070707704291,
-0.01258671446946));
#41301=CARTESIAN_POINT('Ctrl Pts',(-0.00248985220071243,-0.036796646803082,
-0.012432391259228));
#41302=CARTESIAN_POINT('Ctrl Pts',(-0.00249946638041196,-0.0367881088263436,
-0.0123094172689833));
#41303=CARTESIAN_POINT('Ctrl Pts',(-0.00250063509976623,-0.0367686412633752,
-0.0120282695279969));
#41304=CARTESIAN_POINT('Ctrl Pts',(-0.00248631645326805,-0.0367577763474871,
-0.0118705663002083));
#41305=CARTESIAN_POINT('Ctrl Pts',(-0.00244810252673388,-0.0367440701375694,
-0.0116667030251335));
#41306=CARTESIAN_POINT('Ctrl Pts',(-0.00243756442219698,-0.0367408472555988,
-0.0116184304627458));
#41307=CARTESIAN_POINT('Ctrl Pts',(-0.00241707678493895,-0.0367354016567608,
-0.0115363382703059));
#41308=CARTESIAN_POINT('Ctrl Pts',(-0.00240783031484883,-0.0367331581484131,
-0.0115023601425407));
#41309=CARTESIAN_POINT('Ctrl Pts',(-0.00238708232382073,-0.0367285311772032,
-0.0114320175024609));
#41310=CARTESIAN_POINT('Ctrl Pts',(-0.00237546026863942,-0.0367261521508053,
-0.0113956978868597));
#41311=CARTESIAN_POINT('Ctrl Pts',(-0.00234099282563577,-0.0367196326852915,
-0.0112959094654426));
#41312=CARTESIAN_POINT('Ctrl Pts',(-0.00231640249687684,-0.0367155476019408,
-0.011233075947207));
#41313=CARTESIAN_POINT('Ctrl Pts',(-0.00225189965040911,-0.0367059619142053,
-0.0110860775100659));
#41314=CARTESIAN_POINT('Ctrl Pts',(-0.0022097676897272,-0.0367005224583516,
-0.0110029972017964));
#41315=CARTESIAN_POINT('Ctrl Pts',(-0.00208302931870926,-0.0366858048066992,
-0.0107842733090032));
#41316=CARTESIAN_POINT('Ctrl Pts',(-0.00198991179638418,-0.0366766112439648,
-0.0106540960393782));
#41317=CARTESIAN_POINT('Ctrl Pts',(-0.00186546062510466,-0.0366649546425962,
-0.0105112378927437));
#41318=CARTESIAN_POINT('Ctrl Pts',(-0.00184549028730537,-0.0366630999754086,
-0.0104891247450294));
#41319=CARTESIAN_POINT('Ctrl Pts',(-0.00181147493556331,-0.0366599564426063,
-0.0104527868789954));
#41320=CARTESIAN_POINT('Ctrl Pts',(-0.00179764622375264,-0.0366586823407605,
-0.0104383644913556));
#41321=CARTESIAN_POINT('Ctrl Pts',(-0.00176668900135214,-0.0366558360342001,
-0.0104068435160508));
#41322=CARTESIAN_POINT('Ctrl Pts',(-0.00174948372368646,-0.0366542587256429,
-0.0103898263577796));
#41323=CARTESIAN_POINT('Ctrl Pts',(-0.00169246110904554,-0.0366490539337528,
-0.0103350417665158));
#41324=CARTESIAN_POINT('Ctrl Pts',(-0.00165164888087414,-0.0366453643926251,
-0.0102983371757591));
#41325=CARTESIAN_POINT('Ctrl Pts',(-0.00153957170239187,-0.0366353949112652,
-0.0102040238792165));
#41326=CARTESIAN_POINT('Ctrl Pts',(-0.0014662913717555,-0.0366290437720225,
-0.0101489392003892));
#41327=CARTESIAN_POINT('Ctrl Pts',(-0.00126233992970625,-0.0366120542218922,
-0.0100124884119692));
#41328=CARTESIAN_POINT('Ctrl Pts',(-0.00112688958707917,-0.0366014876390732,
-0.00993893992301181));
#41329=CARTESIAN_POINT('Ctrl Pts',(-0.000939911680799899,-0.036588039556691,
-0.0098587367156452));
#41330=CARTESIAN_POINT('Ctrl Pts',(-0.000893725531981653,-0.0365848006553184,
-0.00984053352286213));
#41331=CARTESIAN_POINT('Ctrl Pts',(-0.000813868931503444,-0.0365793369893011,
-0.00981177645386332));
#41332=CARTESIAN_POINT('Ctrl Pts',(-0.00078046252223885,-0.0365770910671529,
-0.00980053849471339));
#41333=CARTESIAN_POINT('Ctrl Pts',(-0.000710521477533227,-0.0365724666210445,
-0.00977864520734291));
#41334=CARTESIAN_POINT('Ctrl Pts',(-0.000673958596474642,-0.0365700923773996,
-0.00976811007037555));
#41335=CARTESIAN_POINT('Ctrl Pts',(-0.000572447072846225,-0.0365636084103815,
-0.00974135454314261));
#41336=CARTESIAN_POINT('Ctrl Pts',(-0.000507063920339304,-0.0365595529565469,
-0.0097269010527598));
#41337=CARTESIAN_POINT('Ctrl Pts',(-0.000350693671306399,-0.0365500631393257,
-0.00969886640561742));
#41338=CARTESIAN_POINT('Ctrl Pts',(-0.000259382816589645,-0.0365446880321659,
-0.00968764671185863));
#41339=CARTESIAN_POINT('Ctrl Pts',(-5.67775373194534E-6,-0.0365298811520002,
-0.00967059402151928));
#41340=CARTESIAN_POINT('Ctrl Pts',(0.000156958885541035,-0.0365205441272375,
-0.00967551177728026));
#41341=CARTESIAN_POINT('Ctrl Pts',(0.000347211629370229,-0.0365087373076922,
-0.00969990609530903));
#41342=CARTESIAN_POINT('Ctrl Pts',(0.000376404586822594,-0.0365069000521739,
-0.00970417575474959));
#41343=CARTESIAN_POINT('Ctrl Pts',(0.000425198309956907,-0.036503776112433,
-0.00971219658293011));
#41344=CARTESIAN_POINT('Ctrl Pts',(0.000444841605217921,-0.0365025037208431,
-0.00971566754709915));
#41345=CARTESIAN_POINT('Ctrl Pts',(0.000488384087035448,-0.0364996480020015,
-0.00972390004960938));
#41346=CARTESIAN_POINT('Ctrl Pts',(0.000512257208666858,-0.0364980592869458,
-0.00972877622667336));
#41347=CARTESIAN_POINT('Ctrl Pts',(0.000590792072181815,-0.0364927650463557,
-0.00974601679721187));
#41348=CARTESIAN_POINT('Ctrl Pts',(0.000645106573247217,-0.0364889946491507,
-0.00975986959177396));
#41349=CARTESIAN_POINT('Ctrl Pts',(0.000790180433086395,-0.0364787036275535,
-0.00980211102496447));
#41350=CARTESIAN_POINT('Ctrl Pts',(0.000879862224628475,-0.0364721071590439,
-0.00983387147933904));
#41351=CARTESIAN_POINT('Ctrl Pts',(0.0011042663627245,-0.0364552614039727,
-0.00992805631955577));
#41352=CARTESIAN_POINT('Ctrl Pts',(0.00123565606089343,-0.0364450846335122,
-0.0099975144137393));
#41353=CARTESIAN_POINT('Ctrl Pts',(0.00140191148913842,-0.0364319847883632,
-0.0101053160605805));
#41354=CARTESIAN_POINT('Ctrl Pts',(0.0014428811107623,-0.0364287341578732,
-0.0101336547438982));
#41355=CARTESIAN_POINT('Ctrl Pts',(0.00151136937717297,-0.0364232572464437,
-0.0101841188166146));
#41356=CARTESIAN_POINT('Ctrl Pts',(0.00153931483466529,-0.0364210095393525,
-0.0102056366401827));
#41357=CARTESIAN_POINT('Ctrl Pts',(0.00159639611881538,-0.0364163868303005,
-0.0102515450326858));
#41358=CARTESIAN_POINT('Ctrl Pts',(0.00162545013808221,-0.0364140159962058,
-0.0102760230542913));
#41359=CARTESIAN_POINT('Ctrl Pts',(0.00170385358245753,-0.0364075572963168,
-0.0103451938031733));
#41360=CARTESIAN_POINT('Ctrl Pts',(0.0017519946202944,-0.0364035229324523,
-0.0103912112804881));
#41361=CARTESIAN_POINT('Ctrl Pts',(0.00186153963496296,-0.0363941009246183,
-0.0105046347322418));
#41362=CARTESIAN_POINT('Ctrl Pts',(0.00192120729947134,-0.0363887712190662,
-0.0105735845468272));
#41363=CARTESIAN_POINT('Ctrl Pts',(0.00207750402219195,-0.0363738997735992,
-0.0107755142547893));
#41364=CARTESIAN_POINT('Ctrl Pts',(0.00216497405934135,-0.0363644604052467,
-0.0109149620133418));
#41365=CARTESIAN_POINT('Ctrl Pts',(0.00225118270482701,-0.0363525462068422,
-0.0110881794429497));
#41366=CARTESIAN_POINT('Ctrl Pts',(0.00226377103503794,-0.0363507215581471,
-0.0111146282917565));
#41367=CARTESIAN_POINT('Ctrl Pts',(0.00228413701928706,-0.0363476117173661,
-0.0111594305784336));
#41368=CARTESIAN_POINT('Ctrl Pts',(0.00229216492712964,-0.036346340477327,
-0.0111776664503463));
#41369=CARTESIAN_POINT('Ctrl Pts',(0.00230957368568218,-0.0363434775285437,
-0.0112185292969175));
#41370=CARTESIAN_POINT('Ctrl Pts',(0.00231884086723502,-0.0363418802192158,
-0.0112412000065099));
#41371=CARTESIAN_POINT('Ctrl Pts',(0.00234853982716357,-0.0363365173614458,
-0.011317015493793));
#41372=CARTESIAN_POINT('Ctrl Pts',(0.00236748801046929,-0.0363326847400693,
-0.0113707189971832));
#41373=CARTESIAN_POINT('Ctrl Pts',(0.00241395958707821,-0.0363221406850836,
-0.0115183085507397));
#41374=CARTESIAN_POINT('Ctrl Pts',(0.00243783319235319,-0.0363153497085916,
-0.0116132395647649));
#41375=CARTESIAN_POINT('Ctrl Pts',(0.00248300807545953,-0.0362985975935805,
-0.011851065506205));
#41376=CARTESIAN_POINT('Ctrl Pts',(0.00249761459014234,-0.0362887078554256,
-0.0119948904697711));
#41377=CARTESIAN_POINT('Ctrl Pts',(0.00249991037372639,-0.036278358753258,
-0.0121514091157483));
#41378=CARTESIAN_POINT('Ctrl Pts',(0.0024999999999885,-0.0362775531707368,
-0.0121636312894922));
#41379=CARTESIAN_POINT('Ctrl Pts',(0.0025,-0.0362767501454997,-0.0121758532842053));
#41380=CARTESIAN_POINT('Ctrl Pts',(0.0025,-0.0361517921417372,-0.0121758532883121));
#41381=CARTESIAN_POINT('Ctrl Pts',(0.00250000000001732,-0.0361532969286916,
-0.0121511649771985));
#41382=CARTESIAN_POINT('Ctrl Pts',(0.0024996342921978,-0.0361548152361512,
-0.0121264770364312));
#41383=CARTESIAN_POINT('Ctrl Pts',(0.00249817675417057,-0.036157873977649,
-0.0120772944971944));
#41384=CARTESIAN_POINT('Ctrl Pts',(0.00249709026948674,-0.0361594138859829,
-0.0120528044824867));
#41385=CARTESIAN_POINT('Ctrl Pts',(0.00249447021013777,-0.0361622378119806,
-0.0120084794140612));
#41386=CARTESIAN_POINT('Ctrl Pts',(0.00249305971196675,-0.0361635156435239,
-0.0119886399896802));
#41387=CARTESIAN_POINT('Ctrl Pts',(0.00248899862140974,-0.036166696268289,
-0.0119397693412445));
#41388=CARTESIAN_POINT('Ctrl Pts',(0.00248607674588793,-0.0361686121509704,
-0.0119107646084144));
#41389=CARTESIAN_POINT('Ctrl Pts',(0.0024632065078464,-0.0361815275415674,
-0.0117176620029709));
#41390=CARTESIAN_POINT('Ctrl Pts',(0.0024275324011118,-0.0361930938416531,
-0.0115558482267804));
#41391=CARTESIAN_POINT('Ctrl Pts',(0.00234797607685132,-0.036210759873643,
-0.0113125885522278));
#41392=CARTESIAN_POINT('Ctrl Pts',(0.0023151306115756,-0.0362169635994065,
-0.0112280188199955));
#41393=CARTESIAN_POINT('Ctrl Pts',(0.00225041533685465,-0.0362275006411803,
-0.0110849671775967));
#41394=CARTESIAN_POINT('Ctrl Pts',(0.00222067230207197,-0.0362318860880483,
-0.0110256283119983));
#41395=CARTESIAN_POINT('Ctrl Pts',(0.00217027473221903,-0.0362386564823279,
-0.0109343439909819));
#41396=CARTESIAN_POINT('Ctrl Pts',(0.00215119460944113,-0.0362410926642295,
-0.0109015692728963));
#41397=CARTESIAN_POINT('Ctrl Pts',(0.00211296375747703,-0.0362457424840735,
-0.0108392063025702));
#41398=CARTESIAN_POINT('Ctrl Pts',(0.00209391866524951,-0.0362479591203712,
-0.0108095642179501));
#41399=CARTESIAN_POINT('Ctrl Pts',(0.00204646243198919,-0.0362532562979283,
-0.0107390269112703));
#41400=CARTESIAN_POINT('Ctrl Pts',(0.00201744330125472,-0.0362563140474926,
-0.0106985579403063));
#41401=CARTESIAN_POINT('Ctrl Pts',(0.00190053039245494,-0.0362680032982854,
-0.0105453920086602));
#41402=CARTESIAN_POINT('Ctrl Pts',(0.00180424597537692,-0.0362763247494811,
-0.010439442936532));
#41403=CARTESIAN_POINT('Ctrl Pts',(0.00162696619575666,-0.0362903875899586,
-0.0102751316646094));
#41404=CARTESIAN_POINT('Ctrl Pts',(0.00155058886803671,-0.0362961256843174,
-0.0102123273989611));
#41405=CARTESIAN_POINT('Ctrl Pts',(0.00142441094666287,-0.0363054412430823,
-0.010120535755744));
#41406=CARTESIAN_POINT('Ctrl Pts',(0.00137698190117222,-0.0363089103531119,
-0.0100884633952098));
#41407=CARTESIAN_POINT('Ctrl Pts',(0.00130772902535701,-0.036313992309463,
-0.0100450210835914));
#41408=CARTESIAN_POINT('Ctrl Pts',(0.00128677059063228,-0.0363155324036604,
-0.0100322995969759));
#41409=CARTESIAN_POINT('Ctrl Pts',(0.00124847617560075,-0.0363183564947223,
-0.0100098193835235));
#41410=CARTESIAN_POINT('Ctrl Pts',(0.00123120507554796,-0.0363196343005626,
-0.00999995586350741));
#41411=CARTESIAN_POINT('Ctrl Pts',(0.00118833787072059,-0.0363228146290413,
-0.00997614816207177));
#41412=CARTESIAN_POINT('Ctrl Pts',(0.00116261294324202,-0.0363247302345519,
-0.00996244403812264));
#41413=CARTESIAN_POINT('Ctrl Pts',(0.000989394468147815,-0.0363376475562736,
-0.00987402021924515));
#41414=CARTESIAN_POINT('Ctrl Pts',(0.000835048476674809,-0.0363492163461727,
-0.00981364558938359));
#41415=CARTESIAN_POINT('Ctrl Pts',(0.00058862236812525,-0.0363668836383153,
-0.00974444656543307));
#41416=CARTESIAN_POINT('Ctrl Pts',(0.00050008768365968,-0.0363730862942786,
-0.00972470467635234));
#41417=CARTESIAN_POINT('Ctrl Pts',(0.00034523322347434,-0.0363836218073554,
-0.00969891671423938));
#41418=CARTESIAN_POINT('Ctrl Pts',(0.000279384082836112,-0.036388006773449,
-0.00969062762879891));
#41419=CARTESIAN_POINT('Ctrl Pts',(0.000175500231029585,-0.0363947765997946,
-0.00968173273989668));
#41420=CARTESIAN_POINT('Ctrl Pts',(0.000137652102716281,-0.0363972126811644,
-0.00967935778649933));
#41421=CARTESIAN_POINT('Ctrl Pts',(6.45631858851483E-5,-0.0364018623922129,
-0.00967643883724852));
#41422=CARTESIAN_POINT('Ctrl Pts',(2.93364191766409E-5,-0.0364040790184051,
-0.00967577717484428));
#41423=CARTESIAN_POINT('Ctrl Pts',(-5.56805786665413E-5,-0.0364093763025371,
-0.00967597761172541));
#41424=CARTESIAN_POINT('Ctrl Pts',(-0.000105454781875508,-0.0364124341648461,
-0.00967758218416136));
#41425=CARTESIAN_POINT('Ctrl Pts',(-0.000297933856858051,-0.0364241332866678,
-0.00968955054345357));
#41426=CARTESIAN_POINT('Ctrl Pts',(-0.000439695786970914,-0.0364324636511113,
-0.00971066805494442));
#41427=CARTESIAN_POINT('Ctrl Pts',(-0.000674889545747243,-0.0364465292891003,
-0.00976664935470826));
#41428=CARTESIAN_POINT('Ctrl Pts',(-0.000769454155484879,-0.0364522610894565,
-0.00979516476164522));
#41429=CARTESIAN_POINT('Ctrl Pts',(-0.000915778419033223,-0.0364615680289228,
-0.00984891914892726));
#41430=CARTESIAN_POINT('Ctrl Pts',(-0.000968779356184011,-0.0364650350507535,
-0.00987048169580886));
#41431=CARTESIAN_POINT('Ctrl Pts',(-0.00104336442719228,-0.0364701145110101,
-0.00990385163642731));
#41432=CARTESIAN_POINT('Ctrl Pts',(-0.00106558944021804,-0.0364716542938449,
-0.00991419021192531));
#41433=CARTESIAN_POINT('Ctrl Pts',(-0.00110556773651197,-0.036474478114334,
-0.00993350727543451));
#41434=CARTESIAN_POINT('Ctrl Pts',(-0.0011233719444242,-0.0364757559694346,
-0.00994237370716314));
#41435=CARTESIAN_POINT('Ctrl Pts',(-0.00116700820236698,-0.0364789368402748,
-0.00996475812456358));
#41436=CARTESIAN_POINT('Ctrl Pts',(-0.00119271230461342,-0.0364808529507348,
-0.00997851691147382));
#41437=CARTESIAN_POINT('Ctrl Pts',(-0.00136249481386875,-0.0364937666334979,
-0.0100732540690368));
#41438=CARTESIAN_POINT('Ctrl Pts',(-0.00149847041161189,-0.036505330758113,
-0.0101678950466629));
#41439=CARTESIAN_POINT('Ctrl Pts',(-0.00169303184232238,-0.0365229956639271,
-0.0103341521300499));
#41440=CARTESIAN_POINT('Ctrl Pts',(-0.00175870768402333,-0.0365292003026396,
-0.0103967609568813));
#41441=CARTESIAN_POINT('Ctrl Pts',(-0.00186630593728238,-0.0365397386233811,
-0.0105111297115197));
#41442=CARTESIAN_POINT('Ctrl Pts',(-0.00190983191449707,-0.036544124456584,
-0.0105612493828944));
#41443=CARTESIAN_POINT('Ctrl Pts',(-0.00197501891260304,-0.0365508952693436,
-0.0106426415966734));
#41444=CARTESIAN_POINT('Ctrl Pts',(-0.00199804702552586,-0.0365533314959028,
-0.0106727744044653));
#41445=CARTESIAN_POINT('Ctrl Pts',(-0.00204112950067508,-0.0365579813068854,
-0.0107318895407052));
#41446=CARTESIAN_POINT('Ctrl Pts',(-0.00206127394947851,-0.036560197891696,
-0.010760794687589));
#41447=CARTESIAN_POINT('Ctrl Pts',(-0.00210839480464267,-0.0365654947794551,
-0.0108315506887275));
#41448=CARTESIAN_POINT('Ctrl Pts',(-0.0021347455600349,-0.0365685522962797,
-0.0108738010540575));
#41449=CARTESIAN_POINT('Ctrl Pts',(-0.0022316391465855,-0.0365802238850457,
-0.0110400169025678));
#41450=CARTESIAN_POINT('Ctrl Pts',(-0.00229278851383359,-0.0365885293957336,
-0.0111691442498614));
#41451=CARTESIAN_POINT('Ctrl Pts',(-0.00237717351599074,-0.0366025875573592,
-0.0113955656445488));
#41452=CARTESIAN_POINT('Ctrl Pts',(-0.00240620629511256,-0.036608337229675,
-0.011490308210455));
#41453=CARTESIAN_POINT('Ctrl Pts',(-0.0024430533413161,-0.0366176686467207,
-0.0116422104894747));
#41454=CARTESIAN_POINT('Ctrl Pts',(-0.00245464291861119,-0.0366211415914102,
-0.0116983478731764));
#41455=CARTESIAN_POINT('Ctrl Pts',(-0.00246842316546757,-0.036626228096677,
-0.0117790049578425));
#41456=CARTESIAN_POINT('Ctrl Pts',(-0.00247219739638716,-0.0366277687225857,
-0.0118032389482794));
#41457=CARTESIAN_POINT('Ctrl Pts',(-0.00247838547372813,-0.0366305932312941,
-0.0118472182194491));
#41458=CARTESIAN_POINT('Ctrl Pts',(-0.00248092123203021,-0.0366318709074048,
-0.0118669434164088));
#41459=CARTESIAN_POINT('Ctrl Pts',(-0.00248659076542711,-0.0366350500853271,
-0.0119156322172972));
#41460=CARTESIAN_POINT('Ctrl Pts',(-0.00248945399433441,-0.0366369646464156,
-0.0119446233639717));
#41461=CARTESIAN_POINT('Ctrl Pts',(-0.00250519307016456,-0.0366498895321647,
-0.0121385867037762));
#41462=CARTESIAN_POINT('Ctrl Pts',(-0.00250216785424727,-0.0366614680161941,
-0.0123044278731853));
#41463=CARTESIAN_POINT('Ctrl Pts',(-0.00247217179840446,-0.0366791403559196,
-0.0125586995973125));
#41464=CARTESIAN_POINT('Ctrl Pts',(-0.00245667809783091,-0.0366853389791898,
-0.0126480181772522));
#41465=CARTESIAN_POINT('Ctrl Pts',(-0.00242150302932559,-0.0366958687944396,
-0.0128009296560709));
#41466=CARTESIAN_POINT('Ctrl Pts',(-0.00240407065510009,-0.0367002520094542,
-0.0128649417761621));
#41467=CARTESIAN_POINT('Ctrl Pts',(-0.00237270290059417,-0.0367070198541235,
-0.0129643444210921));
#41468=CARTESIAN_POINT('Ctrl Pts',(-0.00236047245004971,-0.0367094556523334,
-0.0130002363207279));
#41469=CARTESIAN_POINT('Ctrl Pts',(-0.00233531102820602,-0.0367141051878846,
-0.0130689174097979));
#41470=CARTESIAN_POINT('Ctrl Pts',(-0.00232249393527816,-0.0367163219137734,
-0.0131017383997141));
#41471=CARTESIAN_POINT('Ctrl Pts',(-0.0022898952971021,-0.0367216200561394,
-0.0131802732696674));
#41472=CARTESIAN_POINT('Ctrl Pts',(-0.00226943282765788,-0.0367246786571308,
-0.0132256890407943));
#41473=CARTESIAN_POINT('Ctrl Pts',(-0.00218425900271001,-0.0367364794608299,
-0.0134005810244449));
#41474=CARTESIAN_POINT('Ctrl Pts',(-0.00210971157630988,-0.0367449020013716,
-0.0135249519644654));
#41475=CARTESIAN_POINT('Ctrl Pts',(-0.00196762097177015,-0.0367589962287997,
-0.0137211612422479));
#41476=CARTESIAN_POINT('Ctrl Pts',(-0.00190585685069581,-0.03676466239984,
-0.0137967224149057));
#41477=CARTESIAN_POINT('Ctrl Pts',(-0.00180136522244201,-0.0367738792902254,
-0.0139103021666383));
#41478=CARTESIAN_POINT('Ctrl Pts',(-0.00176147677090706,-0.0367773243908369,
-0.0139507978499153));
#41479=CARTESIAN_POINT('Ctrl Pts',(-0.00170249836123113,-0.03678237778154,
-0.014006726737373));
#41480=CARTESIAN_POINT('Ctrl Pts',(-0.00168450494104781,-0.0367839144467999,
-0.0140232951013958));
#41481=CARTESIAN_POINT('Ctrl Pts',(-0.00165143667225138,-0.0367867357696183,
-0.0140528596616974));
#41482=CARTESIAN_POINT('Ctrl Pts',(-0.00163644482265526,-0.0367880143348335,
-0.0140659443583956));
#41483=CARTESIAN_POINT('Ctrl Pts',(-0.00160265868890948,-0.0367908934064162,
-0.0140947292020543));
#41484=CARTESIAN_POINT('Ctrl Pts',(-0.00158378709633748,-0.0367924995960476,
-0.0141103346075932));
#41485=CARTESIAN_POINT('Ctrl Pts',(-0.00150439359046006,-0.0367992384943448,
-0.0141740466991031));
#41486=CARTESIAN_POINT('Ctrl Pts',(-0.00144188970856939,-0.0368044990645285,
-0.0142196069584674));
#41487=CARTESIAN_POINT('Ctrl Pts',(-0.00125115314914072,-0.0368202172315811,
-0.0143455293211941));
#41488=CARTESIAN_POINT('Ctrl Pts',(-0.00111761228202061,-0.0368307807472205,
-0.0144172425660154));
#41489=CARTESIAN_POINT('Ctrl Pts',(-0.00089827136869339,-0.0368469809664464,
-0.0145105249262246));
#41490=CARTESIAN_POINT('Ctrl Pts',(-0.000816403892349176,-0.0368528012427316,
-0.0145403977517451));
#41491=CARTESIAN_POINT('Ctrl Pts',(-0.000693967532365007,-0.036861166894107,
-0.0145779539541803));
#41492=CARTESIAN_POINT('Ctrl Pts',(-0.00065450752144139,-0.0368638134889614,
-0.0145890044989252));
#41493=CARTESIAN_POINT('Ctrl Pts',(-0.000581250311792042,-0.0368686399286667,
-0.0146075904271785));
#41494=CARTESIAN_POINT('Ctrl Pts',(-0.000547534542512971,-0.0368708278713999,
-0.0146154031545027));
#41495=CARTESIAN_POINT('Ctrl Pts',(-0.000470743990796697,-0.0368757410587395,
-0.014631525008002));
#41496=CARTESIAN_POINT('Ctrl Pts',(-0.000427590417983763,-0.0368784526320793,
-0.0146394056596525));
#41497=CARTESIAN_POINT('Ctrl Pts',(-0.000269596982441658,-0.036888226000936,
-0.0146639812537609));
#41498=CARTESIAN_POINT('Ctrl Pts',(-0.000153835917919869,-0.0368950843502155,
-0.0146738127984216));
#41499=CARTESIAN_POINT('Ctrl Pts',(0.000126232869975961,-0.0369114508375757,
-0.0146780480195134));
#41500=CARTESIAN_POINT('Ctrl Pts',(0.000290097198179099,-0.0369208319654994,
-0.0146643764553365));
#41501=CARTESIAN_POINT('Ctrl Pts',(0.000492094376711041,-0.0369332714562593,
-0.014627292221559));
#41502=CARTESIAN_POINT('Ctrl Pts',(0.000532569559533968,-0.0369358105335989,
-0.0146188184863748));
#41503=CARTESIAN_POINT('Ctrl Pts',(0.000594191105201978,-0.036939772999877,
-0.0146043135513696));
#41504=CARTESIAN_POINT('Ctrl Pts',(0.00061550066413709,-0.0369411612306676,
-0.0145990002442089));
#41505=CARTESIAN_POINT('Ctrl Pts',(0.000656931831980199,-0.0369439003268179,
-0.0145880880822758));
#41506=CARTESIAN_POINT('Ctrl Pts',(0.000677058449612257,-0.0369452497874767,
-0.0145825165150732));
#41507=CARTESIAN_POINT('Ctrl Pts',(0.000731286758599727,-0.0369489326942958,
-0.0145667706992798));
#41508=CARTESIAN_POINT('Ctrl Pts',(0.00076524405256289,-0.0369512894517418,
-0.0145561195837569));
#41509=CARTESIAN_POINT('Ctrl Pts',(0.000843357924680048,-0.0369568112282263,
-0.0145297740096758));
#41510=CARTESIAN_POINT('Ctrl Pts',(0.000887323544886222,-0.0369599946877288,
-0.0145135555439412));
#41511=CARTESIAN_POINT('Ctrl Pts',(0.00105743149094895,-0.0369725494534005,
-0.0144453143032938));
#41512=CARTESIAN_POINT('Ctrl Pts',(0.00117968727277185,-0.0369820782492673,
-0.0143842359263524));
#41513=CARTESIAN_POINT('Ctrl Pts',(0.00138750242481359,-0.0369987432919234,
-0.014258208031137));
#41514=CARTESIAN_POINT('Ctrl Pts',(0.00147503332822346,-0.0370059338421185,
-0.0141971512952803));
#41515=CARTESIAN_POINT('Ctrl Pts',(0.00159269736944193,-0.037015807946753,
-0.0141033486013389));
#41516=CARTESIAN_POINT('Ctrl Pts',(0.00162626396876562,-0.0370186519954304,
-0.0140751134028164));
#41517=CARTESIAN_POINT('Ctrl Pts',(0.00168495799956095,-0.0370236786460554,
-0.0140230441184259));
#41518=CARTESIAN_POINT('Ctrl Pts',(0.00171036523524432,-0.0370258736920758,
-0.0139995441540643));
#41519=CARTESIAN_POINT('Ctrl Pts',(0.00176477311080598,-0.037030621518774,
-0.0139470830045284));
#41520=CARTESIAN_POINT('Ctrl Pts',(0.00179356633607497,-0.0370331650295079,
-0.0139179207185068));
#41521=CARTESIAN_POINT('Ctrl Pts',(0.00188129117384234,-0.0370410299940846,
-0.0138245896676529));
#41522=CARTESIAN_POINT('Ctrl Pts',(0.00193759644071001,-0.0370462472017684,
-0.0137580385614667));
#41523=CARTESIAN_POINT('Ctrl Pts',(0.002081919231378,-0.0370603246273959,
-0.0135681633444368));
#41524=CARTESIAN_POINT('Ctrl Pts',(0.00216238379915213,-0.0370689902042344,
-0.0134395817250453));
#41525=CARTESIAN_POINT('Ctrl Pts',(0.00226556750569695,-0.0370824683125001,
-0.0132356461609043));
#41526=CARTESIAN_POINT('Ctrl Pts',(0.00229720156907751,-0.0370870846129693,
-0.013165206580885));
#41527=CARTESIAN_POINT('Ctrl Pts',(0.00233450993633415,-0.0370933687283898,
-0.0130706508566329));
#41528=CARTESIAN_POINT('Ctrl Pts',(0.00234315989326879,-0.0370948974266925,
-0.0130477483184021));
#41529=CARTESIAN_POINT('Ctrl Pts',(0.00235822829673303,-0.0370977017584978,
-0.0130060070404093));
#41530=CARTESIAN_POINT('Ctrl Pts',(0.00236476048704052,-0.0370989712793348,
-0.0129872124931785));
#41531=CARTESIAN_POINT('Ctrl Pts',(0.00237882319653925,-0.0371018307596736,
-0.0129451378391678));
#41532=CARTESIAN_POINT('Ctrl Pts',(0.00238623703721665,-0.0371034263155972,
-0.0129218232702511));
#41533=CARTESIAN_POINT('Ctrl Pts',(0.00240974314132829,-0.0371087828488224,
-0.0128439640018595));
#41534=CARTESIAN_POINT('Ctrl Pts',(0.00242431555260982,-0.037112610749602,
-0.0127889822036274));
#41535=CARTESIAN_POINT('Ctrl Pts',(0.00245877930717899,-0.0371231378500889,
-0.0126383855162499));
#41536=CARTESIAN_POINT('Ctrl Pts',(0.0024749645776264,-0.0371299163886139,
-0.0125420239951231));
#41537=CARTESIAN_POINT('Ctrl Pts',(0.00249515434765317,-0.037142895916894,
-0.0123555552999207));
#41538=CARTESIAN_POINT('Ctrl Pts',(0.0025,-0.0371490887583808,-0.0122657206983139));
#41539=CARTESIAN_POINT('Ctrl Pts',(0.0025,-0.0371551761478877,-0.0121758532865581));
#41540=CARTESIAN_POINT('Origin',(0.,-0.0397787743898723,-0.0121758532865581));
#41541=CARTESIAN_POINT('',(0.0025,-0.0382770671668707,-0.0121758532865581));
#41542=CARTESIAN_POINT('',(0.0025,-0.0381539840246788,-0.0121758532868784));
#41543=CARTESIAN_POINT('',(0.0025,-0.0397787743898723,-0.0121758532865581));
#41544=CARTESIAN_POINT('Ctrl Pts',(0.0025,-0.0382770671668707,-0.0121758532865581));
#41545=CARTESIAN_POINT('Ctrl Pts',(0.0025,-0.038266648351978,-0.0123484233248802));
#41546=CARTESIAN_POINT('Ctrl Pts',(0.00248213258965094,-0.0382567310896037,
-0.0125205849801563));
#41547=CARTESIAN_POINT('Ctrl Pts',(0.00243165258255063,-0.0382423854219848,
-0.0127609933562431));
#41548=CARTESIAN_POINT('Ctrl Pts',(0.00241354186202213,-0.0382380963272977,
-0.0128317021372035));
#41549=CARTESIAN_POINT('Ctrl Pts',(0.00237847075891303,-0.0382308262909001,
-0.0129473250147727));
#41550=CARTESIAN_POINT('Ctrl Pts',(0.00236326300636025,-0.0382279038854537,
-0.0129927248310423));
#41551=CARTESIAN_POINT('Ctrl Pts',(0.00233879518817045,-0.038223475770528,
-0.0130593527232582));
#41552=CARTESIAN_POINT('Ctrl Pts',(0.00233052768115301,-0.0382220191983679,
-0.0130809360570954));
#41553=CARTESIAN_POINT('Ctrl Pts',(0.00231452670270875,-0.0382192660654279,
-0.0131210351070867));
#41554=CARTESIAN_POINT('Ctrl Pts',(0.00230686748142584,-0.0382179734620846,
-0.0131395777521876));
#41555=CARTESIAN_POINT('Ctrl Pts',(0.00228647242581149,-0.038214597660604,
-0.0131873168000068));
#41556=CARTESIAN_POINT('Ctrl Pts',(0.0022734004952124,-0.0382124969175176,
-0.0132163649697932));
#41557=CARTESIAN_POINT('Ctrl Pts',(0.00220025267773399,-0.0382010942503547,
-0.0133709499643583));
#41558=CARTESIAN_POINT('Ctrl Pts',(0.00213033134399354,-0.0381914124996758,
-0.0134915475237513));
#41559=CARTESIAN_POINT('Ctrl Pts',(0.00199201142202049,-0.0381746777935562,
-0.013689932750067));
#41560=CARTESIAN_POINT('Ctrl Pts',(0.00192813818566363,-0.0381676127607061,
-0.0137704793170425));
#41561=CARTESIAN_POINT('Ctrl Pts',(0.00181169201214085,-0.0381558784733875,
-0.0139000589343368));
#41562=CARTESIAN_POINT('Ctrl Pts',(0.00176163394186917,-0.0381511372952276,
-0.0139511731146526));
#41563=CARTESIAN_POINT('Ctrl Pts',(0.00168115620616752,-0.03814396308667,
-0.0140265875247387));
#41564=CARTESIAN_POINT('Ctrl Pts',(0.00165224924064926,-0.0381414677931332,
-0.0140524395821871));
#41565=CARTESIAN_POINT('Ctrl Pts',(0.00159613119701894,-0.0381367717600846,
-0.0141003245865437));
#41566=CARTESIAN_POINT('Ctrl Pts',(0.00156903617274202,-0.0381345665462568,
-0.0141224786392016));
#41567=CARTESIAN_POINT('Ctrl Pts',(0.00150388348262836,-0.0381294022216525,
-0.0141735057746038));
#41568=CARTESIAN_POINT('Ctrl Pts',(0.00146544531958654,-0.0381264626895305,
-0.0142018719071543));
#41569=CARTESIAN_POINT('Ctrl Pts',(0.00126422037268961,-0.0381115638696141,
-0.014341644368517));
#41570=CARTESIAN_POINT('Ctrl Pts',(0.00108948233514589,-0.03810028716686,
-0.0144345998725599));
#41571=CARTESIAN_POINT('Ctrl Pts',(0.000843375268429188,-0.0380848313346593,
-0.014530248968462));
#41572=CARTESIAN_POINT('Ctrl Pts',(0.000780180522547825,-0.0380808902953429,
-0.0145519379353241));
#41573=CARTESIAN_POINT('Ctrl Pts',(0.000672841287146767,-0.0380741320873495,
-0.0145840335931913));
#41574=CARTESIAN_POINT('Ctrl Pts',(0.00062914429002299,-0.038071363357087,
-0.0145958170698696));
#41575=CARTESIAN_POINT('Ctrl Pts',(0.00056311357261925,-0.038067121015749,
-0.0146117139289849));
#41576=CARTESIAN_POINT('Ctrl Pts',(0.000541002316568172,-0.0380656906816978,
-0.0146167200117643));
#41577=CARTESIAN_POINT('Ctrl Pts',(0.000499014490772209,-0.0380629509935083,
-0.0146256277130373));
#41578=CARTESIAN_POINT('Ctrl Pts',(0.000479153134571793,-0.0380616447631206,
-0.0146295896961051));
#41579=CARTESIAN_POINT('Ctrl Pts',(0.00042676264808953,-0.0380581754496267,
-0.0146393803772029));
#41580=CARTESIAN_POINT('Ctrl Pts',(0.000394162893044924,-0.0380559929334715,
-0.0146448059910956));
#41581=CARTESIAN_POINT('Ctrl Pts',(0.000237681942354664,-0.0380454325208168,
-0.0146676713405692));
#41582=CARTESIAN_POINT('Ctrl Pts',(0.0001127222718948,-0.0380367573077866,
-0.0146764410897942));
#41583=CARTESIAN_POINT('Ctrl Pts',(-0.00012229675935095,-0.0380204846613085,
-0.0146752792485404));
#41584=CARTESIAN_POINT('Ctrl Pts',(-0.000232086539329571,-0.038012900235242,
-0.0146674844334593));
#41585=CARTESIAN_POINT('Ctrl Pts',(-0.000414653142569712,-0.0380004645323029,
-0.0146423464343174));
#41586=CARTESIAN_POINT('Ctrl Pts',(-0.000487809575432174,-0.0379955279587467,
-0.0146289267159705));
#41587=CARTESIAN_POINT('Ctrl Pts',(-0.000598483184159789,-0.0379881343249413,
-0.0146034767591937));
#41588=CARTESIAN_POINT('Ctrl Pts',(-0.00063649064759546,-0.0379856085767315,
-0.0145937899647144));
#41589=CARTESIAN_POINT('Ctrl Pts',(-0.000707857580316338,-0.0379808875062097,
-0.0145738014226241));
#41590=CARTESIAN_POINT('Ctrl Pts',(-0.000741259410710683,-0.0379786869673909,
-0.0145636875132853));
#41591=CARTESIAN_POINT('Ctrl Pts',(-0.000818981756903161,-0.037973582053773,
-0.014538365392493));
#41592=CARTESIAN_POINT('Ctrl Pts',(-0.000863108846696353,-0.0379706958386521,
-0.0145226038289881));
#41593=CARTESIAN_POINT('Ctrl Pts',(-0.00107697192358637,-0.037956724362385,
-0.014439365787931));
#41594=CARTESIAN_POINT('Ctrl Pts',(-0.00123940278310876,-0.0379462140620093,
-0.0143546703154158));
#41595=CARTESIAN_POINT('Ctrl Pts',(-0.00145520677732491,-0.0379310638560855,
-0.0142101379644974));
#41596=CARTESIAN_POINT('Ctrl Pts',(-0.00151722691609498,-0.0379265429119622,
-0.0141643105092558));
#41597=CARTESIAN_POINT('Ctrl Pts',(-0.00161546144222776,-0.0379189366981224,
-0.0140844490439993));
#41598=CARTESIAN_POINT('Ctrl Pts',(-0.00165295557991421,-0.0379159170948097,
-0.0140520703874035));
#41599=CARTESIAN_POINT('Ctrl Pts',(-0.001706697726981,-0.0379113716998078,
-0.0140027987497902));
#41600=CARTESIAN_POINT('Ctrl Pts',(-0.00172371144335557,-0.0379098989077076,
-0.0139867551672282));
#41601=CARTESIAN_POINT('Ctrl Pts',(-0.00175483575075298,-0.0379071355314612,
-0.0139565695695701));
#41602=CARTESIAN_POINT('Ctrl Pts',(-0.00176900621429655,-0.0379058493936831,
-0.0139424930062018));
#41603=CARTESIAN_POINT('Ctrl Pts',(-0.00180489770710741,-0.0379025216360983,
-0.0139059745726439));
#41604=CARTESIAN_POINT('Ctrl Pts',(-0.00182636912948285,-0.0379004634545333,
-0.0138832931810054));
#41605=CARTESIAN_POINT('Ctrl Pts',(-0.00194621227548652,-0.037888613615882,
-0.0137518492914627));
#41606=CARTESIAN_POINT('Ctrl Pts',(-0.00203528250209412,-0.0378783943318016,
-0.0136350056196532));
#41607=CARTESIAN_POINT('Ctrl Pts',(-0.00216644150800256,-0.037861410949501,
-0.0134273814148368));
#41608=CARTESIAN_POINT('Ctrl Pts',(-0.00221427918536977,-0.037854613938942,
-0.013340654498436));
#41609=CARTESIAN_POINT('Ctrl Pts',(-0.00228695182231855,-0.0378432472822442,
-0.0131881511219335));
#41610=CARTESIAN_POINT('Ctrl Pts',(-0.00231438818850902,-0.0378386122107011,
-0.0131237479741729));
#41611=CARTESIAN_POINT('Ctrl Pts',(-0.00235268953567896,-0.0378315573417044,
-0.0130222200966319));
#41612=CARTESIAN_POINT('Ctrl Pts',(-0.00236545581178896,-0.0378290786802289,
-0.0129858556904086));
#41613=CARTESIAN_POINT('Ctrl Pts',(-0.00238822519367106,-0.037824395079808,
-0.0129158602134208));
#41614=CARTESIAN_POINT('Ctrl Pts',(-0.00239837098322131,-0.0378221860956407,
-0.0128822856242248));
#41615=CARTESIAN_POINT('Ctrl Pts',(-0.00242081373804952,-0.0378169832103377,
-0.0128019503705473));
#41616=CARTESIAN_POINT('Ctrl Pts',(-0.0024324675822765,-0.037814009784381,
-0.0127550239281337));
#41617=CARTESIAN_POINT('Ctrl Pts',(-0.00248397054685601,-0.0377993005476244,
-0.0125185110836304));
#41618=CARTESIAN_POINT('Ctrl Pts',(-0.00250304935813366,-0.0377882149399982,
-0.0123250908286065));
#41619=CARTESIAN_POINT('Ctrl Pts',(-0.00249839422320036,-0.0377728984480414,
-0.0120633319114935));
#41620=CARTESIAN_POINT('Ctrl Pts',(-0.0024944038416649,-0.0377688845626646,
-0.0119953450407695));
#41621=CARTESIAN_POINT('Ctrl Pts',(-0.00248309530968993,-0.0377620184978214,
-0.011882022402238));
#41622=CARTESIAN_POINT('Ctrl Pts',(-0.0024772941505594,-0.0377592167969208,
-0.0118365716291559));
#41623=CARTESIAN_POINT('Ctrl Pts',(-0.00246674595997307,-0.0377549344726481,
-0.0117688118173486));
#41624=CARTESIAN_POINT('Ctrl Pts',(-0.00246293679715169,-0.0377534983494909,
-0.0117463644825976));
#41625=CARTESIAN_POINT('Ctrl Pts',(-0.00245516903720368,-0.0377507558901246,
-0.0117040976486968));
#41626=CARTESIAN_POINT('Ctrl Pts',(-0.00245127573949789,-0.0377494528624718,
-0.0116842685808227));
#41627=CARTESIAN_POINT('Ctrl Pts',(-0.00244043933679202,-0.0377460051162837,
-0.0116324106847229));
#41628=CARTESIAN_POINT('Ctrl Pts',(-0.00243310615354872,-0.0377438414008662,
-0.0116004679998408));
#41629=CARTESIAN_POINT('Ctrl Pts',(-0.00239825207901131,-0.0377342614452151,
-0.0114612551109804));
#41630=CARTESIAN_POINT('Ctrl Pts',(-0.00236425029004917,-0.0377266129669288,
-0.0113557431978358));
#41631=CARTESIAN_POINT('Ctrl Pts',(-0.00227924626902856,-0.0377106726335527,
-0.0111417743626027));
#41632=CARTESIAN_POINT('Ctrl Pts',(-0.00222721189728784,-0.0377024004858524,
-0.0110340066596268));
#41633=CARTESIAN_POINT('Ctrl Pts',(-0.00212891630433674,-0.0376890583085457,
-0.0108629310756423));
#41634=CARTESIAN_POINT('Ctrl Pts',(-0.00208703917488962,-0.0376838835626023,
-0.0107973327615932));
#41635=CARTESIAN_POINT('Ctrl Pts',(-0.00201925249087216,-0.0376762247688677,
-0.0107013372466339));
#41636=CARTESIAN_POINT('Ctrl Pts',(-0.00199556615574467,-0.0376736638126523,
-0.0106694356219295));
#41637=CARTESIAN_POINT('Ctrl Pts',(-0.00194972728444761,-0.0376689130109799,
-0.0106106778723023));
#41638=CARTESIAN_POINT('Ctrl Pts',(-0.00192775500652634,-0.0376667170987196,
-0.0105836939397391));
#41639=CARTESIAN_POINT('Ctrl Pts',(-0.00187603710986693,-0.0376617246778843,
-0.0105228206022559));
#41640=CARTESIAN_POINT('Ctrl Pts',(-0.00184592333688678,-0.0376589435342649,
-0.0104892591725747));
#41641=CARTESIAN_POINT('Ctrl Pts',(-0.0016826449216898,-0.0376444655533574,
-0.0103169026617696));
#41642=CARTESIAN_POINT('Ctrl Pts',(-0.00153470487112565,-0.0376334272681061,
-0.0101930074092318));
#41643=CARTESIAN_POINT('Ctrl Pts',(-0.00131297605128778,-0.0376179279783162,
-0.0100471372151987));
#41644=CARTESIAN_POINT('Ctrl Pts',(-0.00125020949291117,-0.0376136330159059,
-0.0100096784792033));
#41645=CARTESIAN_POINT('Ctrl Pts',(-0.00114371618836145,-0.0376063544853546,
-0.00995229553907206));
#41646=CARTESIAN_POINT('Ctrl Pts',(-0.00110089385966737,-0.0376034296172707,
-0.00993078583470947));
#41647=CARTESIAN_POINT('Ctrl Pts',(-0.00103653257121679,-0.0375989984507089,
-0.00990074124558544));
#41648=CARTESIAN_POINT('Ctrl Pts',(-0.00101544832222549,-0.0375975413772552,
-0.00989125284397109));
#41649=CARTESIAN_POINT('Ctrl Pts',(-0.000975826893932983,-0.0375947876648727,
-0.00987407908875711));
#41650=CARTESIAN_POINT('Ctrl Pts',(-0.000957323491036033,-0.0375934949928333,
-0.00986632212002606));
#41651=CARTESIAN_POINT('Ctrl Pts',(-0.000909212325078636,-0.0375901194626916,
-0.00984683048040391));
#41652=CARTESIAN_POINT('Ctrl Pts',(-0.000879470681621455,-0.0375880190717043,
-0.00983543764281324));
#41653=CARTESIAN_POINT('Ctrl Pts',(-0.000718505933719115,-0.0375766078509464,
-0.00977727975102571));
#41654=CARTESIAN_POINT('Ctrl Pts',(-0.000583772210240915,-0.0375669164424697,
-0.00974097940270314));
#41655=CARTESIAN_POINT('Ctrl Pts',(-0.000345762855775532,-0.0375501781106134,
-0.00969775359825071));
#41656=CARTESIAN_POINT('Ctrl Pts',(-0.000243758648160511,-0.0375431187611106,
-0.00968564955050368));
#41657=CARTESIAN_POINT('Ctrl Pts',(-6.99317160158425E-5,-0.0375313921284449,
-0.0096758096358315));
#41658=CARTESIAN_POINT('Ctrl Pts',(1.57452670687609E-6,-0.0375266530757697,
-0.00967483193645387));
#41659=CARTESIAN_POINT('Ctrl Pts',(0.000111785748213136,-0.0375194810481381,
-0.00967805280963605));
#41660=CARTESIAN_POINT('Ctrl Pts',(0.000150511321571955,-0.0375169858909543,
-0.00968008689398806));
#41661=CARTESIAN_POINT('Ctrl Pts',(0.000224075758914965,-0.0375122896015905,
-0.0096856695418937));
#41662=CARTESIAN_POINT('Ctrl Pts',(0.000258917622393482,-0.0375100840063717,
-0.0096890507441003));
#41663=CARTESIAN_POINT('Ctrl Pts',(0.000341129780876372,-0.0375049179300782,
-0.00969877565138785));
#41664=CARTESIAN_POINT('Ctrl Pts',(0.000388412563168479,-0.0375019770558065,
-0.00970574817488102));
#41665=CARTESIAN_POINT('Ctrl Pts',(0.000629568223582207,-0.0374870849273301,
-0.00974840662841968));
#41666=CARTESIAN_POINT('Ctrl Pts',(0.000818921324996043,-0.037475814987661,
-0.0098055737602736));
#41667=CARTESIAN_POINT('Ctrl Pts',(0.00106085895570087,-0.0374603642066134,
-0.00991111379467665));
#41668=CARTESIAN_POINT('Ctrl Pts',(0.00112101794069365,-0.0374564206572916,
-0.00994028076458841));
#41669=CARTESIAN_POINT('Ctrl Pts',(0.00121984533105607,-0.0374496586916192,
-0.00999318818389156));
#41670=CARTESIAN_POINT('Ctrl Pts',(0.00125916764197979,-0.0374468887744168,
-0.0100156343406633));
#41671=CARTESIAN_POINT('Ctrl Pts',(0.00131723694949441,-0.0374426449026767,
-0.0100509059909875));
#41672=CARTESIAN_POINT('Ctrl Pts',(0.00133645575220129,-0.0374412142612031,
-0.0100629405755851));
#41673=CARTESIAN_POINT('Ctrl Pts',(0.0013725243257484,-0.0374384743380744,
-0.0100862152481735));
#41674=CARTESIAN_POINT('Ctrl Pts',(0.00138940593267399,-0.0374371681873588,
-0.0100974016509193));
#41675=CARTESIAN_POINT('Ctrl Pts',(0.00143346693514852,-0.0374336994114188,
-0.0101273747846713));
#41676=CARTESIAN_POINT('Ctrl Pts',(0.00146041249060754,-0.0374315173641894,
-0.010146497047843));
#41677=CARTESIAN_POINT('Ctrl Pts',(0.00158743526547992,-0.0374209657718817,
-0.0102404804182953));
#41678=CARTESIAN_POINT('Ctrl Pts',(0.00168217860577192,-0.0374122994590536,
-0.0103222379662543));
#41679=CARTESIAN_POINT('Ctrl Pts',(0.00184808696327729,-0.0373960295382161,
-0.0104886427016876));
#41680=CARTESIAN_POINT('Ctrl Pts',(0.00192054560524107,-0.0373884391069072,
-0.0105716049076001));
#41681=CARTESIAN_POINT('Ctrl Pts',(0.00203242463859123,-0.0373759954816367,
-0.0107181906946309));
#41682=CARTESIAN_POINT('Ctrl Pts',(0.00207488578225504,-0.0373710568226065,
-0.0107792929077976));
#41683=CARTESIAN_POINT('Ctrl Pts',(0.00213548411650259,-0.0373636609840927,
-0.010875374279836));
#41684=CARTESIAN_POINT('Ctrl Pts',(0.00215562283752787,-0.0373611350396869,
-0.0109090350207436));
#41685=CARTESIAN_POINT('Ctrl Pts',(0.00219216590290643,-0.0373564140130751,
-0.0109735114061478));
#41686=CARTESIAN_POINT('Ctrl Pts',(0.00220873293498352,-0.0373542137050769,
-0.0110042235002551));
#41687=CARTESIAN_POINT('Ctrl Pts',(0.00224601787164922,-0.0373491099814727,
-0.0110769461870895));
#41688=CARTESIAN_POINT('Ctrl Pts',(0.00226620921720971,-0.0373462247054723,
-0.0111192127150631));
#41689=CARTESIAN_POINT('Ctrl Pts',(0.00235932290368399,-0.0373322458693659,
-0.0113290937475608));
#41690=CARTESIAN_POINT('Ctrl Pts',(0.0024148994130645,-0.0373217284070465,
-0.0115037873353278));
#41691=CARTESIAN_POINT('Ctrl Pts',(0.00246612169864635,-0.0373065731665948,
-0.0117585075669225));
#41692=CARTESIAN_POINT('Ctrl Pts',(0.00247780866819228,-0.0373020549170756,
-0.0118346838080897));
#41693=CARTESIAN_POINT('Ctrl Pts',(0.00249120017015691,-0.0372944525908288,
-0.0119605087079745));
#41694=CARTESIAN_POINT('Ctrl Pts',(0.00249497607041573,-0.0372914341066806,
-0.0120098855005812));
#41695=CARTESIAN_POINT('Ctrl Pts',(0.00249837305303083,-0.0372868901336898,
-0.0120826935118889));
#41696=CARTESIAN_POINT('Ctrl Pts',(0.00249913499473276,-0.0372854176070781,
-0.0121060618950372));
#41697=CARTESIAN_POINT('Ctrl Pts',(0.00249985636577821,-0.0372829413351572,
-0.0121449081098642));
#41698=CARTESIAN_POINT('Ctrl Pts',(0.00250000000000597,-0.0372819472956257,
-0.0121603809209419));
#41699=CARTESIAN_POINT('Ctrl Pts',(0.0025,-0.0372809459012698,-0.0121758532875225));
#41700=CARTESIAN_POINT('Ctrl Pts',(0.0025,-0.0371551761478877,-0.0121758532865581));
#41701=CARTESIAN_POINT('Ctrl Pts',(0.0025,-0.0371588732405284,-0.012121273544903));
#41702=CARTESIAN_POINT('Ctrl Pts',(0.00249821262887724,-0.0371625322456442,
-0.0120666817557802));
#41703=CARTESIAN_POINT('Ctrl Pts',(0.00249137523274373,-0.037169436287764,
-0.0119624781081467));
#41704=CARTESIAN_POINT('Ctrl Pts',(0.00248663097685343,-0.0371726865236799,
-0.0119128961385677));
#41705=CARTESIAN_POINT('Ctrl Pts',(0.00247600682716946,-0.0371781608138532,
-0.0118285331595566));
#41706=CARTESIAN_POINT('Ctrl Pts',(0.00247086659556786,-0.0371804063271866,
-0.0117936759115406));
#41707=CARTESIAN_POINT('Ctrl Pts',(0.00245866842605222,-0.0371850225114768,
-0.0117215549224501));
#41708=CARTESIAN_POINT('Ctrl Pts',(0.00245149592927497,-0.0371873890689005,
-0.0116843195856719));
#41709=CARTESIAN_POINT('Ctrl Pts',(0.00242945596982218,-0.0371938287839682,
-0.0115824374803436));
#41710=CARTESIAN_POINT('Ctrl Pts',(0.00241285834255083,-0.0371978489164038,
-0.0115181950912784));
#41711=CARTESIAN_POINT('Ctrl Pts',(0.00236758877508944,-0.0372072274110915,
-0.0113679349943336));
#41712=CARTESIAN_POINT('Ctrl Pts',(0.00233675583325947,-0.0372125286275146,
-0.0112826668131943));
#41713=CARTESIAN_POINT('Ctrl Pts',(0.00223673439751916,-0.0372274419122276,
-0.0110469649549369));
#41714=CARTESIAN_POINT('Ctrl Pts',(0.00215715865973339,-0.0372369465789953,
-0.0109014816815006));
#41715=CARTESIAN_POINT('Ctrl Pts',(0.00204737012559697,-0.0372489283153428,
-0.0107408882967017));
#41716=CARTESIAN_POINT('Ctrl Pts',(0.00203050791415675,-0.0372507437279206,
-0.0107171256237146));
#41717=CARTESIAN_POINT('Ctrl Pts',(0.00200144354890014,-0.0372538419051825,
-0.0106776479317048));
#41718=CARTESIAN_POINT('Ctrl Pts',(0.00198946244084735,-0.0372551109401504,
-0.0106617744480759));
#41719=CARTESIAN_POINT('Ctrl Pts',(0.00196228652425008,-0.0372579737976691,
-0.0106266493113335));
#41720=CARTESIAN_POINT('Ctrl Pts',(0.00194699665243246,-0.0372595733141312,
-0.0106074766462316));
#41721=CARTESIAN_POINT('Ctrl Pts',(0.00189505636386408,-0.0372649617863302,
-0.0105442764724628));
#41722=CARTESIAN_POINT('Ctrl Pts',(0.00185717700575608,-0.0372688187012443,
-0.010501286445035));
#41723=CARTESIAN_POINT('Ctrl Pts',(0.001749942780224,-0.0372794653861836,
-0.0103877012494666));
#41724=CARTESIAN_POINT('Ctrl Pts',(0.00167781950046844,-0.0372863362539561,
-0.0103198608063866));
#41725=CARTESIAN_POINT('Ctrl Pts',(0.00149230024038699,-0.0373030559236669,
-0.0101650307748533));
#41726=CARTESIAN_POINT('Ctrl Pts',(0.00137509013877611,-0.0373128341623391,
-0.0100831268389333));
#41727=CARTESIAN_POINT('Ctrl Pts',(0.00120842556643995,-0.0373255623895726,
-0.00998674718971798));
#41728=CARTESIAN_POINT('Ctrl Pts',(0.00116459711126692,-0.0373288114824042,
-0.00996311923557821));
#41729=CARTESIAN_POINT('Ctrl Pts',(0.00108859657512858,-0.0373342844840245,
-0.00992503156688167));
#41730=CARTESIAN_POINT('Ctrl Pts',(0.00105677214308859,-0.0373365298255882,
-0.009909915565667));
#41731=CARTESIAN_POINT('Ctrl Pts',(0.000990049413701822,-0.037341146182647,
-0.00987993516253935));
#41732=CARTESIAN_POINT('Ctrl Pts',(0.00095511085249052,-0.037343513073693,
-0.00986518209169217));
#41733=CARTESIAN_POINT('Ctrl Pts',(0.000858146316598404,-0.0373499552354603,
-0.00982681344070009));
#41734=CARTESIAN_POINT('Ctrl Pts',(0.000795493137252516,-0.0373539774073863,
-0.00980486298231614));
#41735=CARTESIAN_POINT('Ctrl Pts',(0.000645332135951805,-0.0373633624180702,
-0.00975887808433417));
#41736=CARTESIAN_POINT('Ctrl Pts',(0.000557243831091014,-0.0373686679862518,
-0.00973706191922827));
#41737=CARTESIAN_POINT('Ctrl Pts',(0.0003058305787371,-0.0373835749319994,
-0.00968913321034425));
#41738=CARTESIAN_POINT('Ctrl Pts',(0.000140850642591267,-0.0373930696817843,
-0.00967436231927322));
#41739=CARTESIAN_POINT('Ctrl Pts',(-5.35128056789639E-5,-0.0374050410017591,
-0.0096762560079129));
#41740=CARTESIAN_POINT('Ctrl Pts',(-8.26605479173067E-5,-0.0374068576632098,
-0.00967705012508711));
#41741=CARTESIAN_POINT('Ctrl Pts',(-0.000131657307400051,-0.0374099572288557,
-0.0096792431841545));
#41742=CARTESIAN_POINT('Ctrl Pts',(-0.000151515075138346,-0.0374112263696641,
-0.00968036960596051));
#41743=CARTESIAN_POINT('Ctrl Pts',(-0.000195810511243041,-0.0374140884700735,
-0.009683412922291));
#41744=CARTESIAN_POINT('Ctrl Pts',(-0.000220235451106661,-0.0374156871018454,
-0.00968545232238211));
#41745=CARTESIAN_POINT('Ctrl Pts',(-0.00030154221504298,-0.0374210684326458,
-0.00969344656263809));
#41746=CARTESIAN_POINT('Ctrl Pts',(-0.000358246224784456,-0.0374249188587891,
-0.00970099379323162));
#41747=CARTESIAN_POINT('Ctrl Pts',(-0.000511910111394329,-0.0374355387061347,
-0.00972683762022137));
#41748=CARTESIAN_POINT('Ctrl Pts',(-0.000608126794533348,-0.0374423888299507,
-0.00974893952325825));
#41749=CARTESIAN_POINT('Ctrl Pts',(-0.000840134536559872,-0.0374591171587561,
-0.00981690052360707));
#41750=CARTESIAN_POINT('Ctrl Pts',(-0.000973793184968563,-0.0374689245539323,
-0.0098688594032971));
#41751=CARTESIAN_POINT('Ctrl Pts',(-0.00114696659032597,-0.0374816802645159,
-0.00995392934498782));
#41752=CARTESIAN_POINT('Ctrl Pts',(-0.00119098612857973,-0.0374849297068421,
-0.00997721030457246));
#41753=CARTESIAN_POINT('Ctrl Pts',(-0.00126491818064556,-0.0374904030981148,
-0.0100191838732753));
#41754=CARTESIAN_POINT('Ctrl Pts',(-0.00129518282739628,-0.0374926484880039,
-0.0100372222744937));
#41755=CARTESIAN_POINT('Ctrl Pts',(-0.00135721070225358,-0.037497264779268,
-0.0100759921392308));
#41756=CARTESIAN_POINT('Ctrl Pts',(-0.00138890387081183,-0.0374996315596356,
-0.0100968188944574));
#41757=CARTESIAN_POINT('Ctrl Pts',(-0.00147471503162175,-0.0375060729337506,
-0.0101560470139788));
#41758=CARTESIAN_POINT('Ctrl Pts',(-0.0015277986500562,-0.0375100944520712,
-0.0101958951698862));
#41759=CARTESIAN_POINT('Ctrl Pts',(-0.00164951409426047,-0.0375194773767364,
-0.010295076470449));
#41760=CARTESIAN_POINT('Ctrl Pts',(-0.00171662663218259,-0.037524781552225,
-0.0103561245948884));
#41761=CARTESIAN_POINT('Ctrl Pts',(-0.00189633812871021,-0.0375396905317433,
-0.0105384070426369));
#41762=CARTESIAN_POINT('Ctrl Pts',(-0.00200042249383268,-0.037549188460147,
-0.0106673357310069));
#41763=CARTESIAN_POINT('Ctrl Pts',(-0.00210698912535109,-0.0375611631192572,
-0.0108299533617198));
#41764=CARTESIAN_POINT('Ctrl Pts',(-0.00212253870069934,-0.0375629793783563,
-0.0108546117960118));
#41765=CARTESIAN_POINT('Ctrl Pts',(-0.00214796639526064,-0.0375660784922145,
-0.0108965425406685));
#41766=CARTESIAN_POINT('Ctrl Pts',(-0.00215807566547284,-0.0375673475942844,
-0.0109136706492718));
#41767=CARTESIAN_POINT('Ctrl Pts',(-0.00218018720661165,-0.0375702099177524,
-0.0109521765882714));
#41768=CARTESIAN_POINT('Ctrl Pts',(-0.00219208047716474,-0.0375718088180809,
-0.0109736120503907));
#41769=CARTESIAN_POINT('Ctrl Pts',(-0.00223067845967603,-0.0375771923407254,
-0.0110456551904282));
#41770=CARTESIAN_POINT('Ctrl Pts',(-0.00225595930751256,-0.0375810447619402,
-0.0110970016992436));
#41771=CARTESIAN_POINT('Ctrl Pts',(-0.00232000004147967,-0.0375916728465572,
-0.0112391851563366));
#41772=CARTESIAN_POINT('Ctrl Pts',(-0.00235517620199612,-0.0375985293346023,
-0.011331524349454));
#41773=CARTESIAN_POINT('Ctrl Pts',(-0.00242770784773348,-0.0376152551268038,
-0.011562107981696));
#41774=CARTESIAN_POINT('Ctrl Pts',(-0.00245883847305205,-0.0376250536931657,
-0.0117019632134072));
#41775=CARTESIAN_POINT('Ctrl Pts',(-0.0024844539093545,-0.0376378010957612,
-0.0118930689186244));
#41776=CARTESIAN_POINT('Ctrl Pts',(-0.00248959253759177,-0.0376410504460935,
-0.0119425985279008));
#41777=CARTESIAN_POINT('Ctrl Pts',(-0.00249583606199858,-0.0376465237319185,
-0.0120273834302457));
#41778=CARTESIAN_POINT('Ctrl Pts',(-0.00249768041747382,-0.0376487691063079,
-0.0120625674577943));
#41779=CARTESIAN_POINT('Ctrl Pts',(-0.00249996476438387,-0.0376533854055685,
-0.0121356794760301));
#41780=CARTESIAN_POINT('Ctrl Pts',(-0.00250028656929416,-0.0376557522086132,
-0.0121736022524783));
#41781=CARTESIAN_POINT('Ctrl Pts',(-0.00249879901690386,-0.0376621937606823,
-0.0122778612191967));
#41782=CARTESIAN_POINT('Ctrl Pts',(-0.00249521179670208,-0.0376662154288805,
-0.0123441425926648));
#41783=CARTESIAN_POINT('Ctrl Pts',(-0.00248049282331027,-0.0376755988406322,
-0.01250046781423));
#41784=CARTESIAN_POINT('Ctrl Pts',(-0.00246709036810547,-0.0376809033440191,
-0.0125902029941435));
#41785=CARTESIAN_POINT('Ctrl Pts',(-0.00241557344638587,-0.0376958118014755,
-0.0128409311664561));
#41786=CARTESIAN_POINT('Ctrl Pts',(-0.00236633209262211,-0.037705308941086,
-0.0129991290369363));
#41787=CARTESIAN_POINT('Ctrl Pts',(-0.00229047759703111,-0.0377172827691985,
-0.0131781318190623));
#41788=CARTESIAN_POINT('Ctrl Pts',(-0.00227863488235069,-0.037719099127798,
-0.0132047715449294));
#41789=CARTESIAN_POINT('Ctrl Pts',(-0.00225793313474505,-0.0377221983630126,
-0.013249228147586));
#41790=CARTESIAN_POINT('Ctrl Pts',(-0.00224932255905463,-0.0377234674845901,
-0.0132671569228806));
#41791=CARTESIAN_POINT('Ctrl Pts',(-0.00222962310064065,-0.037726329802467,
-0.0133069508639312));
#41792=CARTESIAN_POINT('Ctrl Pts',(-0.00221842571023967,-0.0377279286766415,
-0.013328757514631));
#41793=CARTESIAN_POINT('Ctrl Pts',(-0.00218002910643096,-0.0377333118849348,
-0.0134009029738061));
#41794=CARTESIAN_POINT('Ctrl Pts',(-0.00215142413475836,-0.037737164005625,
-0.0134504696411301));
#41795=CARTESIAN_POINT('Ctrl Pts',(-0.00206890023058864,-0.0377477908518304,
-0.0135827635858914));
#41796=CARTESIAN_POINT('Ctrl Pts',(-0.00201174051928373,-0.0377546463812288,
-0.0136633490866566));
#41797=CARTESIAN_POINT('Ctrl Pts',(-0.00186047090774206,-0.037771372260567,
-0.0138518905558524));
#41798=CARTESIAN_POINT('Ctrl Pts',(-0.00176155656163934,-0.0377811718663155,
-0.0139555670708428));
#41799=CARTESIAN_POINT('Ctrl Pts',(-0.0016169827052835,-0.037793920248975,
-0.0140831668877494));
#41800=CARTESIAN_POINT('Ctrl Pts',(-0.00157868121342839,-0.0377971696079862,
-0.0141149882555724));
#41801=CARTESIAN_POINT('Ctrl Pts',(-0.00151169640836178,-0.0378026429266149,
-0.0141673388985111));
#41802=CARTESIAN_POINT('Ctrl Pts',(-0.0014834836402625,-0.0378048883246053,
-0.0141884430269106));
#41803=CARTESIAN_POINT('Ctrl Pts',(-0.00142399634368329,-0.0378095046931221,
-0.0142310107568261));
#41804=CARTESIAN_POINT('Ctrl Pts',(-0.00139266039688508,-0.0378118715413125,
-0.014252373228893));
#41805=CARTESIAN_POINT('Ctrl Pts',(-0.00130518957296975,-0.0378183132913902,
-0.0143091330755973));
#41806=CARTESIAN_POINT('Ctrl Pts',(-0.00124811122153282,-0.0378223351080318,
-0.0143430223879998));
#41807=CARTESIAN_POINT('Ctrl Pts',(-0.00111000843383108,-0.0378317189635866,
-0.0144177501259986));
#41808=CARTESIAN_POINT('Ctrl Pts',(-0.00102797727352534,-0.0378370237548111,
-0.0144565295488911));
#41809=CARTESIAN_POINT('Ctrl Pts',(-0.000790966835365474,-0.0378519318671046,
-0.014553181938555));
#41810=CARTESIAN_POINT('Ctrl Pts',(-0.000632122048189224,-0.0378614284208444,
-0.0146002560265273));
#41811=CARTESIAN_POINT('Ctrl Pts',(-0.000441183559959953,-0.0378734016368977,
-0.0146367894959463));
#41812=CARTESIAN_POINT('Ctrl Pts',(-0.000412456695076201,-0.0378752180785833,
-0.0146417667613537));
#41813=CARTESIAN_POINT('Ctrl Pts',(-0.000363995871075622,-0.0378783173992866,
-0.0146492927219344));
#41814=CARTESIAN_POINT('Ctrl Pts',(-0.000344307135439707,-0.0378795865208704,
-0.0146521101793716));
#41815=CARTESIAN_POINT('Ctrl Pts',(-0.000300281363758517,-0.0378824487445634,
-0.0146578750295461));
#41816=CARTESIAN_POINT('Ctrl Pts',(-0.000275932602387833,-0.0378840475224937,
-0.014660699744501));
#41817=CARTESIAN_POINT('Ctrl Pts',(-0.000194630029985185,-0.0378894300960542,
-0.0146689220522243));
#41818=CARTESIAN_POINT('Ctrl Pts',(-0.000137535960343696,-0.0378932816601816,
-0.0146727224454632));
#41819=CARTESIAN_POINT('Ctrl Pts',(1.82732687588285E-5,-0.0379039062317722,
-0.0146777337676203));
#41820=CARTESIAN_POINT('Ctrl Pts',(0.000117011318379751,-0.0379107600123903,
-0.0146750625860317));
#41821=CARTESIAN_POINT('Ctrl Pts',(0.000357848769779478,-0.037927486805768,
-0.0146542414179252));
#41822=CARTESIAN_POINT('Ctrl Pts',(0.000499063720456591,-0.0379372890505839,
-0.0146297091561706));
#41823=CARTESIAN_POINT('Ctrl Pts',(0.000685556045182069,-0.0379500398856968,
-0.0145805343784468));
#41824=CARTESIAN_POINT('Ctrl Pts',(0.00073330532711476,-0.037953289248627,
-0.0145664059634975));
#41825=CARTESIAN_POINT('Ctrl Pts',(0.000814069223045794,-0.0379587625282782,
-0.0145398609487416));
#41826=CARTESIAN_POINT('Ctrl Pts',(0.000847299816321274,-0.0379610078847682,
-0.01452815516945));
#41827=CARTESIAN_POINT('Ctrl Pts',(0.000915762129038186,-0.0379656241217229,
-0.0145023995310569));
#41828=CARTESIAN_POINT('Ctrl Pts',(0.000950943986517909,-0.0379679908809522,
-0.0144882424140195));
#41829=CARTESIAN_POINT('Ctrl Pts',(0.00104676196183467,-0.037974432223804,
-0.0144471285193998));
#41830=CARTESIAN_POINT('Ctrl Pts',(0.00110666981507643,-0.0379784537312753,
-0.0144185491562909));
#41831=CARTESIAN_POINT('Ctrl Pts',(0.00124557577588733,-0.0379878366347455,
-0.0143453599483277));
#41832=CARTESIAN_POINT('Ctrl Pts',(0.00132342322323941,-0.0379931407991109,
-0.0142987688448356));
#41833=CARTESIAN_POINT('Ctrl Pts',(0.00153559641294985,-0.0380080498299906,
-0.0141555685708384));
#41834=CARTESIAN_POINT('Ctrl Pts',(0.0016630947242035,-0.0380175478155954,
-0.0140497347548168));
#41835=CARTESIAN_POINT('Ctrl Pts',(0.00179967944347598,-0.0380295225377554,
-0.0139113657945893));
#41836=CARTESIAN_POINT('Ctrl Pts',(0.0018197924881693,-0.0380313387782911,
-0.0138902642335271));
#41837=CARTESIAN_POINT('Ctrl Pts',(0.00185300006796865,-0.0380344378507581,
-0.0138541817268452));
#41838=CARTESIAN_POINT('Ctrl Pts',(0.00186629272081414,-0.0380357069297858,
-0.0138393877928635));
#41839=CARTESIAN_POINT('Ctrl Pts',(0.00189557267062487,-0.0380385691689307,
-0.0138060082244455));
#41840=CARTESIAN_POINT('Ctrl Pts',(0.00191146451086293,-0.0380401680071973,
-0.0137873445789218));
#41841=CARTESIAN_POINT('Ctrl Pts',(0.00196352683298741,-0.0380455511408569,
-0.0137243480187127));
#41842=CARTESIAN_POINT('Ctrl Pts',(0.00199844765754735,-0.038049403225228,
-0.0136790098110857));
#41843=CARTESIAN_POINT('Ctrl Pts',(0.00208929641697335,-0.0380600298762508,
-0.0135522924201939));
#41844=CARTESIAN_POINT('Ctrl Pts',(0.00214200921302042,-0.038066885250019,
-0.0134687336581958));
#41845=CARTESIAN_POINT('Ctrl Pts',(0.00225866424320271,-0.0380836121429279,
-0.0132570069458657));
#41846=CARTESIAN_POINT('Ctrl Pts',(0.00231681612679142,-0.0380934129021212,
-0.0131260270516478));
#41847=CARTESIAN_POINT('Ctrl Pts',(0.00237967813600566,-0.038106162407578,
-0.0129437141366519));
#41848=CARTESIAN_POINT('Ctrl Pts',(0.00239449724357181,-0.0381094118230363,
-0.012896173927572));
#41849=CARTESIAN_POINT('Ctrl Pts',(0.00241736182664375,-0.0381148851699031,
-0.0128142910200956));
#41850=CARTESIAN_POINT('Ctrl Pts',(0.00242611817960691,-0.0381171305421612,
-0.0127801642324504));
#41851=CARTESIAN_POINT('Ctrl Pts',(0.00244279591400892,-0.0381217467913269,
-0.0127089441033296));
#41852=CARTESIAN_POINT('Ctrl Pts',(0.00245060043938598,-0.0381241135474091,
-0.0126718325405866));
#41853=CARTESIAN_POINT('Ctrl Pts',(0.00246973111666688,-0.0381305548329474,
-0.0125693375517378));
#41854=CARTESIAN_POINT('Ctrl Pts',(0.00247930384723672,-0.0381345762890585,
-0.0125036568012529));
#41855=CARTESIAN_POINT('Ctrl Pts',(0.00249541115062034,-0.0381437677413351,
-0.0123506985764858));
#41856=CARTESIAN_POINT('Ctrl Pts',(0.00249999999997759,-0.0381488885800515,
-0.0122633067332957));
#41857=CARTESIAN_POINT('Ctrl Pts',(0.0025,-0.0381539840246788,-0.0121758532871986));
#41858=CARTESIAN_POINT('Origin',(0.,-0.0397787743898723,-0.0121758532865581));
#41859=CARTESIAN_POINT('',(0.0025,-0.0410787743898723,-0.0121758532865581));
#41860=CARTESIAN_POINT('Ctrl Pts',(0.0025,-0.0410787743898723,-0.0121758532865581));
#41861=CARTESIAN_POINT('Ctrl Pts',(0.0025,-0.0410787743898723,-0.0128288629739675));
#41862=CARTESIAN_POINT('Ctrl Pts',(0.00222759672557515,-0.0410787754263847,
-0.0134795746236003));
#41863=CARTESIAN_POINT('Ctrl Pts',(0.00170270298531027,-0.0410787748338191,
-0.01401101416509));
#41864=CARTESIAN_POINT('Ctrl Pts',(0.00163307252212577,-0.0410787748546467,
-0.0140737931571262));
#41865=CARTESIAN_POINT('Ctrl Pts',(0.00112277204735936,-0.0410787754415589,
-0.0144808811151188));
#41866=CARTESIAN_POINT('Ctrl Pts',(0.000559471036736449,-0.0410787782045595,
-0.0146719896977074));
#41867=CARTESIAN_POINT('Ctrl Pts',(-0.000187047541110501,-0.0410787758560658,
-0.0146778823060338));
#41868=CARTESIAN_POINT('Ctrl Pts',(-0.000374485721687926,-0.0410787757252281,
-0.014658497162392));
#41869=CARTESIAN_POINT('Ctrl Pts',(-0.00101199045659152,-0.041078775974969,
-0.014513111446229));
#41870=CARTESIAN_POINT('Ctrl Pts',(-0.00143610269325865,-0.0410787774094811,
-0.0142704576596842));
#41871=CARTESIAN_POINT('Ctrl Pts',(-0.00196496964495242,-0.0410787753961375,
-0.0137449744512443));
#41872=CARTESIAN_POINT('Ctrl Pts',(-0.00213246263452953,-0.0410787751295836,
-0.0135142982090746));
#41873=CARTESIAN_POINT('Ctrl Pts',(-0.00241637084585988,-0.0410787750762288,
-0.0129245209925911));
#41874=CARTESIAN_POINT('Ctrl Pts',(-0.00249713293482234,-0.0410787754775941,
-0.0125483842109252));
#41875=CARTESIAN_POINT('Ctrl Pts',(-0.00249776121147513,-0.0410787759848237,
-0.0118033367512004));
#41876=CARTESIAN_POINT('Ctrl Pts',(-0.00241756107791694,-0.0410787755114441,
-0.0114267889635422));
#41877=CARTESIAN_POINT('Ctrl Pts',(-0.00213348624334714,-0.0410787752677254,
-0.0108367968316592));
#41878=CARTESIAN_POINT('Ctrl Pts',(-0.00196556467943907,-0.0410787753518017,
-0.0106062063041865));
#41879=CARTESIAN_POINT('Ctrl Pts',(-0.00143571657760741,-0.0410787772765541,
-0.0100815865218018));
#41880=CARTESIAN_POINT('Ctrl Pts',(-0.00101147589656772,-0.0410787759052714,
-0.00984010203688117));
#41881=CARTESIAN_POINT('Ctrl Pts',(-0.00037429365328496,-0.041078774977993,
-0.00969482154357104));
#41882=CARTESIAN_POINT('Ctrl Pts',(-0.000186977209885448,-0.0410787748267238,
-0.00967530739438422));
#41883=CARTESIAN_POINT('Ctrl Pts',(0.000559246821395463,-0.0410787755265359,
-0.00968032969550766));
#41884=CARTESIAN_POINT('Ctrl Pts',(0.00112319433023955,-0.0410787747030648,
-0.00987028964463931));
#41885=CARTESIAN_POINT('Ctrl Pts',(0.00163370320205056,-0.0410787748872101,
-0.010277362013647));
#41886=CARTESIAN_POINT('Ctrl Pts',(0.00170331323667582,-0.0410787749410509,
-0.0103401241140352));
#41887=CARTESIAN_POINT('Ctrl Pts',(0.00222825340530501,-0.0410787756766175,
-0.0108717944914544));
#41888=CARTESIAN_POINT('Ctrl Pts',(0.0025,-0.0410787743898723,-0.0115228435991487));
#41889=CARTESIAN_POINT('Ctrl Pts',(0.0025,-0.0410787743898723,-0.0121758532865581));
#41890=CARTESIAN_POINT('',(0.00250000000001,-0.0397787743898823,-0.0121758532865581));
#41891=CARTESIAN_POINT('',(0.0025,-0.0397787743898723,-0.0121758532865581));
#41892=CARTESIAN_POINT('',(-0.0025,-0.0397787743898723,-0.0121758532865581));
#41893=CARTESIAN_POINT('Origin',(0.,-0.0397787743898823,-0.0121758532865581));
#41894=CARTESIAN_POINT('',(0.00249999934544701,-0.0392787743898823,-0.0121740442081995));
#41895=CARTESIAN_POINT('Ctrl Pts',(-0.0025,-0.0397787743898823,-0.0121758532865575));
#41896=CARTESIAN_POINT('Ctrl Pts',(-0.00249999999999988,-0.0397478427471941,
-0.0116900920949362));
#41897=CARTESIAN_POINT('Ctrl Pts',(-0.00235413749876254,-0.0397169111045061,
-0.0112043658373873));
#41898=CARTESIAN_POINT('Ctrl Pts',(-0.00208674577744029,-0.039685979461818,
-0.010799084584003));
#41899=CARTESIAN_POINT('Ctrl Pts',(-0.00199394577425234,-0.0396752444378394,
-0.0106584291388004));
#41900=CARTESIAN_POINT('Ctrl Pts',(-0.0018869550846095,-0.0396645094138609,
-0.0105273175393106));
#41901=CARTESIAN_POINT('Ctrl Pts',(-0.00176808672695887,-0.0396537743898823,
-0.0104084061654391));
#41902=CARTESIAN_POINT('Ctrl Pts',(-0.00143189695686255,-0.0396234130278288,
-0.010072094734594));
#41903=CARTESIAN_POINT('Ctrl Pts',(-0.000995398673130767,-0.0395930516657754,
-0.00983346644714466));
#41904=CARTESIAN_POINT('Ctrl Pts',(-0.000529138176708866,-0.0395626903037219,
-0.00973249232469651));
#41905=CARTESIAN_POINT('Ctrl Pts',(-0.000355522219299805,-0.0395513849991087,
-0.00969489377393592));
#41906=CARTESIAN_POINT('Ctrl Pts',(-0.000178043485081894,-0.0395400796944955,
-0.00967591754185142));
#41907=CARTESIAN_POINT('Ctrl Pts',(-9.04539238496386E-7,-0.0395287743898823,
-0.00967585345019635));
#41908=CARTESIAN_POINT('Ctrl Pts',(0.000474817243811614,-0.0394984130278289,
-0.00967568132657733));
#41909=CARTESIAN_POINT('Ctrl Pts',(0.000952258454684218,-0.0394680516657754,
-0.00981561710386961));
#41910=CARTESIAN_POINT('Ctrl Pts',(0.00135331081152122,-0.0394376903037219,
-0.0100738185943088));
#41911=CARTESIAN_POINT('Ctrl Pts',(0.00150264597810249,-0.0394263849991087,
-0.0101699620576968));
#41912=CARTESIAN_POINT('Ctrl Pts',(0.00164153365230363,-0.0394150796944955,
-0.010281989457779));
#41913=CARTESIAN_POINT('Ctrl Pts',(0.00176680728390159,-0.0394037743898823,
-0.0104071271852207));
#41914=CARTESIAN_POINT('Ctrl Pts',(0.00210955958854106,-0.0393728427471942,
-0.0107495076521303));
#41915=CARTESIAN_POINT('Ctrl Pts',(0.00235052058641601,-0.0393419111045061,
-0.0111953350141756));
#41916=CARTESIAN_POINT('Ctrl Pts',(0.00244859938587972,-0.039310979461818,
-0.0116715110937272));
#41917=CARTESIAN_POINT('Ctrl Pts',(0.00248263825910249,-0.0393002444378395,
-0.0118367710407515));
#41918=CARTESIAN_POINT('Ctrl Pts',(0.00249987735095609,-0.0392895094138609,
-0.0120054577310056));
#41919=CARTESIAN_POINT('Ctrl Pts',(0.00249999934544701,-0.0392787743898823,
-0.0121740442081995));
#41920=CARTESIAN_POINT('',(0.0025,-0.0391527785395309,-0.0121758533085357));
#41921=CARTESIAN_POINT('',(0.0025,-0.0397787743898723,-0.0121758532865581));
#41922=CARTESIAN_POINT('',(-0.00175719004339858,-0.0397787743898823,-0.0139541342405783));
#41923=CARTESIAN_POINT('Ctrl Pts',(0.0025,-0.0391527785410365,-0.0121758533086393));
#41924=CARTESIAN_POINT('Ctrl Pts',(0.00250000000061648,-0.039157582660636,
-0.0121060562114304));
#41925=CARTESIAN_POINT('Ctrl Pts',(0.00249707701919054,-0.0391624234467435,
-0.0120362772125198));
#41926=CARTESIAN_POINT('Ctrl Pts',(0.00247960951818523,-0.0391768568469155,
-0.011828220973911));
#41927=CARTESIAN_POINT('Ctrl Pts',(0.002456456148426,-0.0391863646039281,
-0.0116909370520127));
#41928=CARTESIAN_POINT('Ctrl Pts',(0.002409695504752,-0.0391988343180563,
-0.0115081439464148));
#41929=CARTESIAN_POINT('Ctrl Pts',(0.00239595042780696,-0.0392020761857502,
-0.011460388200149));
#41930=CARTESIAN_POINT('Ctrl Pts',(0.00237002275056489,-0.0392075459337757,
-0.0113794629250897));
#41931=CARTESIAN_POINT('Ctrl Pts',(0.00235854421671177,-0.039209794925704,
-0.0113460853524034));
#41932=CARTESIAN_POINT('Ctrl Pts',(0.00233320281379181,-0.0392144275131173,
-0.0112771774626844));
#41933=CARTESIAN_POINT('Ctrl Pts',(0.0023192259424744,-0.039216806785421,
-0.0112416986552508));
#41934=CARTESIAN_POINT('Ctrl Pts',(0.00227839175432255,-0.0392233114884375,
-0.011144618391072));
#41935=CARTESIAN_POINT('Ctrl Pts',(0.00224985360101651,-0.0392273822427032,
-0.0110837570181563));
#41936=CARTESIAN_POINT('Ctrl Pts',(0.00217632142479415,-0.0392369158138843,
-0.0109420926119364));
#41937=CARTESIAN_POINT('Ctrl Pts',(0.00212922984753439,-0.0392423186708913,
-0.0108624904440866));
#41938=CARTESIAN_POINT('Ctrl Pts',(0.00198798533245351,-0.0392571089857904,
-0.0106513784799449));
#41939=CARTESIAN_POINT('Ctrl Pts',(0.00188533583113448,-0.0392664049750631,
-0.0105261243297593));
#41940=CARTESIAN_POINT('Ctrl Pts',(0.00175044921612559,-0.0392781688516613,
-0.0103906911892844));
#41941=CARTESIAN_POINT('Ctrl Pts',(0.00172919128789605,-0.0392800118854489,
-0.0103700920938546));
#41942=CARTESIAN_POINT('Ctrl Pts',(0.00169304079938588,-0.0392831383282574,
-0.0103362857389185));
#41943=CARTESIAN_POINT('Ctrl Pts',(0.00167834749159793,-0.0392844071890178,
-0.0103228703984346));
#41944=CARTESIAN_POINT('Ctrl Pts',(0.00164555616250351,-0.0392872375810382,
-0.010293641188445));
#41945=CARTESIAN_POINT('Ctrl Pts',(0.00162738882544127,-0.0392888041220506,
-0.0102779115138656));
#41946=CARTESIAN_POINT('Ctrl Pts',(0.00156726690162972,-0.0392939753712362,
-0.0102273545174884));
#41947=CARTESIAN_POINT('Ctrl Pts',(0.00152440145952903,-0.0392976419304811,
-0.0101936392959742));
#41948=CARTESIAN_POINT('Ctrl Pts',(0.00140738385367027,-0.0393075288652982,
-0.0101076420849578));
#41949=CARTESIAN_POINT('Ctrl Pts',(0.00133142975461876,-0.0393138201152119,
-0.0100579485359475));
#41950=CARTESIAN_POINT('Ctrl Pts',(0.00111758497766121,-0.0393309440465368,
-0.00993409667149849));
#41951=CARTESIAN_POINT('Ctrl Pts',(0.000975146505137239,-0.0393417046139173,
-0.00986856683695444));
#41952=CARTESIAN_POINT('Ctrl Pts',(0.000780868114425284,-0.0393553150878084,
-0.00980041918618019));
#41953=CARTESIAN_POINT('Ctrl Pts',(0.000733758235032195,-0.0393585404214021,
-0.0097854471325298));
#41954=CARTESIAN_POINT('Ctrl Pts',(0.000652590928776104,-0.0393639742761535,
-0.00976227729419006));
#41955=CARTESIAN_POINT('Ctrl Pts',(0.000618750022325753,-0.039366204060264,
-0.00975338087215502));
#41956=CARTESIAN_POINT('Ctrl Pts',(0.000548145929854338,-0.0393707865604291,
-0.00973639595912972));
#41957=CARTESIAN_POINT('Ctrl Pts',(0.000511364294928023,-0.0393731352315771,
-0.009728421407159));
#41958=CARTESIAN_POINT('Ctrl Pts',(0.000409976828297761,-0.0393795142486738,
-0.00970882543898236));
#41959=CARTESIAN_POINT('Ctrl Pts',(0.000345069813037825,-0.0393834925148775,
-0.00969891258161475));
#41960=CARTESIAN_POINT('Ctrl Pts',(0.000191138965591627,-0.0393927497783937,
-0.00968157297597101));
#41961=CARTESIAN_POINT('Ctrl Pts',(0.000101959255066238,-0.0393979733445863,
-0.00967633853530567));
#41962=CARTESIAN_POINT('Ctrl Pts',(-0.00014852370566438,-0.039412557863015,
-0.00967506733469505));
#41963=CARTESIAN_POINT('Ctrl Pts',(-0.000309417849968945,-0.0394218125435577,
-0.00968984467637572));
#41964=CARTESIAN_POINT('Ctrl Pts',(-0.000499477094730154,-0.0394336652202432,
-0.00972604394515474));
#41965=CARTESIAN_POINT('Ctrl Pts',(-0.000531083223092435,-0.0394356683107231,
-0.00973270090407705));
#41966=CARTESIAN_POINT('Ctrl Pts',(-0.000582085813717356,-0.0394389657075573,
-0.00974447957669038));
#41967=CARTESIAN_POINT('Ctrl Pts',(-0.000601566286691135,-0.0394402407870793,
-0.00974922599894935));
#41968=CARTESIAN_POINT('Ctrl Pts',(-0.000643057067412867,-0.0394429934231556,
-0.00975986555950009));
#41969=CARTESIAN_POINT('Ctrl Pts',(-0.000665047190610122,-0.0394444741367174,
-0.00976582605996293));
#41970=CARTESIAN_POINT('Ctrl Pts',(-0.000731128519181098,-0.039448983630436,
-0.00978471086953718));
#41971=CARTESIAN_POINT('Ctrl Pts',(-0.000774945934629837,-0.0394520547474661,
-0.00979855036092699));
#41972=CARTESIAN_POINT('Ctrl Pts',(-0.000882895035253787,-0.0394597845898461,
-0.00983594691946712));
#41973=CARTESIAN_POINT('Ctrl Pts',(-0.000946489559851482,-0.03946448478577,
-0.00986094031605689));
#41974=CARTESIAN_POINT('Ctrl Pts',(-0.00118754901785606,-0.0394827049763967,
-0.0099672746063182));
#41975=CARTESIAN_POINT('Ctrl Pts',(-0.00135631330578544,-0.0394962618798542,
-0.0100666995735911));
#41976=CARTESIAN_POINT('Ctrl Pts',(-0.00155044208003037,-0.0395123546487842,
-0.0102140981798258));
#41977=CARTESIAN_POINT('Ctrl Pts',(-0.0015882212972613,-0.0395155177431289,
-0.0102445564757565));
#41978=CARTESIAN_POINT('Ctrl Pts',(-0.00165182610085897,-0.03952090229862,
-0.0102989653830152));
#41979=CARTESIAN_POINT('Ctrl Pts',(-0.00167807518874211,-0.0395231430151491,
-0.0103223966430386));
#41980=CARTESIAN_POINT('Ctrl Pts',(-0.00173210405914562,-0.0395277992113981,
-0.0103727145876207));
#41981=CARTESIAN_POINT('Ctrl Pts',(-0.00175977257632255,-0.0395302095095703,
-0.0103997073555977));
#41982=CARTESIAN_POINT('Ctrl Pts',(-0.00183593877314693,-0.0395369308692806,
-0.0104775412168436));
#41983=CARTESIAN_POINT('Ctrl Pts',(-0.00188293669064766,-0.0395411808870754,
-0.0105298017389423));
#41984=CARTESIAN_POINT('Ctrl Pts',(-0.0019911769682663,-0.0395513192102645,
-0.0106608746375088));
#41985=CARTESIAN_POINT('Ctrl Pts',(-0.00205002389018882,-0.0395571354131304,
-0.0107415069289753));
#41986=CARTESIAN_POINT('Ctrl Pts',(-0.00218152261675665,-0.0395713160882073,
-0.0109463776956109));
#41987=CARTESIAN_POINT('Ctrl Pts',(-0.00224856694586445,-0.0395796423988666,
-0.0110737692938842));
#41988=CARTESIAN_POINT('Ctrl Pts',(-0.00231654710161025,-0.0395903992507804,
-0.0112353174285732));
#41989=CARTESIAN_POINT('Ctrl Pts',(-0.00232824743724487,-0.0395923615412376,
-0.0112646662379435));
#41990=CARTESIAN_POINT('Ctrl Pts',(-0.00234661026791289,-0.0395956447079986,
-0.0113133918707819));
#41991=CARTESIAN_POINT('Ctrl Pts',(-0.00235359620816925,-0.0395969484893898,
-0.0113326425769288));
#41992=CARTESIAN_POINT('Ctrl Pts',(-0.00236837108914986,-0.0395998323509752,
-0.0113749715857738));
#41993=CARTESIAN_POINT('Ctrl Pts',(-0.00237606016619275,-0.0396014169637098,
-0.011398080121452));
#41994=CARTESIAN_POINT('Ctrl Pts',(-0.00239958952059697,-0.0396065380962115,
-0.0114724020050694));
#41995=CARTESIAN_POINT('Ctrl Pts',(-0.00241411993927983,-0.0396101312131657,
-0.0115240115177225));
#41996=CARTESIAN_POINT('Ctrl Pts',(-0.00244811160213753,-0.039619739318698,
-0.011661550405884));
#41997=CARTESIAN_POINT('Ctrl Pts',(-0.00246470954775051,-0.0396258172288196,
-0.0117481107294897));
#41998=CARTESIAN_POINT('Ctrl Pts',(-0.00249739404152034,-0.0396423625611843,
-0.011985855689533));
#41999=CARTESIAN_POINT('Ctrl Pts',(-0.00250432617195534,-0.0396527653776538,
-0.012137938927484));
#42000=CARTESIAN_POINT('Ctrl Pts',(-0.0024951616966148,-0.0396660382162044,
-0.0123389309042198));
#42001=CARTESIAN_POINT('Ctrl Pts',(-0.00249146429441867,-0.039669247594065,
-0.0123880616758106));
#42002=CARTESIAN_POINT('Ctrl Pts',(-0.0024825925406336,-0.0396747068144292,
-0.0124725101522114));
#42003=CARTESIAN_POINT('Ctrl Pts',(-0.0024781095303846,-0.0396769762231178,
-0.0125078839745554));
#42004=CARTESIAN_POINT('Ctrl Pts',(-0.00246710611757726,-0.0396816966597413,
-0.0125819655751408));
#42005=CARTESIAN_POINT('Ctrl Pts',(-0.0024604277244359,-0.0396841423026736,
-0.0126206402665768));
#42006=CARTESIAN_POINT('Ctrl Pts',(-0.00243895887099843,-0.0396909914559501,
-0.0127296010944704));
#42007=CARTESIAN_POINT('Ctrl Pts',(-0.00242204630631484,-0.0396953310741771,
-0.0127994316595031));
#42008=CARTESIAN_POINT('Ctrl Pts',(-0.00237375112622782,-0.0397057137609527,
-0.0129669369278575));
#42009=CARTESIAN_POINT('Ctrl Pts',(-0.00233932099393189,-0.039711679882097,
-0.0130635956338083));
#42010=CARTESIAN_POINT('Ctrl Pts',(-0.00224325251832436,-0.0397259061316189,
-0.0132885067680261));
#42011=CARTESIAN_POINT('Ctrl Pts',(-0.00217642517413692,-0.0397341336360773,
-0.0134141361583159));
#42012=CARTESIAN_POINT('Ctrl Pts',(-0.00208213379415691,-0.0397447853638204,
-0.0135599481538735));
#42013=CARTESIAN_POINT('Ctrl Pts',(-0.00206446305273776,-0.0397467484546398,
-0.0135861695037583));
#42014=CARTESIAN_POINT('Ctrl Pts',(-0.00203588021800161,-0.0397498848631493,
-0.013626894556479));
#42015=CARTESIAN_POINT('Ctrl Pts',(-0.0020252987736522,-0.0397510380483964,
-0.0136416274365659));
#42016=CARTESIAN_POINT('Ctrl Pts',(-0.00200222590653047,-0.0397535388409107,
-0.0136730256730993));
#42017=CARTESIAN_POINT('Ctrl Pts',(-0.00198968521731073,-0.0397548901755503,
-0.0136896519358763));
#42018=CARTESIAN_POINT('Ctrl Pts',(-0.00196306243452417,-0.0397577396944162,
-0.0137240457234404));
#42019=CARTESIAN_POINT('Ctrl Pts',(-0.00194894313828253,-0.0397592401013026,
-0.0137417825646316));
#42020=CARTESIAN_POINT('Ctrl Pts',(-0.00187891197293792,-0.0397666201559316,
-0.0138273422379145));
#42021=CARTESIAN_POINT('Ctrl Pts',(-0.00181970175645458,-0.0397726701680068,
-0.0138923639339491));
#42022=CARTESIAN_POINT('Ctrl Pts',(-0.00175719004339085,-0.0397787743898682,
-0.0139541342405719));
#42023=CARTESIAN_POINT('Origin',(0.,-0.0397787743898823,-0.0121758532865581));
#42024=CARTESIAN_POINT('Ctrl Pts',(0.00190999122146646,-0.0443987860946598,
-0.0121758532865581));
#42025=CARTESIAN_POINT('Ctrl Pts',(0.00190999122146646,-0.0443987860946598,
-0.0116043852298449));
#42026=CARTESIAN_POINT('Ctrl Pts',(0.00136395817994342,-0.0443987860946598,
-0.0104664540336249));
#42027=CARTESIAN_POINT('Ctrl Pts',(-0.000486152278277537,-0.0443987860946598,
-0.0100448265867138));
#42028=CARTESIAN_POINT('Ctrl Pts',(-0.00197136065961974,-0.0443987860946598,
-0.011227004012724));
#42029=CARTESIAN_POINT('Ctrl Pts',(-0.00196862385650474,-0.0443987860946598,
-0.0131236069817994));
#42030=CARTESIAN_POINT('Ctrl Pts',(-0.000487368329395306,-0.0443987860946598,
-0.0143095653443973));
#42031=CARTESIAN_POINT('Ctrl Pts',(0.00136371609385951,-0.0443987860946598,
-0.0138834237073105));
#42032=CARTESIAN_POINT('Ctrl Pts',(0.00190999122146646,-0.0443987860946598,
-0.0127473213432713));
#42033=CARTESIAN_POINT('Ctrl Pts',(0.00190999122146646,-0.0443987860946598,
-0.0121758532865581));
#42034=CARTESIAN_POINT('Ctrl Pts',(0.00192589049556924,-0.0443775867868491,
-0.0121758532865581));
#42035=CARTESIAN_POINT('Ctrl Pts',(0.00192589049556924,-0.0443775867868491,
-0.0115996636724157));
#42036=CARTESIAN_POINT('Ctrl Pts',(0.00137529606726147,-0.0443775867868491,
-0.0104522153996155));
#42037=CARTESIAN_POINT('Ctrl Pts',(-0.00049019777087024,-0.0443775867868491,
-0.0100270982797518));
#42038=CARTESIAN_POINT('Ctrl Pts',(-0.00198775342676737,-0.0443775867868491,
-0.0112191060568122));
#42039=CARTESIAN_POINT('Ctrl Pts',(-0.00198501288010718,-0.0443775867868491,
-0.0131315025932785));
#42040=CARTESIAN_POINT('Ctrl Pts',(-0.000491416389901987,-0.0443775867868491,
-0.0143272981564294));
#42041=CARTESIAN_POINT('Ctrl Pts',(0.00137505627975056,-0.0443775867868491,
-0.0138976586778796));
#42042=CARTESIAN_POINT('Ctrl Pts',(0.00192589049556924,-0.0443775867868491,
-0.0127520429007005));
#42043=CARTESIAN_POINT('Ctrl Pts',(0.00192589049556924,-0.0443775867868491,
-0.0121758532865581));
#42044=CARTESIAN_POINT('Ctrl Pts',(0.00195438435881241,-0.0443409038628781,
-0.0121758532865581));
#42045=CARTESIAN_POINT('Ctrl Pts',(0.00195438435881241,-0.0443409038628781,
-0.0115910933812226));
#42046=CARTESIAN_POINT('Ctrl Pts',(0.00139566437443473,-0.0443409038628781,
-0.0104267256068493));
#42047=CARTESIAN_POINT('Ctrl Pts',(-0.000497452079284101,-0.0443409038628781,
-0.00999529310352459));
#42048=CARTESIAN_POINT('Ctrl Pts',(-0.00201718480527981,-0.0443409038628781,
-0.0112049501630331));
#42049=CARTESIAN_POINT('Ctrl Pts',(-0.00201437932167482,-0.044340903862878,
-0.0131456335630356));
#42050=CARTESIAN_POINT('Ctrl Pts',(-0.000498698406502515,-0.0443409038628781,
-0.0143591659955113));
#42051=CARTESIAN_POINT('Ctrl Pts',(0.00139541551284433,-0.044340903862878,
-0.0139231065486815));
#42052=CARTESIAN_POINT('Ctrl Pts',(0.00195438435881241,-0.0443409038628781,
-0.0127606131918936));
#42053=CARTESIAN_POINT('Ctrl Pts',(0.00195438435881241,-0.0443409038628781,
-0.0121758532865581));
#42054=CARTESIAN_POINT('Ctrl Pts',(0.00201714899795489,-0.0442974094567112,
-0.0121758532865581));
#42055=CARTESIAN_POINT('Ctrl Pts',(0.00201714899795489,-0.0442974094567112,
-0.0115723431648622));
#42056=CARTESIAN_POINT('Ctrl Pts',(0.00144047261468403,-0.0442974094567112,
-0.0103705452165039));
#42057=CARTESIAN_POINT('Ctrl Pts',(-0.000513426520915583,-0.0442974094567112,
-0.00992527387087597));
#42058=CARTESIAN_POINT('Ctrl Pts',(-0.00208195197224179,-0.0442974094567112,
-0.0111737702411527));
#42059=CARTESIAN_POINT('Ctrl Pts',(-0.00207907206613982,-0.0442974094567112,
-0.0131767830034219));
#42060=CARTESIAN_POINT('Ctrl Pts',(-0.000514706653486131,-0.0442974094567112,
-0.0144292589295152));
#42061=CARTESIAN_POINT('Ctrl Pts',(0.00144021931264795,-0.0442974094567112,
-0.0139792362605124));
#42062=CARTESIAN_POINT('Ctrl Pts',(0.00201714899795489,-0.0442974094567112,
-0.0127793634082539));
#42063=CARTESIAN_POINT('Ctrl Pts',(0.00201714899795489,-0.0442974094567112,
-0.0121758532865581));
#42064=CARTESIAN_POINT('Ctrl Pts',(0.00208710243564359,-0.0442779618954001,
-0.0121758532865581));
#42065=CARTESIAN_POINT('Ctrl Pts',(0.00208710243564359,-0.0442779618954001,
-0.0115513767164868));
#42066=CARTESIAN_POINT('Ctrl Pts',(0.00149044407485555,-0.0442779618954001,
-0.0103079478417784));
#42067=CARTESIAN_POINT('Ctrl Pts',(-0.000531233254498119,-0.0442779618954001,
-0.00984721379520205));
#42068=CARTESIAN_POINT('Ctrl Pts',(-0.00215417088504416,-0.0442779618954001,
-0.0111390181009185));
#42069=CARTESIAN_POINT('Ctrl Pts',(-0.00215117120441165,-0.0442779618954001,
-0.0132114880644132));
#42070=CARTESIAN_POINT('Ctrl Pts',(-0.00053256567848247,-0.0442779618954001,
-0.0145074356744791));
#42071=CARTESIAN_POINT('Ctrl Pts',(0.00149017747918706,-0.0442779618954001,
-0.0140417547899323));
#42072=CARTESIAN_POINT('Ctrl Pts',(0.00208710243564359,-0.0442779618954001,
-0.0128003298566294));
#42073=CARTESIAN_POINT('Ctrl Pts',(0.00208710243564359,-0.0442779618954001,
-0.0121758532865581));
#42074=CARTESIAN_POINT('Ctrl Pts',(0.00213645587150032,-0.0442788243925216,
-0.0121758532865581));
#42075=CARTESIAN_POINT('Ctrl Pts',(0.00213645587150032,-0.0442788243925216,
-0.0115366816146531));
#42076=CARTESIAN_POINT('Ctrl Pts',(0.00152565591062824,-0.0442788243925216,
-0.0102637592345077));
#42077=CARTESIAN_POINT('Ctrl Pts',(-0.00054379248925872,-0.0442788243925216,
-0.00979217086851526));
#42078=CARTESIAN_POINT('Ctrl Pts',(-0.002205075151519,-0.0442788243925216,
-0.0111145012429317));
#42079=CARTESIAN_POINT('Ctrl Pts',(-0.00220204305666343,-0.0442788243925216,
-0.013235990244785));
#42080=CARTESIAN_POINT('Ctrl Pts',(-0.000545141135798698,-0.0442788243925216,
-0.0145625120797918));
#42081=CARTESIAN_POINT('Ctrl Pts',(0.00152539173851854,-0.0442788243925216,
-0.0140859193992423));
#42082=CARTESIAN_POINT('Ctrl Pts',(0.00213645587150032,-0.0442788243925216,
-0.0128150249584631));
#42083=CARTESIAN_POINT('Ctrl Pts',(0.00213645587150032,-0.0442788243925216,
-0.0121758532865581));
#42084=CARTESIAN_POINT('Ctrl Pts',(0.00215952697976718,-0.0442787673768399,
-0.0121758532865581));
#42085=CARTESIAN_POINT('Ctrl Pts',(0.00215952697976718,-0.0442787673768399,
-0.0115296965823474));
#42086=CARTESIAN_POINT('Ctrl Pts',(0.00154216857972284,-0.0442787673768399,
-0.0102431322722294));
#42087=CARTESIAN_POINT('Ctrl Pts',(-0.000549667972357268,-0.0442787673768399,
-0.00976640454250539));
#42088=CARTESIAN_POINT('Ctrl Pts',(-0.00222892774721398,-0.0442787673768399,
-0.0111030387336221));
#42089=CARTESIAN_POINT('Ctrl Pts',(-0.00222581851868729,-0.0442787673768399,
-0.0132474238346592));
#42090=CARTESIAN_POINT('Ctrl Pts',(-0.000551048797835124,-0.0442787673768399,
-0.0145883521636443));
#42091=CARTESIAN_POINT('Ctrl Pts',(0.00154189149668708,-0.0442787673768399,
-0.0141064975077928));
#42092=CARTESIAN_POINT('Ctrl Pts',(0.00215952697976718,-0.0442787673768399,
-0.0128220099907686));
#42093=CARTESIAN_POINT('Ctrl Pts',(0.00215952697976718,-0.0442787673768399,
-0.0121758532865581));
#42094=CARTESIAN_POINT('',(0.00215000000001,-0.0442787743898723,-0.0121758532865581));
#42095=CARTESIAN_POINT('',(0.00191,-0.0443987743898723,-0.0121758532865581));
#42096=CARTESIAN_POINT('Ctrl Pts',(0.00215000000001,-0.0442787743898723,
-0.0121758532865581));
#42097=CARTESIAN_POINT('Ctrl Pts',(0.00213012938819229,-0.0442787743898723,
-0.0121758532865581));
#42098=CARTESIAN_POINT('Ctrl Pts',(0.00208390361990812,-0.0442788511892961,
-0.0121758532865581));
#42099=CARTESIAN_POINT('Ctrl Pts',(0.00201714899795489,-0.0442974094567112,
-0.0121758532865581));
#42100=CARTESIAN_POINT('Ctrl Pts',(0.00195438855983192,-0.0443409009516712,
-0.0121758532865581));
#42101=CARTESIAN_POINT('Ctrl Pts',(0.00192589648945146,-0.0443775790706037,
-0.0121758532865581));
#42102=CARTESIAN_POINT('Ctrl Pts',(0.00191,-0.0443987743898723,-0.0121758532865581));
#42103=CARTESIAN_POINT('',(-0.00215000000001046,-0.0442787744046664,-0.0121758532865581));
#42104=CARTESIAN_POINT('Origin',(0.,-0.0442787743898823,-0.0121758532865581));
#42105=CARTESIAN_POINT('',(-0.00190884695691278,-0.0443979099384254,-0.0121758531596464));
#42106=CARTESIAN_POINT('Ctrl Pts',(-0.00215000000001053,-0.0442787744120635,
-0.0121758532865581));
#42107=CARTESIAN_POINT('Ctrl Pts',(-0.00212945708742072,-0.0442787748951294,
-0.0121758575253048));
#42108=CARTESIAN_POINT('Ctrl Pts',(-0.00210900073339659,-0.0442787255022982,
-0.012175855287986));
#42109=CARTESIAN_POINT('Ctrl Pts',(-0.00208844214891447,-0.0442812121748871,
-0.0121758544076401));
#42110=CARTESIAN_POINT('Ctrl Pts',(-0.00206193243021586,-0.0442844186695213,
-0.0121758532724587));
#42111=CARTESIAN_POINT('Ctrl Pts',(-0.00203525272905052,-0.044291841976487,
-0.0121758543935678));
#42112=CARTESIAN_POINT('Ctrl Pts',(-0.00201079104512614,-0.0443040605875159,
-0.0121758543850288));
#42113=CARTESIAN_POINT('Ctrl Pts',(-0.00199244478218284,-0.0443132245457876,
-0.0121758543786247));
#42114=CARTESIAN_POINT('Ctrl Pts',(-0.00197534615393758,-0.0443250858625948,
-0.0121758537367935));
#42115=CARTESIAN_POINT('Ctrl Pts',(-0.0019603454088488,-0.0443386005552682,
-0.0121758540374385));
#42116=CARTESIAN_POINT('Ctrl Pts',(-0.00194061637249586,-0.0443563751298959,
-0.012175854432848));
#42117=CARTESIAN_POINT('Ctrl Pts',(-0.00192451617246681,-0.0443770096495027,
-0.0121758564585159));
#42118=CARTESIAN_POINT('Ctrl Pts',(-0.00190884695647826,-0.0443979099380992,
-0.0121758537542897));
#42119=CARTESIAN_POINT('Ctrl Pts',(0.00191,-0.0443987743898723,-0.0121758532865581));
#42120=CARTESIAN_POINT('Ctrl Pts',(0.00191,-0.0443987743898723,-0.0116769538853774));
#42121=CARTESIAN_POINT('Ctrl Pts',(0.00170286569430852,-0.0443979141034954,
-0.0111791984316711));
#42122=CARTESIAN_POINT('Ctrl Pts',(0.00130148688929984,-0.0443984059277294,
-0.0107730760513384));
#42123=CARTESIAN_POINT('Ctrl Pts',(0.00124824039806454,-0.0443984214812156,
-0.0107250730699049));
#42124=CARTESIAN_POINT('Ctrl Pts',(0.00085820319796886,-0.0443983102877573,
-0.0104139306476503));
#42125=CARTESIAN_POINT('Ctrl Pts',(0.000427365466200854,-0.0443970919325886,
-0.0102678966017304));
#42126=CARTESIAN_POINT('Ctrl Pts',(-0.000142889419619194,-0.0443981275956193,
-0.0102649171393808));
#42127=CARTESIAN_POINT('Ctrl Pts',(-0.000285989619838265,-0.0443981683922595,
-0.0102798769391036));
#42128=CARTESIAN_POINT('Ctrl Pts',(-0.000772950241023675,-0.0443979823563326,
-0.0103907749516927));
#42129=CARTESIAN_POINT('Ctrl Pts',(-0.00109761918967261,-0.0443972656261806,
-0.0105748535622802));
#42130=CARTESIAN_POINT('Ctrl Pts',(-0.00150220109501196,-0.0443982715496484,
-0.0109762745220466));
#42131=CARTESIAN_POINT('Ctrl Pts',(-0.00163050456530604,-0.0443983785168756,
-0.0111525082295191));
#42132=CARTESIAN_POINT('Ctrl Pts',(-0.00184765159456686,-0.0443983257609707,
-0.0116033854086035));
#42133=CARTESIAN_POINT('Ctrl Pts',(-0.00190905487174541,-0.0443980661033178,
-0.011891145752726));
#42134=CARTESIAN_POINT('Ctrl Pts',(-0.00190884695778182,-0.0443979099390777,
-0.0121758519703597));
#42135=CARTESIAN_POINT('Origin',(0.,-0.0397787743898723,-0.0121758532865581));
#42136=CARTESIAN_POINT('Ctrl Pts',(0.00249999935903926,-0.0392790584006181,
-0.0121740630901204));
#42137=CARTESIAN_POINT('Ctrl Pts',(0.00250007956807936,-0.0392713094448282,
-0.012286074568086));
#42138=CARTESIAN_POINT('Ctrl Pts',(0.00249263173726238,-0.0392635731967025,
-0.0123979738977816));
#42139=CARTESIAN_POINT('Ctrl Pts',(0.00246733605361282,-0.0392507422192454,
-0.0125861025581287));
#42140=CARTESIAN_POINT('Ctrl Pts',(0.00245337573639674,-0.0392455676519652,
-0.0126626809130144));
#42141=CARTESIAN_POINT('Ctrl Pts',(0.00242690245496861,-0.0392379021202853,
-0.0127772936630157));
#42142=CARTESIAN_POINT('Ctrl Pts',(0.00241701327554165,-0.0392353348903791,
-0.0128158791978145));
#42143=CARTESIAN_POINT('Ctrl Pts',(0.00239672010907757,-0.0392305673004155,
-0.0128878608886453));
#42144=CARTESIAN_POINT('Ctrl Pts',(0.00238652922805646,-0.0392283609778843,
-0.0129213065325673));
#42145=CARTESIAN_POINT('Ctrl Pts',(0.00236149140120812,-0.0392233368771582,
-0.0129976937533472));
#42146=CARTESIAN_POINT('Ctrl Pts',(0.00234616858500414,-0.039220534776043,
-0.0130404669269349));
#42147=CARTESIAN_POINT('Ctrl Pts',(0.00226003621061368,-0.0392060584453356,
-0.0132617162607692));
#42148=CARTESIAN_POINT('Ctrl Pts',(0.00217000806586963,-0.0391950378577499,
-0.0134320111981609));
#42149=CARTESIAN_POINT('Ctrl Pts',(0.00201939095886307,-0.0391795000751182,
-0.0136515108509263));
#42150=CARTESIAN_POINT('Ctrl Pts',(0.001974710770261,-0.0391751414655364,
-0.0137107869249371));
#42151=CARTESIAN_POINT('Ctrl Pts',(0.00189662176439386,-0.0391677668860012,
-0.0138053229027469));
#42152=CARTESIAN_POINT('Ctrl Pts',(0.00186470340147605,-0.0391648115905817,
-0.0138417542234014));
#42153=CARTESIAN_POINT('Ctrl Pts',(0.00181595056253204,-0.0391603430353711,
-0.0138942427919207));
#42154=CARTESIAN_POINT('Ctrl Pts',(0.00179991605181313,-0.0391588801778623,
-0.0139110308136084));
#42155=CARTESIAN_POINT('Ctrl Pts',(0.00176968858466169,-0.0391561294940817,
-0.0139418089392524));
#42156=CARTESIAN_POINT('Ctrl Pts',(0.00175555814557438,-0.0391548459258268,
-0.0139558568103638));
#42157=CARTESIAN_POINT('Ctrl Pts',(0.00171877666747503,-0.0391515130272924,
-0.0139915594081504));
#42158=CARTESIAN_POINT('Ctrl Pts',(0.00169588416679098,-0.0391494468417173,
-0.0140129593355787));
#42159=CARTESIAN_POINT('Ctrl Pts',(0.00156497778349947,-0.0391377063619642,
-0.0141307986675549));
#42160=CARTESIAN_POINT('Ctrl Pts',(0.00144915290219264,-0.0391276145863704,
-0.0142181357359344));
#42161=CARTESIAN_POINT('Ctrl Pts',(0.00124177240671048,-0.0391106849498419,
-0.0143479435805051));
#42162=CARTESIAN_POINT('Ctrl Pts',(0.0011540096266945,-0.0391038192518612,
-0.0143958171422466));
#42163=CARTESIAN_POINT('Ctrl Pts',(0.00100002238319515,-0.0390923647016948,
-0.0144682085245878));
#42164=CARTESIAN_POINT('Ctrl Pts',(0.000935196404764055,-0.0390877081392731,
-0.0144954106791712));
#42165=CARTESIAN_POINT('Ctrl Pts',(0.000833290456592871,-0.0390806405583546,
-0.0145332040180072));
#42166=CARTESIAN_POINT('Ctrl Pts',(0.000796971231267928,-0.0390781693712407,
-0.0145457293540501));
#42167=CARTESIAN_POINT('Ctrl Pts',(0.000727247850065306,-0.0390735116960162,
-0.0145679903896269));
#42168=CARTESIAN_POINT('Ctrl Pts',(0.000693901295168457,-0.0390713209172959,
-0.0145778754633805));
#42169=CARTESIAN_POINT('Ctrl Pts',(0.000614470762973968,-0.0390661832913899,
-0.0145996291119793));
#42170=CARTESIAN_POINT('Ctrl Pts',(0.000568232114567011,-0.0390632561072837,
-0.0146108843492146));
#42171=CARTESIAN_POINT('Ctrl Pts',(0.000327463267891536,-0.0390482919685742,
-0.0146622588559959));
#42172=CARTESIAN_POINT('Ctrl Pts',(0.000128987277406619,-0.0390369544908499,
-0.0146804112996346));
#42173=CARTESIAN_POINT('Ctrl Pts',(-0.00013624320578099,-0.0390214374052796,
-0.0146730294698443));
#42174=CARTESIAN_POINT('Ctrl Pts',(-0.000202829421000357,-0.039017503716378,
-0.0146685045567991));
#42175=CARTESIAN_POINT('Ctrl Pts',(-0.000314071396957006,-0.039010757905199,
-0.014656458185455));
#42176=CARTESIAN_POINT('Ctrl Pts',(-0.00035884877449846,-0.0390079946155222,
-0.0146503771852284));
#42177=CARTESIAN_POINT('Ctrl Pts',(-0.000425699956247967,-0.0390037646428949,
-0.0146394459046998));
#42178=CARTESIAN_POINT('Ctrl Pts',(-0.000447914917421691,-0.0390023415399719,
-0.0146355039081018));
#42179=CARTESIAN_POINT('Ctrl Pts',(-0.000489906582527642,-0.0389996132008413,
-0.0146274648684539));
#42180=CARTESIAN_POINT('Ctrl Pts',(-0.000509692497781764,-0.0389983110649594,
-0.014623427853502));
#42181=CARTESIAN_POINT('Ctrl Pts',(-0.000561475282717601,-0.0389948629593587,
-0.0146122072997597));
#42182=CARTESIAN_POINT('Ctrl Pts',(-0.000593382910862238,-0.0389926979182879,
-0.0146046331975596));
#42183=CARTESIAN_POINT('Ctrl Pts',(-0.000735342028510397,-0.0389829107024314,
-0.014567971345772));
#42184=CARTESIAN_POINT('Ctrl Pts',(-0.000843473076475308,-0.0389750425965237,
-0.0145320167176374));
#42185=CARTESIAN_POINT('Ctrl Pts',(-0.00105762428101284,-0.0389590156085835,
-0.0144441729213225));
#42186=CARTESIAN_POINT('Ctrl Pts',(-0.00116319844389065,-0.038950877181691,
-0.0143918894223511));
#42187=CARTESIAN_POINT('Ctrl Pts',(-0.00133129862955095,-0.038937704612051,
-0.0142933055960654));
#42188=CARTESIAN_POINT('Ctrl Pts',(-0.00139605428816112,-0.0389325699374373,
-0.0142511833078515));
#42189=CARTESIAN_POINT('Ctrl Pts',(-0.00149101437166873,-0.0389249507224814,
-0.0141829540249695));
#42190=CARTESIAN_POINT('Ctrl Pts',(-0.00152271138738355,-0.0389223909370783,
-0.0141590142857709));
#42191=CARTESIAN_POINT('Ctrl Pts',(-0.00158117969491548,-0.0389176335877468,
-0.01411262636824));
#42192=CARTESIAN_POINT('Ctrl Pts',(-0.00160807667283415,-0.0389154301516067,
-0.0140903529086273));
#42193=CARTESIAN_POINT('Ctrl Pts',(-0.00166889709263256,-0.0389104069701919,
-0.0140378009404544));
#42194=CARTESIAN_POINT('Ctrl Pts',(-0.00170247926496707,-0.0389076030008652,
-0.0140071455377505));
#42195=CARTESIAN_POINT('Ctrl Pts',(-0.00187108631641443,-0.0388933233397116,
-0.0138445837629436));
#42196=CARTESIAN_POINT('Ctrl Pts',(-0.00199169085157221,-0.038882473030154,
-0.0136986134107762));
#42197=CARTESIAN_POINT('Ctrl Pts',(-0.00213511309275719,-0.0388671234641056,
-0.0134784534504286));
#42198=CARTESIAN_POINT('Ctrl Pts',(-0.00217272740441468,-0.0388627738211867,
-0.0134146953108739));
#42199=CARTESIAN_POINT('Ctrl Pts',(-0.00223013028260811,-0.0388554158594305,
-0.0133067166945462));
#42200=CARTESIAN_POINT('Ctrl Pts',(-0.00225156137082834,-0.0388524674498998,
-0.0132634211630765));
#42201=CARTESIAN_POINT('Ctrl Pts',(-0.00228142560336189,-0.0388480046596076,
-0.0131984173716676));
#42202=CARTESIAN_POINT('Ctrl Pts',(-0.00229083226155805,-0.0388465401001722,
-0.0131771661984361));
#42203=CARTESIAN_POINT('Ctrl Pts',(-0.0023078237096158,-0.0388437758749244,
-0.0131372866748334));
#42204=CARTESIAN_POINT('Ctrl Pts',(-0.00231548232733165,-0.0388424802622809,
-0.013118692571443));
#42205=CARTESIAN_POINT('Ctrl Pts',(-0.00233471859492918,-0.0388390964265217,
-0.0130703411733368));
#42206=CARTESIAN_POINT('Ctrl Pts',(-0.00234595167654181,-0.0388369906162808,
-0.0130404514642194));
#42207=CARTESIAN_POINT('Ctrl Pts',(-0.00240238576789733,-0.0388257181768527,
-0.0128810835140073));
#42208=CARTESIAN_POINT('Ctrl Pts',(-0.00243744521600239,-0.0388161837378341,
-0.0127482718267893));
#42209=CARTESIAN_POINT('Ctrl Pts',(-0.00247958671686932,-0.0387995173401985,
-0.0125111304838851));
#42210=CARTESIAN_POINT('Ctrl Pts',(-0.00249136341631072,-0.0387923783133283,
-0.0124079575189453));
#42211=CARTESIAN_POINT('Ctrl Pts',(-0.00250039193627361,-0.0387805437321716,
-0.0122325258375608));
#42212=CARTESIAN_POINT('Ctrl Pts',(-0.00250098776779624,-0.0387757744929865,
-0.012160575966621));
#42213=CARTESIAN_POINT('Ctrl Pts',(-0.00249712592140333,-0.0387685681693809,
-0.0120498726853318));
#42214=CARTESIAN_POINT('Ctrl Pts',(-0.00249486692454081,-0.0387660679692394,
-0.0120110859425473));
#42215=CARTESIAN_POINT('Ctrl Pts',(-0.00248885666750585,-0.0387613670497003,
-0.0119374903312185));
#42216=CARTESIAN_POINT('Ctrl Pts',(-0.00248527653242043,-0.0387591617555307,
-0.0119026772268701));
#42217=CARTESIAN_POINT('Ctrl Pts',(-0.00247509808725708,-0.0387540039608111,
-0.0118206633971288));
#42218=CARTESIAN_POINT('Ctrl Pts',(-0.00246787867821289,-0.0387510708521218,
-0.0117735528149738));
#42219=CARTESIAN_POINT('Ctrl Pts',(-0.00242367290482959,-0.0387361070637379,
-0.0115315197676855));
#42220=CARTESIAN_POINT('Ctrl Pts',(-0.00236492917918075,-0.0387247693686716,
-0.01134130567534));
#42221=CARTESIAN_POINT('Ctrl Pts',(-0.00225728548916071,-0.0387092614922215,
-0.0110992439397178));
#42222=CARTESIAN_POINT('Ctrl Pts',(-0.00222784071222068,-0.0387053356308295,
-0.0110395653528206));
#42223=CARTESIAN_POINT('Ctrl Pts',(-0.002174480793844,-0.0386985995587368,
-0.0109414826011622));
#42224=CARTESIAN_POINT('Ctrl Pts',(-0.00215183984312562,-0.0386958373978953,
-0.0109024238744217));
#42225=CARTESIAN_POINT('Ctrl Pts',(-0.00211627130687492,-0.0386916032118865,
-0.0108447226817457));
#42226=CARTESIAN_POINT('Ctrl Pts',(-0.00210412606451918,-0.0386901742426793,
-0.0108256065135759));
#42227=CARTESIAN_POINT('Ctrl Pts',(-0.00208063853724313,-0.0386874367707865,
-0.0107897245336473));
#42228=CARTESIAN_POINT('Ctrl Pts',(-0.00206934935287574,-0.0386861313770795,
-0.0107729267776615));
#42229=CARTESIAN_POINT('Ctrl Pts',(-0.00203910020048041,-0.0386826636261566,
-0.010729076997341));
#42230=CARTESIAN_POINT('Ctrl Pts',(-0.00201980615791264,-0.0386804818293827,
-0.0107022610422355));
#42231=CARTESIAN_POINT('Ctrl Pts',(-0.00192376213987685,-0.0386697920474501,
-0.0105742045565931));
#42232=CARTESIAN_POINT('Ctrl Pts',(-0.00183990591172958,-0.0386609769460144,
-0.0104785373654807));
#42233=CARTESIAN_POINT('Ctrl Pts',(-0.00167145740923374,-0.0386446526449844,
-0.0103135818872248));
#42234=CARTESIAN_POINT('Ctrl Pts',(-0.00158887808078922,-0.0386371537149641,
-0.0102426449896635));
#42235=CARTESIAN_POINT('Ctrl Pts',(-0.00144288382669919,-0.038624833354164,
-0.0101329281848067));
#42236=CARTESIAN_POINT('Ctrl Pts',(-0.00138188907811333,-0.0386199287907678,
-0.0100911852048101));
#42237=CARTESIAN_POINT('Ctrl Pts',(-0.00128589870118461,-0.0386125726199831,
-0.0100315597127439));
#42238=CARTESIAN_POINT('Ctrl Pts',(-0.00125218619417094,-0.0386100532991229,
-0.0100116997773888));
#42239=CARTESIAN_POINT('Ctrl Pts',(-0.00118756728797422,-0.0386053402607332,
-0.00997564876379939));
#42240=CARTESIAN_POINT('Ctrl Pts',(-0.00115676144572518,-0.0386031414239712,
-0.00995929759045683));
#42241=CARTESIAN_POINT('Ctrl Pts',(-0.00108374322017955,-0.0385980350429165,
-0.00992247794073592));
#42242=CARTESIAN_POINT('Ctrl Pts',(-0.00104127628996369,-0.0385951457967156,
-0.0099025420612868));
#42243=CARTESIAN_POINT('Ctrl Pts',(-0.00083127565818442,-0.0385812032151748,
-0.00981107878006168));
#42244=CARTESIAN_POINT('Ctrl Pts',(-0.000656832093369744,-0.0385707213511682,
-0.00975681322273996));
#42245=CARTESIAN_POINT('Ctrl Pts',(-0.000402110777389722,-0.0385555872724883,
-0.0097071918123256));
#42246=CARTESIAN_POINT('Ctrl Pts',(-0.000325549435483613,-0.0385510517070664,
-0.00969593416847256));
#42247=CARTESIAN_POINT('Ctrl Pts',(-0.000199207069529726,-0.0385434246152464,
-0.00968330840647957));
#42248=CARTESIAN_POINT('Ctrl Pts',(-0.000149687379126713,-0.0385403993279406,
-0.00967984518520542));
#42249=CARTESIAN_POINT('Ctrl Pts',(-7.67321610441968E-5,-0.0385358478832761,
-0.00967692168347982));
#42250=CARTESIAN_POINT('Ctrl Pts',(-5.33523115760781E-5,-0.0385343750390019,
-0.00967631324554714));
#42251=CARTESIAN_POINT('Ctrl Pts',(-1.00075927420404E-5,-0.0385316124791532,
-0.00967579361941128));
#42252=CARTESIAN_POINT('Ctrl Pts',(9.95362974219692E-6,-0.0385303272352797,
-0.00967579342545424));
#42253=CARTESIAN_POINT('Ctrl Pts',(6.10757741388324E-5,-0.0385270047572596,
-0.00967640513049062));
#42254=CARTESIAN_POINT('Ctrl Pts',(9.22284759683785E-5,-0.0385249510554573,
-0.00967736073363271));
#42255=CARTESIAN_POINT('Ctrl Pts',(0.000270485429823215,-0.0385130625615317,
-0.00968616690447775));
#42256=CARTESIAN_POINT('Ctrl Pts',(0.000416677309051651,-0.0385027956845988,
-0.0097064251323653));
#42257=CARTESIAN_POINT('Ctrl Pts',(0.00065637852069251,-0.0384857874507535,
-0.00976154146567406));
#42258=CARTESIAN_POINT('Ctrl Pts',(0.000751145290130313,-0.0384790112117261,
-0.00978932489190344));
#42259=CARTESIAN_POINT('Ctrl Pts',(0.000909782464449212,-0.0384676725824359,
-0.00984622332900752));
#42260=CARTESIAN_POINT('Ctrl Pts',(0.000974524048473925,-0.0384630452925797,
-0.00987255473353534));
#42261=CARTESIAN_POINT('Ctrl Pts',(0.00107313182191805,-0.0384559984005605,
-0.00991756356609153));
#42262=CARTESIAN_POINT('Ctrl Pts',(0.00110780782329801,-0.0384535202176235,
-0.00993437019305436));
#42263=CARTESIAN_POINT('Ctrl Pts',(0.00117330084286178,-0.0384488355617415,
-0.00996800440018539));
#42264=CARTESIAN_POINT('Ctrl Pts',(0.00120417870502521,-0.0384466250862385,
-0.00998469254098601));
#42265=CARTESIAN_POINT('Ctrl Pts',(0.00127680679537846,-0.0384414152439737,
-0.0100259440369304));
#42266=CARTESIAN_POINT('Ctrl Pts',(0.00131821535169387,-0.0384384364649971,
-0.0100510817409769));
#42267=CARTESIAN_POINT('Ctrl Pts',(0.00152090322710265,-0.0384237633936469,
-0.0101823343308435));
#42268=CARTESIAN_POINT('Ctrl Pts',(0.00167023610750409,-0.0384127130086052,
-0.0103056715560944));
#42269=CARTESIAN_POINT('Ctrl Pts',(0.00185115424463824,-0.038397424953653,
-0.0104942209847853));
#42270=CARTESIAN_POINT('Ctrl Pts',(0.00189637391772476,-0.0383934006193565,
-0.0105453858095551));
#42271=CARTESIAN_POINT('Ctrl Pts',(0.00196839994031086,-0.038386519090943,
-0.0106339363435631));
#42272=CARTESIAN_POINT('Ctrl Pts',(0.0019963711735133,-0.0383837126128927,
-0.0106703275426845));
#42273=CARTESIAN_POINT('Ctrl Pts',(0.00203670928260101,-0.0383794239918355,
-0.0107259102872087));
#42274=CARTESIAN_POINT('Ctrl Pts',(0.00204984193175066,-0.0383779864810876,
-0.0107445366309428));
#42275=CARTESIAN_POINT('Ctrl Pts',(0.00207413791152825,-0.0383752423482606,
-0.0107800164468686));
#42276=CARTESIAN_POINT('Ctrl Pts',(0.00208535471644444,-0.0383739390558308,
-0.0107968303874377));
#42277=CARTESIAN_POINT('Ctrl Pts',(0.00211422121495514,-0.0383704910452267,
-0.0108412587094857));
#42278=CARTESIAN_POINT('Ctrl Pts',(0.00213153355996036,-0.038368327339692,
-0.0108690868658608));
#42279=CARTESIAN_POINT('Ctrl Pts',(0.0022045952139261,-0.0383587912707048,
-0.0109918437103385));
#42280=CARTESIAN_POINT('Ctrl Pts',(0.00225458365770268,-0.0383511896015644,
-0.0110900504934806));
#42281=CARTESIAN_POINT('Ctrl Pts',(0.00234516748123503,-0.0383352666144794,
-0.0113014554234975));
#42282=CARTESIAN_POINT('Ctrl Pts',(0.00238441064520533,-0.0383269647092676,
-0.0114149513149793));
#42283=CARTESIAN_POINT('Ctrl Pts',(0.00243545976366286,-0.0383135840237234,
-0.0116061105628277));
#42284=CARTESIAN_POINT('Ctrl Pts',(0.00245203421202549,-0.0383083996543626,
-0.0116822935060415));
#42285=CARTESIAN_POINT('Ctrl Pts',(0.00247164937571965,-0.0383007302028928,
-0.0117983229972484));
#42286=CARTESIAN_POINT('Ctrl Pts',(0.00247733933720076,-0.0382981678759811,
-0.0118376671647369));
#42287=CARTESIAN_POINT('Ctrl Pts',(0.00248624592811626,-0.0382934158938033,
-0.011911672479033));
#42288=CARTESIAN_POINT('Ctrl Pts',(0.00248968159609899,-0.0382912201389792,
-0.0119462970758275));
#42289=CARTESIAN_POINT('Ctrl Pts',(0.00249590484773491,-0.03828622995467,
-0.0120258927576418));
#42290=CARTESIAN_POINT('Ctrl Pts',(0.00249820182974504,-0.0382834508394078,
-0.0120708906060241));
#42291=CARTESIAN_POINT('Ctrl Pts',(0.00249976069722458,-0.0382794848074351,
-0.0121359058760536));
#42292=CARTESIAN_POINT('Ctrl Pts',(0.0025,-0.0382782729015159,-0.0121558823324649));
#42293=CARTESIAN_POINT('Ctrl Pts',(0.0025,-0.0382770671668707,-0.0121758532865581));
#42294=CARTESIAN_POINT('Ctrl Pts',(0.0025,-0.0381539840246788,-0.0121758532871986));
#42295=CARTESIAN_POINT('Ctrl Pts',(0.00250000000000082,-0.0381541705624727,
-0.0121726517269627));
#42296=CARTESIAN_POINT('Ctrl Pts',(0.00249999385000889,-0.0381543570699,
-0.0121694500843802));
#42297=CARTESIAN_POINT('Ctrl Pts',(0.00249934642527115,-0.0381641720104095,
-0.0120009373131903));
#42298=CARTESIAN_POINT('Ctrl Pts',(0.00248231629253901,-0.038173669900826,
-0.0118361168523468));
#42299=CARTESIAN_POINT('Ctrl Pts',(0.00244330343755171,-0.0381856445063766,
-0.01164564757488));
#42300=CARTESIAN_POINT('Ctrl Pts',(0.00243695525014424,-0.0381874607692292,
-0.0116171953198876));
#42301=CARTESIAN_POINT('Ctrl Pts',(0.00242544100492311,-0.0381905599441513,
-0.0115695269821681));
#42302=CARTESIAN_POINT('Ctrl Pts',(0.00242054054139413,-0.0381918291051899,
-0.0115502502884726));
#42303=CARTESIAN_POINT('Ctrl Pts',(0.00240908659999788,-0.0381946917181867,
-0.0115073453607196));
#42304=CARTESIAN_POINT('Ctrl Pts',(0.00240241509679818,-0.0381962908526318,
-0.0114837530869141));
#42305=CARTESIAN_POINT('Ctrl Pts',(0.00237901490065508,-0.0382016757004568,
-0.0114054221606092));
#42306=CARTESIAN_POINT('Ctrl Pts',(0.00236075440099767,-0.0382055292443022,
-0.0113511632280352));
#42307=CARTESIAN_POINT('Ctrl Pts',(0.00230594736017677,-0.0382161619865515,
-0.0112050987499869));
#42308=CARTESIAN_POINT('Ctrl Pts',(0.00226579512304355,-0.038223022064487,
-0.0111147552809035));
#42309=CARTESIAN_POINT('Ctrl Pts',(0.00215473521105433,-0.0382397446910621,
-0.0109001031759708));
#42310=CARTESIAN_POINT('Ctrl Pts',(0.00207829598423172,-0.0382495365701051,
-0.0107790291376534));
#42311=CARTESIAN_POINT('Ctrl Pts',(0.00196183752924849,-0.0382622776819215,
-0.0106254753901673));
#42312=CARTESIAN_POINT('Ctrl Pts',(0.00193057627244965,-0.0382655269415844,
-0.0105867170657871));
#42313=CARTESIAN_POINT('Ctrl Pts',(0.00187525049488516,-0.0382710002551838,
-0.0105221675060152));
#42314=CARTESIAN_POINT('Ctrl Pts',(0.00185176068022609,-0.0382732457418609,
-0.0104959057687032));
#42315=CARTESIAN_POINT('Ctrl Pts',(0.00180184870494172,-0.0382778624527694,
-0.010442423341932));
#42316=CARTESIAN_POINT('Ctrl Pts',(0.00177534627212186,-0.0382802295509761,
-0.0104152897460699));
#42317=CARTESIAN_POINT('Ctrl Pts',(0.00170079412703607,-0.0382866725179929,
-0.0103423582804202));
#42318=CARTESIAN_POINT('Ctrl Pts',(0.00165152093698755,-0.038290695272157,
-0.010297853219663));
#42319=CARTESIAN_POINT('Ctrl Pts',(0.00153085747719404,-0.0383000819879186,
-0.0101972928071582));
#42320=CARTESIAN_POINT('Ctrl Pts',(0.00145807226607399,-0.0383053886516684,
-0.0101430589585176));
#42321=CARTESIAN_POINT('Ctrl Pts',(0.00124484482363963,-0.0383202943420306,
-0.0100015356982766));
#42322=CARTESIAN_POINT('Ctrl Pts',(0.00109849071249593,-0.0383297869176337,
-0.00992405386014048));
#42323=CARTESIAN_POINT('Ctrl Pts',(0.000918590755929435,-0.0383417559683749,
-0.00985054867963535));
#42324=CARTESIAN_POINT('Ctrl Pts',(0.00089140450199058,-0.0383435729546521,
-0.00983999191742967));
#42325=CARTESIAN_POINT('Ctrl Pts',(0.000845375814920642,-0.0383466728590269,
-0.00982303893141305));
#42326=CARTESIAN_POINT('Ctrl Pts',(0.000826630905350146,-0.0383479420045997,
-0.0098163878867729));
#42327=CARTESIAN_POINT('Ctrl Pts',(0.000784617852132649,-0.0383508037453525,
-0.00980204299940726));
#42328=CARTESIAN_POINT('Ctrl Pts',(0.000761314061312069,-0.0383524020046748,
-0.00979446687441789));
#42329=CARTESIAN_POINT('Ctrl Pts',(0.000683289026682467,-0.0383577809641004,
-0.00977036299646431));
#42330=CARTESIAN_POINT('Ctrl Pts',(0.000628115623028511,-0.0383616293253011,
-0.00975537043930304));
#42331=CARTESIAN_POINT('Ctrl Pts',(0.000476552075874866,-0.0383722407912966,
-0.00971971611300622));
#42332=CARTESIAN_POINT('Ctrl Pts',(0.000379375206622141,-0.0383790844868964,
-0.00970284195134638));
#42333=CARTESIAN_POINT('Ctrl Pts',(0.000139112964132458,-0.0383958160809537,
-0.00967561926094437));
#42334=CARTESIAN_POINT('Ctrl Pts',(-4.37271060656557E-6,-0.0384056330848951,
-0.00967175399304792));
#42335=CARTESIAN_POINT('Ctrl Pts',(-0.000197110386961847,-0.0384183976563063,
-0.00968313874680747));
#42336=CARTESIAN_POINT('Ctrl Pts',(-0.000246709905085807,-0.0384216470531593,
-0.00968755807429891));
#42337=CARTESIAN_POINT('Ctrl Pts',(-0.00033112332366197,-0.0384271201885602,
-0.00969762850313059));
#42338=CARTESIAN_POINT('Ctrl Pts',(-0.000366008573806928,-0.0384293653731207,
-0.00970253999124724));
#42339=CARTESIAN_POINT('Ctrl Pts',(-0.000438200452295828,-0.038433981055254,
-0.00971426485574402));
#42340=CARTESIAN_POINT('Ctrl Pts',(-0.000475479414601754,-0.0384363474363587,
-0.00972119306509451));
#42341=CARTESIAN_POINT('Ctrl Pts',(-0.000577502517495833,-0.038442787034568,
-0.0097425654566891));
#42342=CARTESIAN_POINT('Ctrl Pts',(-0.000641853564258747,-0.0384468072145951,
-0.0097587426400268));
#42343=CARTESIAN_POINT('Ctrl Pts',(-0.000792413387206625,-0.038456186016707,
-0.00980302994649983));
#42344=CARTESIAN_POINT('Ctrl Pts',(-0.000877886642595209,-0.0384614874763449,
-0.00983330639311861));
#42345=CARTESIAN_POINT('Ctrl Pts',(-0.00111423740165229,-0.0384764005485237,
-0.00993178491872894));
#42346=CARTESIAN_POINT('Ctrl Pts',(-0.00126023318113975,-0.0384859047842912,
-0.010010404835257));
#42347=CARTESIAN_POINT('Ctrl Pts',(-0.00142153644882803,-0.038497886085101,
-0.0101191367193451));
#42348=CARTESIAN_POINT('Ctrl Pts',(-0.00144540839605377,-0.0384997014487062,
-0.0101358426708262));
#42349=CARTESIAN_POINT('Ctrl Pts',(-0.00148507293385394,-0.0385027994238487,
-0.0101646462237679));
#42350=CARTESIAN_POINT('Ctrl Pts',(-0.00150102255975954,-0.0385040683017685,
-0.0101765217204181));
#42351=CARTESIAN_POINT('Ctrl Pts',(-0.00153631714380791,-0.0385069305295438,
-0.0102034611765283));
#42352=CARTESIAN_POINT('Ctrl Pts',(-0.00155558383418402,-0.0385085295667161,
-0.0102186205902852));
#42353=CARTESIAN_POINT('Ctrl Pts',(-0.00161908492923169,-0.0385139147863003,
-0.0102701143981229));
#42354=CARTESIAN_POINT('Ctrl Pts',(-0.00166229164401142,-0.038517768838684,
-0.010307682463096));
#42355=CARTESIAN_POINT('Ctrl Pts',(-0.00177645234352948,-0.0385284033171046,
-0.0104140424140648));
#42356=CARTESIAN_POINT('Ctrl Pts',(-0.00184467929833496,-0.0385352646839569,
-0.0104856113857629));
#42357=CARTESIAN_POINT('Ctrl Pts',(-0.00200083375238739,-0.0385519928568928,
-0.0106701633155684));
#42358=CARTESIAN_POINT('Ctrl Pts',(-0.00208365614888532,-0.0385617889204118,
-0.0107870319204679));
#42359=CARTESIAN_POINT('Ctrl Pts',(-0.00218124216654747,-0.0385745342973122,
-0.0109532898898803));
#42360=CARTESIAN_POINT('Ctrl Pts',(-0.0022051569554232,-0.0385777839596734,
-0.010996971609131));
#42361=CARTESIAN_POINT('Ctrl Pts',(-0.00224373895101086,-0.0385832575811734,
-0.0110727320422425));
#42362=CARTESIAN_POINT('Ctrl Pts',(-0.0022590605830719,-0.0385855029874871,
-0.0111044586616928));
#42363=CARTESIAN_POINT('Ctrl Pts',(-0.00228947006757324,-0.0385901191693694,
-0.0111709829646241));
#42364=CARTESIAN_POINT('Ctrl Pts',(-0.00230444704965679,-0.0385924858270522,
-0.0112058215411856));
#42365=CARTESIAN_POINT('Ctrl Pts',(-0.00234343226594881,-0.0385989264635807,
-0.0113025116553677));
#42366=CARTESIAN_POINT('Ctrl Pts',(-0.00236578092009217,-0.0386029473906875,
-0.0113650005976482));
#42367=CARTESIAN_POINT('Ctrl Pts',(-0.00241272021049882,-0.0386123286768818,
-0.01151479666479));
#42368=CARTESIAN_POINT('Ctrl Pts',(-0.00243509935406213,-0.0386176318392299,
-0.0116026978687232));
#42369=CARTESIAN_POINT('Ctrl Pts',(-0.00248467829252718,-0.0386325407226579,
-0.0118538184627112));
#42370=CARTESIAN_POINT('Ctrl Pts',(-0.00250052883380926,-0.038642039492982,
-0.0120187702971199));
#42371=CARTESIAN_POINT('Ctrl Pts',(-0.00249989090737695,-0.0386540149464972,
-0.0122132049603197));
#42372=CARTESIAN_POINT('Ctrl Pts',(-0.00249928546707395,-0.0386558311273124,
-0.012242349006102));
#42373=CARTESIAN_POINT('Ctrl Pts',(-0.00249740964900756,-0.0386589305545246,
-0.0122913561495992));
#42374=CARTESIAN_POINT('Ctrl Pts',(-0.0024964114253466,-0.0386602000629332,
-0.0123112262134441));
#42375=CARTESIAN_POINT('Ctrl Pts',(-0.00249365237209801,-0.0386630644519539,
-0.0123555753639932));
#42376=CARTESIAN_POINT('Ctrl Pts',(-0.00249176821676331,-0.0386646650376619,
-0.0123800424688974));
#42377=CARTESIAN_POINT('Ctrl Pts',(-0.00248428018473284,-0.0386700584900563,
-0.0124615810786516));
#42378=CARTESIAN_POINT('Ctrl Pts',(-0.00247707319844085,-0.0386739194021167,
-0.0125184839774196));
#42379=CARTESIAN_POINT('Ctrl Pts',(-0.00245208809609394,-0.0386845828625149,
-0.0126729338391774));
#42380=CARTESIAN_POINT('Ctrl Pts',(-0.00243045421006269,-0.0386914666641234,
-0.0127697525762979));
#42381=CARTESIAN_POINT('Ctrl Pts',(-0.00236390107356713,-0.0387081694153858,
-0.0130018211908673));
#42382=CARTESIAN_POINT('Ctrl Pts',(-0.00231305860326874,-0.0387179181450143,
-0.0131350304199771));
#42383=CARTESIAN_POINT('Ctrl Pts',(-0.00222950165528394,-0.0387306184707593,
-0.0133080191354538));
#42384=CARTESIAN_POINT('Ctrl Pts',(-0.00220651970562422,-0.0387338669896611,
-0.0133521816792891));
#42385=CARTESIAN_POINT('Ctrl Pts',(-0.00216504003097869,-0.0387393401469098,
-0.0134263905324124));
#42386=CARTESIAN_POINT('Ctrl Pts',(-0.002147197793653,-0.0387415861795271,
-0.0134567840318599));
#42387=CARTESIAN_POINT('Ctrl Pts',(-0.00210881831015474,-0.0387462050882495,
-0.0135191051302542));
#42388=CARTESIAN_POINT('Ctrl Pts',(-0.00208818446062511,-0.0387485738136454,
-0.0135509627648386));
#42389=CARTESIAN_POINT('Ctrl Pts',(-0.00202943520538178,-0.0387550247851162,
-0.0136372948247452));
#42390=CARTESIAN_POINT('Ctrl Pts',(-0.00198985916723715,-0.0387590537203214,
-0.0136907394795097));
#42391=CARTESIAN_POINT('Ctrl Pts',(-0.00189122147994072,-0.0387684592594367,
-0.0138133963399071));
#42392=CARTESIAN_POINT('Ctrl Pts',(-0.00183042108274609,-0.0387737782323989,
-0.0138810881466482));
#42393=CARTESIAN_POINT('Ctrl Pts',(-0.0016494666492127,-0.038788668536376,
-0.0140616948377055));
#42394=CARTESIAN_POINT('Ctrl Pts',(-0.00152166415045526,-0.0387981354467401,
-0.0141662461622445));
#42395=CARTESIAN_POINT('Ctrl Pts',(-0.00136019816630597,-0.0388100776589811,
-0.0142736413717688));
#42396=CARTESIAN_POINT('Ctrl Pts',(-0.00133558637285986,-0.0388118981312168,
-0.0142893959929954));
#42397=CARTESIAN_POINT('Ctrl Pts',(-0.00129376564683746,-0.0388150016437606,
-0.0143151443325941));
#42398=CARTESIAN_POINT('Ctrl Pts',(-0.00127670373178246,-0.0388162708107099,
-0.014325370273962));
#42399=CARTESIAN_POINT('Ctrl Pts',(-0.00123840317315041,-0.0388191287941554,
-0.0143477085349456));
#42400=CARTESIAN_POINT('Ctrl Pts',(-0.00121710719233605,-0.0388207231919584,
-0.0143597139993317));
#42401=CARTESIAN_POINT('Ctrl Pts',(-0.0011457327398832,-0.0388260759543795,
-0.0143985826500701));
#42402=CARTESIAN_POINT('Ctrl Pts',(-0.00109491731420809,-0.0388299012209369,
-0.0144240491060759));
#42403=CARTESIAN_POINT('Ctrl Pts',(-0.000954660070359158,-0.0388404184066393,
-0.0144884566441129));
#42404=CARTESIAN_POINT('Ctrl Pts',(-0.000863735013469948,-0.0388471896278612,
-0.0145239314082387));
#42405=CARTESIAN_POINT('Ctrl Pts',(-0.000633224283974524,-0.0388639605164184,
-0.0145986607716618));
#42406=CARTESIAN_POINT('Ctrl Pts',(-0.000491839383571248,-0.0388738884426874,
-0.0146312704023529));
#42407=CARTESIAN_POINT('Ctrl Pts',(-0.000299115103153614,-0.0388867559307366,
-0.0146583939942214));
#42408=CARTESIAN_POINT('Ctrl Pts',(-0.000249620515464944,-0.0388900053641852,
-0.0146638581836792));
#42409=CARTESIAN_POINT('Ctrl Pts',(-0.00016490382937219,-0.0388954771094111,
-0.0146706570654864));
#42410=CARTESIAN_POINT('Ctrl Pts',(-0.000129757936991223,-0.0388977209113932,
-0.0146727317870172));
#42411=CARTESIAN_POINT('Ctrl Pts',(-5.67420519562254E-5,-0.0389023322616905,
-0.0146754960583138));
#42412=CARTESIAN_POINT('Ctrl Pts',(-1.88765179014198E-5,-0.0389046957291191,
-0.0146760687894049));
#42413=CARTESIAN_POINT('Ctrl Pts',(8.51414429488758E-5,-0.0389111220835623,
-0.0146752786859037));
#42414=CARTESIAN_POINT('Ctrl Pts',(0.000151251255901054,-0.0389151322283889,
-0.0146721506443055));
#42415=CARTESIAN_POINT('Ctrl Pts',(0.000307074464708355,-0.0389244802779819,
-0.0146585636473454));
#42416=CARTESIAN_POINT('Ctrl Pts',(0.000396498523842506,-0.03892976153709,
-0.0146458605141264));
#42417=CARTESIAN_POINT('Ctrl Pts',(0.000648175173277603,-0.038944703853889,
-0.0145960850933967));
#42418=CARTESIAN_POINT('Ctrl Pts',(0.000807661391825655,-0.0389542538528716,
-0.014547629573628));
#42419=CARTESIAN_POINT('Ctrl Pts',(0.000987932963469518,-0.0389662832808593,
-0.0144725533308203));
#42420=CARTESIAN_POINT('Ctrl Pts',(0.00101453239613327,-0.0389680921686267,
-0.0144609280080553));
#42421=CARTESIAN_POINT('Ctrl Pts',(0.00105898316035181,-0.0389711822944906,
-0.0144405716535904));
#42422=CARTESIAN_POINT('Ctrl Pts',(0.00107694326699847,-0.0389724499489362,
-0.0144320863823738));
#42423=CARTESIAN_POINT('Ctrl Pts',(0.0011168732102256,-0.0389753133933625,
-0.0144126360189723));
#42424=CARTESIAN_POINT('Ctrl Pts',(0.00113878447881048,-0.038976914954726,
-0.0144015604911461));
#42425=CARTESIAN_POINT('Ctrl Pts',(0.00121147683354711,-0.0389823216371654,
-0.014363462181737));
#42426=CARTESIAN_POINT('Ctrl Pts',(0.00126148515472098,-0.038986195375057,
-0.0143350112252988));
#42427=CARTESIAN_POINT('Ctrl Pts',(0.00139532051531692,-0.0389969092163965,
-0.0142526319094823));
#42428=CARTESIAN_POINT('Ctrl Pts',(0.00147697606317126,-0.0390038315090007,
-0.0141953753644116));
#42429=CARTESIAN_POINT('Ctrl Pts',(0.00166621912727251,-0.0390205555538059,
-0.0140450485340773));
#42430=CARTESIAN_POINT('Ctrl Pts',(0.00176972424034835,-0.0390302870575528,
-0.013947367539907));
#42431=CARTESIAN_POINT('Ctrl Pts',(0.00189756114235087,-0.0390429736575671,
-0.013804270334125));
#42432=CARTESIAN_POINT('Ctrl Pts',(0.00192962573124047,-0.0390462245870136,
-0.0137661442873352));
#42433=CARTESIAN_POINT('Ctrl Pts',(0.00198239638551046,-0.0390517001987144,
-0.0136994497731451));
#42434=CARTESIAN_POINT('Ctrl Pts',(0.00200367512871736,-0.0390539463436724,
-0.0136713558315795));
#42435=CARTESIAN_POINT('Ctrl Pts',(0.00204660704290472,-0.0390585639141946,
-0.0136121115660901));
#42436=CARTESIAN_POINT('Ctrl Pts',(0.0020681595910738,-0.0390609312232226,
-0.0135808993274417));
#42437=CARTESIAN_POINT('Ctrl Pts',(0.00212544510123207,-0.0390673737801507,
-0.0134937629408868));
#42438=CARTESIAN_POINT('Ctrl Pts',(0.00215967574304779,-0.0390713959738459,
-0.0134368863849838));
#42439=CARTESIAN_POINT('Ctrl Pts',(0.00223523865355963,-0.0390807820641926,
-0.0132992109336272));
#42440=CARTESIAN_POINT('Ctrl Pts',(0.00227451593090324,-0.0390860887191309,
-0.0132173919782099));
#42441=CARTESIAN_POINT('Ctrl Pts',(0.00237247999309516,-0.0391009843188402,
-0.0129811909976451));
#42442=CARTESIAN_POINT('Ctrl Pts',(0.00242044395373002,-0.0391104675045367,
-0.0128228990157841));
#42443=CARTESIAN_POINT('Ctrl Pts',(0.00245812802713222,-0.0391224260989022,
-0.012632425952674));
#42444=CARTESIAN_POINT('Ctrl Pts',(0.00246329091039689,-0.039124244699187,
-0.0126036963861636));
#42445=CARTESIAN_POINT('Ctrl Pts',(0.00247113200339487,-0.0391273492930154,
-0.0125552003768462));
#42446=CARTESIAN_POINT('Ctrl Pts',(0.00247407872878765,-0.0391286215627706,
-0.0125354808750266));
#42447=CARTESIAN_POINT('Ctrl Pts',(0.00248014228871132,-0.0391314966252482,
-0.0124912934162562));
#42448=CARTESIAN_POINT('Ctrl Pts',(0.00248313327375542,-0.0391331052280717,
-0.01246681253051));
#42449=CARTESIAN_POINT('Ctrl Pts',(0.00249193257048902,-0.0391385434541255,
-0.0123847189511998));
#42450=CARTESIAN_POINT('Ctrl Pts',(0.00249610112657119,-0.0391424421493603,
-0.0123269524689338));
#42451=CARTESIAN_POINT('Ctrl Pts',(0.00249942029500609,-0.0391485070700073,
-0.0122380236399158));
#42452=CARTESIAN_POINT('Ctrl Pts',(0.00249999999972546,-0.039150639079543,
-0.0122069366733935));
#42453=CARTESIAN_POINT('Ctrl Pts',(0.0025,-0.0391527785410365,-0.0121758533086393));
#42454=CARTESIAN_POINT('Origin',(0.,-0.0320674495244671,-0.0121758532865581));
#42455=CARTESIAN_POINT('',(0.00199999982444772,-0.0355681130672164,-0.0121766912657388));
#42456=CARTESIAN_POINT('',(0.00199999947635761,-0.0395674495244771,-0.0121744060238692));
#42457=CARTESIAN_POINT('Ctrl Pts',(0.00199999982024451,-0.0355681123252202,
-0.012176701238172));
#42458=CARTESIAN_POINT('Ctrl Pts',(0.00200006372026205,-0.0355794597712501,
-0.0120241914541404));
#42459=CARTESIAN_POINT('Ctrl Pts',(0.00198268576079593,-0.0355906127106426,
-0.0118721885649424));
#42460=CARTESIAN_POINT('Ctrl Pts',(0.00193848766546422,-0.0356055917189111,
-0.0116817755903345));
#42461=CARTESIAN_POINT('Ctrl Pts',(0.00192742358701769,-0.0356089198116543,
-0.0116402368105887));
#42462=CARTESIAN_POINT('Ctrl Pts',(0.00190503977995606,-0.0356150065308702,
-0.0115659157952878));
#42463=CARTESIAN_POINT('Ctrl Pts',(0.00189418901858273,-0.0356177493846711,
-0.0115330096239274));
#42464=CARTESIAN_POINT('Ctrl Pts',(0.00186779778516884,-0.0356239990331276,
-0.0114594567864354));
#42465=CARTESIAN_POINT('Ctrl Pts',(0.00185177489705482,-0.0356275202053536,
-0.0114190034607499));
#42466=CARTESIAN_POINT('Ctrl Pts',(0.00178163648056277,-0.035641937928567,
-0.0112575150145211));
#42467=CARTESIAN_POINT('Ctrl Pts',(0.0017168759052299,-0.0356531670735535,
-0.0111414938200488));
#42468=CARTESIAN_POINT('Ctrl Pts',(0.00158630110163576,-0.0356726271273577,
-0.0109540300345471));
#42469=CARTESIAN_POINT('Ctrl Pts',(0.00152587214325114,-0.035680796332212,
-0.0108793499726965));
#42470=CARTESIAN_POINT('Ctrl Pts',(0.00144138352066207,-0.0356910127280173,
-0.0107890653288063));
#42471=CARTESIAN_POINT('Ctrl Pts',(0.0014220370205924,-0.0356932797316201,
-0.0107692338527021));
#42472=CARTESIAN_POINT('Ctrl Pts',(0.00138807260355076,-0.0356971286291267,
-0.0107358353475258));
#42473=CARTESIAN_POINT('Ctrl Pts',(0.00137365409092878,-0.035698723266576,
-0.0107220748466189));
#42474=CARTESIAN_POINT('Ctrl Pts',(0.00133834199944169,-0.0357025365378354,
-0.0106893688930189));
#42475=CARTESIAN_POINT('Ctrl Pts',(0.00131724931101274,-0.0357047402412553,
-0.0106706457762239));
#42476=CARTESIAN_POINT('Ctrl Pts',(0.00121130063664286,-0.0357154932467055,
-0.0105805331791964));
#42477=CARTESIAN_POINT('Ctrl Pts',(0.00112099543299248,-0.0357236923468493,
-0.0105158318527037));
#42478=CARTESIAN_POINT('Ctrl Pts',(0.000921758513265947,-0.0357408903643568,
-0.010396796125477));
#42479=CARTESIAN_POINT('Ctrl Pts',(0.000812315465694571,-0.0357498646982703,
-0.0103442359697735));
#42480=CARTESIAN_POINT('Ctrl Pts',(0.000659580232080265,-0.0357623763237561,
-0.0102872808846941));
#42481=CARTESIAN_POINT('Ctrl Pts',(0.000619917109655637,-0.0357656222333493,
-0.0102738926916546));
#42482=CARTESIAN_POINT('Ctrl Pts',(0.000546667388170452,-0.0357716313162415,
-0.0102517020323112));
#42483=CARTESIAN_POINT('Ctrl Pts',(0.000513215134607283,-0.0357743809373372,
-0.0102425107890887));
#42484=CARTESIAN_POINT('Ctrl Pts',(0.000436764745341417,-0.0357806864999606,
-0.0102236293904429));
#42485=CARTESIAN_POINT('Ctrl Pts',(0.000393652824776714,-0.0357842578177142,
-0.0102144817173615));
#42486=CARTESIAN_POINT('Ctrl Pts',(0.000240790077661422,-0.0357969897704358,
-0.0101872892550173));
#42487=CARTESIAN_POINT('Ctrl Pts',(0.000129885668804329,-0.0358063652388844,
-0.0101769812420771));
#42488=CARTESIAN_POINT('Ctrl Pts',(-6.11586135789818E-5,-0.0358226233301814,
-0.010175193354002));
#42489=CARTESIAN_POINT('Ctrl Pts',(-0.000141008646280326,-0.0358294462804263,
-0.0101792316712571));
#42490=CARTESIAN_POINT('Ctrl Pts',(-0.000254445753695718,-0.0358390538608624,
-0.0101918093448361));
#42491=CARTESIAN_POINT('Ctrl Pts',(-0.000288385940867445,-0.0358419168192868,
-0.0101964577098354));
#42492=CARTESIAN_POINT('Ctrl Pts',(-0.000349699788095021,-0.0358470510388757,
-0.0102064658446794));
#42493=CARTESIAN_POINT('Ctrl Pts',(-0.000377112774462912,-0.0358493326318625,
-0.0102115307511461));
#42494=CARTESIAN_POINT('Ctrl Pts',(-0.000423932077242514,-0.0358531961727089,
-0.0102211976045163));
#42495=CARTESIAN_POINT('Ctrl Pts',(-0.000443389608732699,-0.0358547912056612,
-0.0102255192136858));
#42496=CARTESIAN_POINT('Ctrl Pts',(-0.000490050054016354,-0.0358585917999575,
-0.0102366172123026));
#42497=CARTESIAN_POINT('Ctrl Pts',(-0.000517180748175394,-0.0358607827895064,
-0.0102436757807234));
#42498=CARTESIAN_POINT('Ctrl Pts',(-0.000652679796783529,-0.0358716721326215,
-0.010281987393025));
#42499=CARTESIAN_POINT('Ctrl Pts',(-0.00075842854558731,-0.035880005855045,
-0.0103218004766724));
#42500=CARTESIAN_POINT('Ctrl Pts',(-0.00096794045489743,-0.0358972030104413,
-0.0104216250891795));
#42501=CARTESIAN_POINT('Ctrl Pts',(-0.00107079616282311,-0.0359060409762,
-0.0104824495340128));
#42502=CARTESIAN_POINT('Ctrl Pts',(-0.00120169692900742,-0.0359184136484365,
-0.01057657635546));
#42503=CARTESIAN_POINT('Ctrl Pts',(-0.00123499658228157,-0.035921668618646,
-0.0106021490013148));
#42504=CARTESIAN_POINT('Ctrl Pts',(-0.0012942905310538,-0.0359276858318921,
-0.0106507255484452));
#42505=CARTESIAN_POINT('Ctrl Pts',(-0.00132053825984378,-0.0359304342716035,
-0.0106733949658894));
#42506=CARTESIAN_POINT('Ctrl Pts',(-0.00137864976963684,-0.0359367251809057,
-0.0107262836388159));
#42507=CARTESIAN_POINT('Ctrl Pts',(-0.00141013315643489,-0.0359402827313761,
-0.0107568919643324));
#42508=CARTESIAN_POINT('Ctrl Pts',(-0.00152408621630788,-0.0359537509296682,
-0.0108752178177149));
#42509=CARTESIAN_POINT('Ctrl Pts',(-0.00159957882847991,-0.0359639230180368,
-0.0109692753529544));
#42510=CARTESIAN_POINT('Ctrl Pts',(-0.00170710264158098,-0.035980475882862,
-0.0111312088692722));
#42511=CARTESIAN_POINT('Ctrl Pts',(-0.0017446018404604,-0.0359867916363548,
-0.0111951154771363));
#42512=CARTESIAN_POINT('Ctrl Pts',(-0.00179356410142959,-0.0359957910075969,
-0.0112902934412212));
#42513=CARTESIAN_POINT('Ctrl Pts',(-0.00180792867997445,-0.0359985452964401,
-0.011320001321169));
#42514=CARTESIAN_POINT('Ctrl Pts',(-0.00183276148622826,-0.0360035101793772,
-0.0113747775774794));
#42515=CARTESIAN_POINT('Ctrl Pts',(-0.00184346673962206,-0.0360057301245718,
-0.0113997298737214));
#42516=CARTESIAN_POINT('Ctrl Pts',(-0.00186115029722121,-0.036009533059476,
-0.0114433798230547));
#42517=CARTESIAN_POINT('Ctrl Pts',(-0.00186836208859691,-0.0360111276722849,
-0.0114619758484414));
#42518=CARTESIAN_POINT('Ctrl Pts',(-0.00188531037198073,-0.036014988136515,
-0.0115076953942276));
#42519=CARTESIAN_POINT('Ctrl Pts',(-0.00189474105435947,-0.0360172377768593,
-0.0115349268048528));
#42520=CARTESIAN_POINT('Ctrl Pts',(-0.00193115712472691,-0.0360264065448639,
-0.0116479195779665));
#42521=CARTESIAN_POINT('Ctrl Pts',(-0.00195293644909198,-0.0360331073892564,
-0.0117352572024554));
#42522=CARTESIAN_POINT('Ctrl Pts',(-0.0019853316361911,-0.0360467624467822,
-0.011916405108863));
#42523=CARTESIAN_POINT('Ctrl Pts',(-0.00199533846551933,-0.036053698626972,
-0.0120100868097281));
#42524=CARTESIAN_POINT('Ctrl Pts',(-0.0020003881931414,-0.0360642836288285,
-0.0121507930589636));
#42525=CARTESIAN_POINT('Ctrl Pts',(-0.00200042786321385,-0.0360678238759117,
-0.0121975048735993));
#42526=CARTESIAN_POINT('Ctrl Pts',(-0.00199740348698823,-0.0360746195085124,
-0.012285989610768));
#42527=CARTESIAN_POINT('Ctrl Pts',(-0.00199466240655691,-0.0360778644388145,
-0.012327748354794));
#42528=CARTESIAN_POINT('Ctrl Pts',(-0.00198725762500653,-0.036083872349982,
-0.0124039108243686));
#42529=CARTESIAN_POINT('Ctrl Pts',(-0.00198300386623346,-0.0360866217990032,
-0.0124383384854523));
#42530=CARTESIAN_POINT('Ctrl Pts',(-0.00197131777385926,-0.0360929277669059,
-0.0125162184114001));
#42531=CARTESIAN_POINT('Ctrl Pts',(-0.00196333996898166,-0.0360964996806398,
-0.0125595689953699));
#42532=CARTESIAN_POINT('Ctrl Pts',(-0.0019300162148669,-0.0361093061827661,
-0.0127121416170955));
#42533=CARTESIAN_POINT('Ctrl Pts',(-0.00189693212423113,-0.0361187599113526,
-0.012819444070496));
#42534=CARTESIAN_POINT('Ctrl Pts',(-0.00182541617002246,-0.0361350437807657,
-0.0129969125567394));
#42535=CARTESIAN_POINT('Ctrl Pts',(-0.00179144520815108,-0.0361418133250543,
-0.013068605977944));
#42536=CARTESIAN_POINT('Ctrl Pts',(-0.0017368920806125,-0.0361513571589629,
-0.0131680075523525));
#42537=CARTESIAN_POINT('Ctrl Pts',(-0.00171971231131524,-0.0361542089908726,
-0.0131974961040721));
#42538=CARTESIAN_POINT('Ctrl Pts',(-0.00168718221683256,-0.0361593258803548,
-0.013250185112041));
#42539=CARTESIAN_POINT('Ctrl Pts',(-0.00167208643035337,-0.0361616011693833,
-0.0132735326120951));
#42540=CARTESIAN_POINT('Ctrl Pts',(-0.00164533981366778,-0.0361654583374121,
-0.0133130665932397));
#42541=CARTESIAN_POINT('Ctrl Pts',(-0.00163392606599862,-0.0361670531549552,
-0.0133294055898316));
#42542=CARTESIAN_POINT('Ctrl Pts',(-0.0016058338486083,-0.0361708590092413,
-0.0133683662851926));
#42543=CARTESIAN_POINT('Ctrl Pts',(-0.00158891961221953,-0.0361730553229059,
-0.0133908118462923));
#42544=CARTESIAN_POINT('Ctrl Pts',(-0.00150226140911318,-0.0361838887961957,
-0.0135009023416009));
#42545=CARTESIAN_POINT('Ctrl Pts',(-0.00142570636290487,-0.0361921672906417,
-0.0135829468599513));
#42546=CARTESIAN_POINT('Ctrl Pts',(-0.00125386045995633,-0.036209348524211,
-0.0137386052476914));
#42547=CARTESIAN_POINT('Ctrl Pts',(-0.00115800658124893,-0.036218226208243,
-0.0138108994262984));
#42548=CARTESIAN_POINT('Ctrl Pts',(-0.00102060073360294,-0.0362306433212439,
-0.0138963585029053));
#42549=CARTESIAN_POINT('Ctrl Pts',(-0.000984248091122991,-0.0362338998993086,
-0.0139174098533958));
#42550=CARTESIAN_POINT('Ctrl Pts',(-0.00091672024282943,-0.0362399186717001,
-0.0139537246461715));
#42551=CARTESIAN_POINT('Ctrl Pts',(-0.000885758358559603,-0.0362426670206583,
-0.013969351100869));
#42552=CARTESIAN_POINT('Ctrl Pts',(-0.000814735762173941,-0.0362489558175553,
-0.0140029085308272));
#42553=CARTESIAN_POINT('Ctrl Pts',(-0.000774460978011599,-0.0362525112998127,
-0.0140203409726528));
#42554=CARTESIAN_POINT('Ctrl Pts',(-0.00062117534750794,-0.0362660197545799,
-0.0140807832834877));
#42555=CARTESIAN_POINT('Ctrl Pts',(-0.000504929781915352,-0.0362762370013897,
-0.0141148360713988));
#42556=CARTESIAN_POINT('Ctrl Pts',(-0.00031400039851391,-0.0362928084016039,
-0.0141524260297192));
#42557=CARTESIAN_POINT('Ctrl Pts',(-0.00024092448432737,-0.0362990974789354,
-0.014162657831295));
#42558=CARTESIAN_POINT('Ctrl Pts',(-0.000134640675424076,-0.0363080646695565,
-0.0141715876893407));
#42559=CARTESIAN_POINT('Ctrl Pts',(-0.000101768181975097,-0.0363108130403072,
-0.0141735337982387));
#42560=CARTESIAN_POINT('Ctrl Pts',(-4.17693200385002E-5,-0.0363157686887946,
-0.014175600804675));
#42561=CARTESIAN_POINT('Ctrl Pts',(-1.46597800301764E-5,-0.0363179852644014,
-0.0141759833116636));
#42562=CARTESIAN_POINT('Ctrl Pts',(3.23980952306466E-5,-0.0363217850113142,
-0.0141756903456227));
#42563=CARTESIAN_POINT('Ctrl Pts',(5.23414829159846E-5,-0.0363233797236368,
-0.0141752677896181));
#42564=CARTESIAN_POINT('Ctrl Pts',(0.000101121151082956,-0.0363272440808545,
-0.0141735037880477));
#42565=CARTESIAN_POINT('Ctrl Pts',(0.000129940499311205,-0.0363294974133465,
-0.0141718364356037));
#42566=CARTESIAN_POINT('Ctrl Pts',(0.000239504866029927,-0.0363379854765585,
-0.0141631141299244));
#42567=CARTESIAN_POINT('Ctrl Pts',(0.000319837839623694,-0.0363440477291476,
-0.0141517771136954));
#42568=CARTESIAN_POINT('Ctrl Pts',(0.000496974397509341,-0.0363574810042967,
-0.0141156880795133));
#42569=CARTESIAN_POINT('Ctrl Pts',(0.000593051196616829,-0.0363648169862106,
-0.0140885038413577));
#42570=CARTESIAN_POINT('Ctrl Pts',(0.000731652186469292,-0.0363758987839011,
-0.0140378350200237));
#42571=CARTESIAN_POINT('Ctrl Pts',(0.000775998466777736,-0.0363795227651278,
-0.0140197938329827));
#42572=CARTESIAN_POINT('Ctrl Pts',(0.000858440401884898,-0.0363864530415998,
-0.013982753471274));
#42573=CARTESIAN_POINT('Ctrl Pts',(0.000896659778307296,-0.0363897477997356,
-0.0139640951468769));
#42574=CARTESIAN_POINT('Ctrl Pts',(0.000964897014594833,-0.0363958025841946,
-0.0139280447441654));
#42575=CARTESIAN_POINT('Ctrl Pts',(0.000995112987960803,-0.0363985477368804,
-0.0139110624957629));
#42576=CARTESIAN_POINT('Ctrl Pts',(0.00106266552078047,-0.0364048421383324,
-0.0138707512482148));
#42577=CARTESIAN_POINT('Ctrl Pts',(0.00109970233186019,-0.0364084067253401,
-0.0138469580969806));
#42578=CARTESIAN_POINT('Ctrl Pts',(0.00123997348430849,-0.0364223726537744,
-0.0137501620768282));
#42579=CARTESIAN_POINT('Ctrl Pts',(0.0013369667065856,-0.0364330687912483,
-0.0136686669071304));
#42580=CARTESIAN_POINT('Ctrl Pts',(0.00149610190982521,-0.0364523943736247,
-0.0135069361771168));
#42581=CARTESIAN_POINT('Ctrl Pts',(0.00156110230431907,-0.0364609645555744,
-0.0134300724832778));
#42582=CARTESIAN_POINT('Ctrl Pts',(0.00163634900559828,-0.036471568196491,
-0.0133261290362688));
#42583=CARTESIAN_POINT('Ctrl Pts',(0.00165217600870689,-0.0364738429721809,
-0.0133032782432026));
#42584=CARTESIAN_POINT('Ctrl Pts',(0.00167852654934271,-0.036477699626104,
-0.0132634864187557));
#42585=CARTESIAN_POINT('Ctrl Pts',(0.00168928124936084,-0.0364792944308592,
-0.0132467062950394));
#42586=CARTESIAN_POINT('Ctrl Pts',(0.00171459537322141,-0.0364831007346985,
-0.0132058788423459));
#42587=CARTESIAN_POINT('Ctrl Pts',(0.00172890187146586,-0.0364852974979562,
-0.0131816805546013));
#42588=CARTESIAN_POINT('Ctrl Pts',(0.00179761640926801,-0.0364961260347862,
-0.0130596543222264));
#42589=CARTESIAN_POINT('Ctrl Pts',(0.0018442609683476,-0.0365043996609087,
-0.0129576698337327));
#42590=CARTESIAN_POINT('Ctrl Pts',(0.00192282970617978,-0.0365216129858041,
-0.012739063849049));
#42591=CARTESIAN_POINT('Ctrl Pts',(0.00195322242421475,-0.0365305277238056,
-0.0126223929710588));
#42592=CARTESIAN_POINT('Ctrl Pts',(0.00197980524934267,-0.0365429744671278,
-0.0124624235186765));
#42593=CARTESIAN_POINT('Ctrl Pts',(0.00198536747266429,-0.0365462199454981,
-0.0124209386791781));
#42594=CARTESIAN_POINT('Ctrl Pts',(0.00199315274703356,-0.0365522284004654,
-0.012344806646019));
#42595=CARTESIAN_POINT('Ctrl Pts',(0.00199578285507167,-0.0365549778312713,
-0.0123102170112996));
#42596=CARTESIAN_POINT('Ctrl Pts',(0.00199970923124176,-0.0365612831174252,
-0.012231571082258));
#42597=CARTESIAN_POINT('Ctrl Pts',(0.00200045121779198,-0.0365648543519947,
-0.0121875067441161));
#42598=CARTESIAN_POINT('Ctrl Pts',(0.00199787936999445,-0.0365778743717673,
-0.0120287527085681));
#42599=CARTESIAN_POINT('Ctrl Pts',(0.00198615585864129,-0.0365875550820124,
-0.0119144382283467));
#42600=CARTESIAN_POINT('Ctrl Pts',(0.00195020696594567,-0.0366039162872233,
-0.0117256297574465));
#42601=CARTESIAN_POINT('Ctrl Pts',(0.00193129384625522,-0.0366105340398136,
-0.0116503884201844));
#42602=CARTESIAN_POINT('Ctrl Pts',(0.00189794514378554,-0.0366198964107415,
-0.011544233682504));
#42603=CARTESIAN_POINT('Ctrl Pts',(0.00188701570073092,-0.0366227162880287,
-0.0115122938507159));
#42604=CARTESIAN_POINT('Ctrl Pts',(0.00186569357881676,-0.0366277834698879,
-0.0114547787914556));
#42605=CARTESIAN_POINT('Ctrl Pts',(0.00185556992208626,-0.0366300407145318,
-0.0114291127388221));
#42606=CARTESIAN_POINT('Ctrl Pts',(0.00183722180171872,-0.0366338800318558,
-0.0113852754187023));
#42607=CARTESIAN_POINT('Ctrl Pts',(0.00182925162866056,-0.0366354746151612,
-0.0113670047917613));
#42608=CARTESIAN_POINT('Ctrl Pts',(0.00180929696405246,-0.0366392973887674,
-0.0113230656920839));
#42609=CARTESIAN_POINT('Ctrl Pts',(0.00179703810793846,-0.0366415103902769,
-0.0112975273427616));
#42610=CARTESIAN_POINT('Ctrl Pts',(0.00173484031386666,-0.0366521513416018,
-0.0111747117790803));
#42611=CARTESIAN_POINT('Ctrl Pts',(0.00167751805348371,-0.0366602404907024,
-0.0110813695613111));
#42612=CARTESIAN_POINT('Ctrl Pts',(0.00154221229859184,-0.0366771959744809,
-0.0108968505532088));
#42613=CARTESIAN_POINT('Ctrl Pts',(0.00146310180609141,-0.0366860378516589,
-0.0108070598422564));
#42614=CARTESIAN_POINT('Ctrl Pts',(0.00134533816331753,-0.0366984779481924,
-0.0106953447984558));
#42615=CARTESIAN_POINT('Ctrl Pts',(0.00131327719910589,-0.0367018000737338,
-0.0106668328586224));
#42616=CARTESIAN_POINT('Ctrl Pts',(0.00125370667310763,-0.0367078813130874,
-0.0106171935308863));
#42617=CARTESIAN_POINT('Ctrl Pts',(0.00122651659506477,-0.0367106248218075,
-0.0105957085450076));
#42618=CARTESIAN_POINT('Ctrl Pts',(0.00116388285386699,-0.036716883315838,
-0.0105488075646894));
#42619=CARTESIAN_POINT('Ctrl Pts',(0.00112813952302434,-0.0367204128576432,
-0.0105238237142059));
#42620=CARTESIAN_POINT('Ctrl Pts',(0.000981421472766178,-0.0367347536325225,
-0.0104282533735347));
#42621=CARTESIAN_POINT('Ctrl Pts',(0.000864438985207459,-0.0367458906898303,
-0.0103675314923803));
#42622=CARTESIAN_POINT('Ctrl Pts',(0.000651008998317222,-0.036765469335323,
-0.0102822146053174));
#42623=CARTESIAN_POINT('Ctrl Pts',(0.000557070931437676,-0.0367738493888426,
-0.0102524823325248));
#42624=CARTESIAN_POINT('Ctrl Pts',(0.000435079241419324,-0.0367841961595787,
-0.0102235640634526));
#42625=CARTESIAN_POINT('Ctrl Pts',(0.000408715479801509,-0.0367864006928543,
-0.0102178749861448));
#42626=CARTESIAN_POINT('Ctrl Pts',(0.000362656642195421,-0.0367901888975908,
-0.0102089068399541));
#42627=CARTESIAN_POINT('Ctrl Pts',(0.000343015162755336,-0.0367917838218753,
-0.010205386629613));
#42628=CARTESIAN_POINT('Ctrl Pts',(0.000294672083937837,-0.0367956614092112,
-0.0101974672831097));
#42629=CARTESIAN_POINT('Ctrl Pts',(0.000265921688213696,-0.0367979274068945,
-0.0101933980596849));
#42630=CARTESIAN_POINT('Ctrl Pts',(0.00011077062147708,-0.0368099910242354,
-0.0101748750056979));
#42631=CARTESIAN_POINT('Ctrl Pts',(-1.6717160445149E-5,-0.0368193305906831,
-0.0101718789178745));
#42632=CARTESIAN_POINT('Ctrl Pts',(-0.000231171361878576,-0.0368352761668842,
-0.0101873208122118));
#42633=CARTESIAN_POINT('Ctrl Pts',(-0.000318186300452089,-0.0368418104483716,
-0.0101993773882134));
#42634=CARTESIAN_POINT('Ctrl Pts',(-0.00045092032500571,-0.0368521353863758,
-0.0102267627141409));
#42635=CARTESIAN_POINT('Ctrl Pts',(-0.000497352755849111,-0.0368558155848458,
-0.0102380909765576));
#42636=CARTESIAN_POINT('Ctrl Pts',(-0.000576916653033613,-0.0368622724481259,
-0.0102605504405343));
#42637=CARTESIAN_POINT('Ctrl Pts',(-0.000610245388870597,-0.0368650239699315,
-0.0102709075957314));
#42638=CARTESIAN_POINT('Ctrl Pts',(-0.000681156106117241,-0.0368709897004767,
-0.0102949954651788));
#42639=CARTESIAN_POINT('Ctrl Pts',(-0.000718630676713551,-0.0368742114057743,
-0.0103089924779559));
#42640=CARTESIAN_POINT('Ctrl Pts',(-0.000831041777317918,-0.0368840994627731,
-0.010354864923161));
#42641=CARTESIAN_POINT('Ctrl Pts',(-0.000904466566600802,-0.0368908714180335,
-0.0103901976627558));
#42642=CARTESIAN_POINT('Ctrl Pts',(-0.000987785497383913,-0.0368989222239252,
-0.0104367509228298));
#42643=CARTESIAN_POINT('Ctrl Pts',(-0.000999972495799115,-0.0369001092775983,
-0.0104437296716397));
#42644=CARTESIAN_POINT('Ctrl Pts',(-0.00109879587062757,-0.0369098109023126,
-0.0105017103330895));
#42645=CARTESIAN_POINT('Ctrl Pts',(-0.00118154606627001,-0.0369184242447914,
-0.0105590491440091));
#42646=CARTESIAN_POINT('Ctrl Pts',(-0.00128919238539798,-0.0369301266041836,
-0.0106463333847669));
#42647=CARTESIAN_POINT('Ctrl Pts',(-0.00131806276453473,-0.0369333187145092,
-0.0106711410037714));
#42648=CARTESIAN_POINT('Ctrl Pts',(-0.00136839499946266,-0.036938959943791,
-0.0107169512809244));
#42649=CARTESIAN_POINT('Ctrl Pts',(-0.0013901252578126,-0.0369414225563398,
-0.0107376419039902));
#42650=CARTESIAN_POINT('Ctrl Pts',(-0.00142543442538057,-0.0369454587846278,
-0.0107728101682445));
#42651=CARTESIAN_POINT('Ctrl Pts',(-0.00143927695279488,-0.0369470500152991,
-0.0107870137439042));
#42652=CARTESIAN_POINT('Ctrl Pts',(-0.00147053087133148,-0.0369506624780771,
-0.0108200522015299));
#42653=CARTESIAN_POINT('Ctrl Pts',(-0.00148779527697202,-0.0369526738235214,
-0.0108390200791985));
#42654=CARTESIAN_POINT('Ctrl Pts',(-0.00155897217816492,-0.0369610613967223,
-0.0109203075463372));
#42655=CARTESIAN_POINT('Ctrl Pts',(-0.00160937733924054,-0.036967241439652,
-0.0109856023280882));
#42656=CARTESIAN_POINT('Ctrl Pts',(-0.00171350945493643,-0.0369810495953943,
-0.0111392555550667));
#42657=CARTESIAN_POINT('Ctrl Pts',(-0.00176470394910575,-0.0369886335850651,
-0.011229032829568));
#42658=CARTESIAN_POINT('Ctrl Pts',(-0.0018294590485119,-0.0370000211949638,
-0.0113662630171804));
#42659=CARTESIAN_POINT('Ctrl Pts',(-0.00184856959207488,-0.0370036944030231,
-0.0114109044497765));
#42660=CARTESIAN_POINT('Ctrl Pts',(-0.00188148061587224,-0.0370107037148611,
-0.0114962409344938));
#42661=CARTESIAN_POINT('Ctrl Pts',(-0.0018956307601921,-0.037014027630454,
-0.0115367713091516));
#42662=CARTESIAN_POINT('Ctrl Pts',(-0.00191882798860973,-0.0370201106104126,
-0.0116107871117771));
#42663=CARTESIAN_POINT('Ctrl Pts',(-0.00192832895619941,-0.0370228540218132,
-0.0116441129603315));
#42664=CARTESIAN_POINT('Ctrl Pts',(-0.00194781330731927,-0.0370291102407018,
-0.0117198685063456));
#42665=CARTESIAN_POINT('Ctrl Pts',(-0.00195728459814625,-0.0370326375550902,
-0.0117624101640019));
#42666=CARTESIAN_POINT('Ctrl Pts',(-0.0019897824076701,-0.0370469995970621,
-0.0119347382856186));
#42667=CARTESIAN_POINT('Ctrl Pts',(-0.00200134048048048,-0.0370581619933841,
-0.0120663288976307));
#42668=CARTESIAN_POINT('Ctrl Pts',(-0.0019988059355266,-0.0370775923151151,
-0.0122944239437779));
#42669=CARTESIAN_POINT('Ctrl Pts',(-0.00199077393651083,-0.0370857986141568,
-0.0123905780112073));
#42670=CARTESIAN_POINT('Ctrl Pts',(-0.00197153582218788,-0.0370960567668822,
-0.0125132221870122));
#42671=CARTESIAN_POINT('Ctrl Pts',(-0.00196666080265298,-0.0370983298646916,
-0.0125405679533566));
#42672=CARTESIAN_POINT('Ctrl Pts',(-0.00195731153504465,-0.0371021848574262,
-0.0125873490594598));
#42673=CARTESIAN_POINT('Ctrl Pts',(-0.00195311386903877,-0.0371037796389771,
-0.0126068330177357));
#42674=CARTESIAN_POINT('Ctrl Pts',(-0.00194229091888752,-0.0371075875064836,
-0.0126536577298692));
#42675=CARTESIAN_POINT('Ctrl Pts',(-0.00193537897328492,-0.0371097858136657,
-0.0126809271075952));
#42676=CARTESIAN_POINT('Ctrl Pts',(-0.00189816994216949,-0.0371205977682293,
-0.0128157192134525));
#42677=CARTESIAN_POINT('Ctrl Pts',(-0.00185947375669505,-0.0371288550220459,
-0.0129207300905785));
#42678=CARTESIAN_POINT('Ctrl Pts',(-0.00176120925056366,-0.0371460665145463,
-0.0131311917990515));
#42679=CARTESIAN_POINT('Ctrl Pts',(-0.00170045076154391,-0.037154995894315,
-0.0132355665520264));
#42680=CARTESIAN_POINT('Ctrl Pts',(-0.00160644511961943,-0.0371674580160518,
-0.0133679459171712));
#42681=CARTESIAN_POINT('Ctrl Pts',(-0.00158115616002576,-0.0371707030051337,
-0.0134012901425602));
#42682=CARTESIAN_POINT('Ctrl Pts',(-0.00153302480183524,-0.0371767110129889,
-0.0134607805598211));
#42683=CARTESIAN_POINT('Ctrl Pts',(-0.00151051139103103,-0.0371794604993252,
-0.0134871725392997));
#42684=CARTESIAN_POINT('Ctrl Pts',(-0.00145786078653481,-0.0371857665470215,
-0.0135457380101189));
#42685=CARTESIAN_POINT('Ctrl Pts',(-0.00142732432145111,-0.0371893385032907,
-0.0135775261818474));
#42686=CARTESIAN_POINT('Ctrl Pts',(-0.00131545127428182,-0.0372021476010341,
-0.0136865361389192));
#42687=CARTESIAN_POINT('Ctrl Pts',(-0.00122870996426901,-0.0372116040285329,
-0.0137578897501099));
#42688=CARTESIAN_POINT('Ctrl Pts',(-0.00107125703818745,-0.0372278887889061,
-0.013866618653536));
#42689=CARTESIAN_POINT('Ctrl Pts',(-0.00100343167043015,-0.0372346564956022,
-0.0139077322759927));
#42690=CARTESIAN_POINT('Ctrl Pts',(-0.000903170860836162,-0.0372441981456313,
-0.0139606351466137));
#42691=CARTESIAN_POINT('Ctrl Pts',(-0.000872593367725354,-0.0372470496030501,
-0.0139757824517772));
#42692=CARTESIAN_POINT('Ctrl Pts',(-0.000816427285820691,-0.0372521659157054,
-0.0140018376941819));
#42693=CARTESIAN_POINT('Ctrl Pts',(-0.000790970096741173,-0.0372544409988147,
-0.014013008452615));
#42694=CARTESIAN_POINT('Ctrl Pts',(-0.000746873103090543,-0.0372582979665442,
-0.0140312717779441));
#42695=CARTESIAN_POINT('Ctrl Pts',(-0.000728347129689305,-0.0372598927847343,
-0.0140386221308174));
#42696=CARTESIAN_POINT('Ctrl Pts',(-0.000683438077299609,-0.037263698846043,
-0.0140556676781315));
#42697=CARTESIAN_POINT('Ctrl Pts',(-0.00065695519819512,-0.0372658953605332,
-0.0140650858965379));
#42698=CARTESIAN_POINT('Ctrl Pts',(-0.000524015625016074,-0.0372767265915936,
-0.0141092298703231));
#42699=CARTESIAN_POINT('Ctrl Pts',(-0.000414960476630937,-0.0372850028772857,
-0.0141355348438161));
#42700=CARTESIAN_POINT('Ctrl Pts',(-0.000185360621513893,-0.0373022167577775,
-0.0141708757046039));
#42701=CARTESIAN_POINT('Ctrl Pts',(-6.50619379126704E-5,-0.0373111293749187,
-0.0141784104682219));
#42702=CARTESIAN_POINT('Ctrl Pts',(9.70094164269938E-5,-0.0373235738184182,
-0.0141739374913336));
#42703=CARTESIAN_POINT('Ctrl Pts',(0.000138792623795986,-0.0373268192916294,
-0.0141714703469583));
#42704=CARTESIAN_POINT('Ctrl Pts',(0.00021500953180113,-0.0373328277511859,
-0.0141645649348134));
#42705=CARTESIAN_POINT('Ctrl Pts',(0.000249464513071551,-0.037335577192105,
-0.0141605372109731));
#42706=CARTESIAN_POINT('Ctrl Pts',(0.000327412140380952,-0.0373418825234562,
-0.0141493635626145));
#42707=CARTESIAN_POINT('Ctrl Pts',(0.000370806766784288,-0.0373454537936954,
-0.0141416720108122));
#42708=CARTESIAN_POINT('Ctrl Pts',(0.000522683727167805,-0.037358183766739,
-0.0141095448719654));
#42709=CARTESIAN_POINT('Ctrl Pts',(0.000629334272877263,-0.0373675572091138,
-0.0140775085577029));
#42710=CARTESIAN_POINT('Ctrl Pts',(0.000807103959575631,-0.0373838155596301,
-0.0140075104228064));
#42711=CARTESIAN_POINT('Ctrl Pts',(0.000879632852575996,-0.0373906408150592,
-0.0139738053109617));
#42712=CARTESIAN_POINT('Ctrl Pts',(0.000980096178100673,-0.0374002511035641,
-0.0139195805664092));
#42713=CARTESIAN_POINT('Ctrl Pts',(0.0010098187561663,-0.037403114511219,
-0.0139025378901922));
#42714=CARTESIAN_POINT('Ctrl Pts',(0.0010629075960811,-0.0374082493948992,
-0.0138702571393256));
#42715=CARTESIAN_POINT('Ctrl Pts',(0.0010864209962758,-0.0374105312083792,
-0.0138552777780935));
#42716=CARTESIAN_POINT('Ctrl Pts',(0.00112619627987677,-0.0374143948753308,
-0.0138287535047519));
#42717=CARTESIAN_POINT('Ctrl Pts',(0.00114261087437365,-0.0374159898217041,
-0.0138174493639702));
#42718=CARTESIAN_POINT('Ctrl Pts',(0.00118169433289094,-0.0374197897866691,
-0.013789663595829));
#42719=CARTESIAN_POINT('Ctrl Pts',(0.0012041905540118,-0.0374219802457077,
-0.0137729476962217));
#42720=CARTESIAN_POINT('Ctrl Pts',(0.001315479341029,-0.0374328750306482,
-0.0136865650922548));
#42721=CARTESIAN_POINT('Ctrl Pts',(0.00139862431276907,-0.0374412141337442,
-0.0136099358648364));
#42722=CARTESIAN_POINT('Ctrl Pts',(0.00155539022228087,-0.0374584130200933,
-0.0134387761293495));
#42723=CARTESIAN_POINT('Ctrl Pts',(0.00162788127348689,-0.0374672472908509,
-0.0133438476403939));
#42724=CARTESIAN_POINT('Ctrl Pts',(0.00171388313790786,-0.0374796158601278,
-0.0132075347606267));
#42725=CARTESIAN_POINT('Ctrl Pts',(0.00173515687398948,-0.0374828707101665,
-0.0131713392086822));
#42726=CARTESIAN_POINT('Ctrl Pts',(0.00177189728981138,-0.0374888878380479,
-0.0131040680357225));
#42727=CARTESIAN_POINT('Ctrl Pts',(0.00178772426159953,-0.0374916363163615,
-0.013073207338985));
#42728=CARTESIAN_POINT('Ctrl Pts',(0.00182175300593214,-0.0374979275150254,
-0.0130023783042651));
#42729=CARTESIAN_POINT('Ctrl Pts',(0.00183945604787153,-0.0375014853212653,
-0.0129621919344909));
#42730=CARTESIAN_POINT('Ctrl Pts',(0.00190066855119462,-0.0375149470228309,
-0.0128098332313055));
#42731=CARTESIAN_POINT('Ctrl Pts',(0.00193534634612376,-0.0375251119061988,
-0.0126944064368557));
#42732=CARTESIAN_POINT('Ctrl Pts',(0.00197428570357736,-0.0375416613458246,
-0.0125040054806906));
#42733=CARTESIAN_POINT('Ctrl Pts',(0.00198508546783883,-0.0375479808965758,
-0.0124306560179852));
#42734=CARTESIAN_POINT('Ctrl Pts',(0.00199477796909831,-0.037556984851982,
-0.0123240083659955));
#42735=CARTESIAN_POINT('Ctrl Pts',(0.00199695119287043,-0.0375597399821034,
-0.0122910716876289));
#42736=CARTESIAN_POINT('Ctrl Pts',(0.00199942492100401,-0.0375647061858646,
-0.012230964590769));
#42737=CARTESIAN_POINT('Ctrl Pts',(0.0019999889362052,-0.0375669266170007,
-0.0122038128945948));
#42738=CARTESIAN_POINT('Ctrl Pts',(0.00200000784605045,-0.0375707300545887,
-0.0121567109876418));
#42739=CARTESIAN_POINT('Ctrl Pts',(0.00199971752824393,-0.0375723246956571,
-0.0121367673907308));
#42740=CARTESIAN_POINT('Ctrl Pts',(0.00199827865261496,-0.0375761848052306,
-0.012088033542739));
#42741=CARTESIAN_POINT('Ctrl Pts',(0.00199680636677368,-0.0375784340739312,
-0.0120592579837219));
#42742=CARTESIAN_POINT('Ctrl Pts',(0.00198863664519388,-0.0375871173561157,
-0.0119471261388361));
#42743=CARTESIAN_POINT('Ctrl Pts',(0.00197733578988694,-0.0375933658567144,
-0.0118641832568899));
#42744=CARTESIAN_POINT('Ctrl Pts',(0.00193199160779409,-0.0376104764635744,
-0.0116383236231266));
#42745=CARTESIAN_POINT('Ctrl Pts',(0.00188737037779793,-0.037621240369542,
-0.0114980939080775));
#42746=CARTESIAN_POINT('Ctrl Pts',(0.00181076746343494,-0.0376357217226709,
-0.011325626688677));
#42747=CARTESIAN_POINT('Ctrl Pts',(0.00179251476470957,-0.0376389783127346,
-0.011287791117484));
#42748=CARTESIAN_POINT('Ctrl Pts',(0.00175719588939473,-0.0376449710021385,
-0.0112201115652511));
#42749=CARTESIAN_POINT('Ctrl Pts',(0.00174052526988488,-0.0376476927582319,
-0.0111900789058641));
#42750=CARTESIAN_POINT('Ctrl Pts',(0.00170053544453039,-0.0376539978464694,
-0.0111222152772039));
#42751=CARTESIAN_POINT('Ctrl Pts',(0.00167671293918052,-0.0376575978266976,
-0.011084703914326));
#42752=CARTESIAN_POINT('Ctrl Pts',(0.0015976780758644,-0.0376690892594782,
-0.0109689608135697));
#42753=CARTESIAN_POINT('Ctrl Pts',(0.00153809393351182,-0.0376771270225727,
-0.0108938911192655));
#42754=CARTESIAN_POINT('Ctrl Pts',(0.0013871396130019,-0.0376960811339597,
-0.0107294421765821));
#42755=CARTESIAN_POINT('Ctrl Pts',(0.00129211542301816,-0.0377070332348158,
-0.010643958141956));
#42756=CARTESIAN_POINT('Ctrl Pts',(0.00116628818021785,-0.0377199898750456,
-0.0105508571697274));
#42757=CARTESIAN_POINT('Ctrl Pts',(0.00114260872823566,-0.0377223667357724,
-0.0105341206508794));
#42758=CARTESIAN_POINT('Ctrl Pts',(0.00110203233628788,-0.0377263271991535,
-0.0105067448989099));
#42759=CARTESIAN_POINT('Ctrl Pts',(0.00108532655081619,-0.0377279261293796,
-0.010495834097586));
#42760=CARTESIAN_POINT('Ctrl Pts',(0.00104563437170556,-0.0377316514175624,
-0.0104707498530013));
#42761=CARTESIAN_POINT('Ctrl Pts',(0.00102251944689131,-0.0377337653641723,
-0.0104567886714004));
#42762=CARTESIAN_POINT('Ctrl Pts',(0.000913135513759129,-0.0377435476955092,
-0.010393709286691));
#42763=CARTESIAN_POINT('Ctrl Pts',(0.000823559401920711,-0.0377509308597381,
-0.0103505837734056));
#42764=CARTESIAN_POINT('Ctrl Pts',(0.000609913314534462,-0.0377679524822781,
-0.0102666731944105));
#42765=CARTESIAN_POINT('Ctrl Pts',(0.000484338160591787,-0.0377775499413346,
-0.0102310203974994));
#42766=CARTESIAN_POINT('Ctrl Pts',(0.00031318480157617,-0.0377908652199709,
-0.010200043121726));
#42767=CARTESIAN_POINT('Ctrl Pts',(0.000269933614756223,-0.0377942468263184,
-0.0101936711953994));
#42768=CARTESIAN_POINT('Ctrl Pts',(0.000192081988798559,-0.0378003870508134,
-0.0101847969620219));
#42769=CARTESIAN_POINT('Ctrl Pts',(0.000157558763748098,-0.0378031284829236,
-0.0101817681027072));
#42770=CARTESIAN_POINT('Ctrl Pts',(8.02601991222002E-5,-0.0378093178668174,
-0.0101770061458459));
#42771=CARTESIAN_POINT('Ctrl Pts',(3.74741157882117E-5,-0.037812778840363,
-0.0101757466079817));
#42772=CARTESIAN_POINT('Ctrl Pts',(-0.000119439652899614,-0.0378256156577653,
-0.010176163712007));
#42773=CARTESIAN_POINT('Ctrl Pts',(-0.000233309468688445,-0.0378352265053964,
-0.010186234454147));
#42774=CARTESIAN_POINT('Ctrl Pts',(-0.000460272407019546,-0.037854832108227,
-0.0102260623594481));
#42775=CARTESIAN_POINT('Ctrl Pts',(-0.000572898115018368,-0.0378647928096336,
-0.0102561326654076));
#42776=CARTESIAN_POINT('Ctrl Pts',(-0.000708305517464874,-0.0378766942117564,
-0.0103052731690095));
#42777=CARTESIAN_POINT('Ctrl Pts',(-0.000734136555291568,-0.0378789602662475,
-0.0103152591807939));
#42778=CARTESIAN_POINT('Ctrl Pts',(-0.000778190739800792,-0.0378828082752215,
-0.0103333505260722));
#42779=CARTESIAN_POINT('Ctrl Pts',(-0.000796513180758882,-0.0378844029495056,
-0.0103411968884309));
#42780=CARTESIAN_POINT('Ctrl Pts',(-0.000840483662182668,-0.0378882173428055,
-0.0103608097132594));
#42781=CARTESIAN_POINT('Ctrl Pts',(-0.00086600533456494,-0.0378904221027663,
-0.010372847197548));
#42782=CARTESIAN_POINT('Ctrl Pts',(-0.000922462327936118,-0.0378952976082513,
-0.0104009511326673));
#42783=CARTESIAN_POINT('Ctrl Pts',(-0.000953249933725808,-0.0378979552284288,
-0.0104172944203574));
#42784=CARTESIAN_POINT('Ctrl Pts',(-0.00105570219694375,-0.0379068484286634,
-0.0104751620232309));
#42785=CARTESIAN_POINT('Ctrl Pts',(-0.00112521300116565,-0.0379129685014775,
-0.0105203306333061));
#42786=CARTESIAN_POINT('Ctrl Pts',(-0.00127779940184788,-0.0379270488797308,
-0.0106335447107695));
#42787=CARTESIAN_POINT('Ctrl Pts',(-0.00135859092995394,-0.0379350038016011,
-0.0107042166929915));
#42788=CARTESIAN_POINT('Ctrl Pts',(-0.00146399011277126,-0.0379465622199433,
-0.0108125242863669));
#42789=CARTESIAN_POINT('Ctrl Pts',(-0.001493603242113,-0.0379499603303875,
-0.0108450333008675));
#42790=CARTESIAN_POINT('Ctrl Pts',(-0.00154461631564727,-0.0379561171799667,
-0.0109048838850407));
#42791=CARTESIAN_POINT('Ctrl Pts',(-0.00156642154377424,-0.0379588583090676,
-0.010931857291425));
#42792=CARTESIAN_POINT('Ctrl Pts',(-0.00161301394457054,-0.0379649747119398,
-0.0109926610896534));
#42793=CARTESIAN_POINT('Ctrl Pts',(-0.00163745984551324,-0.0379683613307496,
-0.0110267307994885));
#42794=CARTESIAN_POINT('Ctrl Pts',(-0.00172650473410387,-0.0379814189809069,
-0.0111594468537029));
#42795=CARTESIAN_POINT('Ctrl Pts',(-0.00178339720749385,-0.0379913478302212,
-0.011262953321342));
#42796=CARTESIAN_POINT('Ctrl Pts',(-0.00187701245352657,-0.0380111392656663,
-0.0114758642272042));
#42797=CARTESIAN_POINT('Ctrl Pts',(-0.00191406948471588,-0.0380209576811575,
-0.0115846658969556));
#42798=CARTESIAN_POINT('Ctrl Pts',(-0.00194827554810133,-0.0380327409405725,
-0.0117230863763989));
#42799=CARTESIAN_POINT('Ctrl Pts',(-0.00195439133817699,-0.0380350204854707,
-0.0117502593335966));
#42800=CARTESIAN_POINT('Ctrl Pts',(-0.00196390691663225,-0.0380388818505571,
-0.0117970831734445));
#42801=CARTESIAN_POINT('Ctrl Pts',(-0.00196758365527947,-0.0380404767110245,
-0.0118166711122663));
#42802=CARTESIAN_POINT('Ctrl Pts',(-0.00197572896531307,-0.0380442785245321,
-0.0118639531783277));
#42803=CARTESIAN_POINT('Ctrl Pts',(-0.0019799088898604,-0.0380464708642459,
-0.0118916919884722));
#42804=CARTESIAN_POINT('Ctrl Pts',(-0.00199605023909678,-0.0380562095646285,
-0.0120165894677957));
#42805=CARTESIAN_POINT('Ctrl Pts',(-0.00200145408979447,-0.0380634870219811,
-0.0121144701986351));
#42806=CARTESIAN_POINT('Ctrl Pts',(-0.00199731153593474,-0.0380803134791257,
-0.0123413561098355));
#42807=CARTESIAN_POINT('Ctrl Pts',(-0.00198248144568392,-0.0380898236921549,
-0.0124698047553217));
#42808=CARTESIAN_POINT('Ctrl Pts',(-0.00194618537572517,-0.0381030510275557,
-0.0126387593561005));
#42809=CARTESIAN_POINT('Ctrl Pts',(-0.00193557881838683,-0.0381064401727976,
-0.0126812775162492));
#42810=CARTESIAN_POINT('Ctrl Pts',(-0.00191409822173182,-0.0381125879388726,
-0.0127567395422326));
#42811=CARTESIAN_POINT('Ctrl Pts',(-0.00190374692082494,-0.0381153291720509,
-0.0127898143704626));
#42812=CARTESIAN_POINT('Ctrl Pts',(-0.00187873404632049,-0.0381215103173969,
-0.0128630080940655));
#42813=CARTESIAN_POINT('Ctrl Pts',(-0.00186363639818402,-0.0381249630681109,
-0.0129029586219866));
#42814=CARTESIAN_POINT('Ctrl Pts',(-0.00180216363623665,-0.0381380824302724,
-0.0130511010363636));
#42815=CARTESIAN_POINT('Ctrl Pts',(-0.00174755377819325,-0.0381480026027225,
-0.0131555979925288));
#42816=CARTESIAN_POINT('Ctrl Pts',(-0.00162358878327254,-0.0381675624529433,
-0.0133491130223898));
#42817=CARTESIAN_POINT('Ctrl Pts',(-0.00155524949633392,-0.0381771562219628,
-0.0134383040426665));
#42818=CARTESIAN_POINT('Ctrl Pts',(-0.00146089134015479,-0.0381887517609584,
-0.0135420836852323));
#42819=CARTESIAN_POINT('Ctrl Pts',(-0.00144155781384415,-0.0381910518695265,
-0.0135624679820263));
#42820=CARTESIAN_POINT('Ctrl Pts',(-0.00140778240823205,-0.0381949339587745,
-0.0135966086989769));
#42821=CARTESIAN_POINT('Ctrl Pts',(-0.00139355415013042,-0.0381965294619312,
-0.0136105672596134));
#42822=CARTESIAN_POINT('Ctrl Pts',(-0.00135897495918084,-0.0382003139014703,
-0.0136434910454913));
#42823=CARTESIAN_POINT('Ctrl Pts',(-0.00133843302066023,-0.0382024887189372,
-0.0136622485263724));
#42824=CARTESIAN_POINT('Ctrl Pts',(-0.00129181546836941,-0.0382072821999684,
-0.0137030660070713));
#42825=CARTESIAN_POINT('Ctrl Pts',(-0.00126555243225979,-0.0382098884490764,
-0.0137248992007725));
#42826=CARTESIAN_POINT('Ctrl Pts',(-0.00117642234843681,-0.0382184761592371,
-0.0137952146576192));
#42827=CARTESIAN_POINT('Ctrl Pts',(-0.00111122759664908,-0.038224350204512,
-0.0138406282217031));
#42828=CARTESIAN_POINT('Ctrl Pts',(-0.000948034191794875,-0.0382385254756857,
-0.0139404366672938));
#42829=CARTESIAN_POINT('Ctrl Pts',(-0.000847843732767766,-0.0382468178552304,
-0.0139907033234199));
#42830=CARTESIAN_POINT('Ctrl Pts',(-0.000703072476874712,-0.0382587446283123,
-0.0140487204686366));
#42831=CARTESIAN_POINT('Ctrl Pts',(-0.000661635084892373,-0.0382621505658226,
-0.0140637571153293));
#42832=CARTESIAN_POINT('Ctrl Pts',(-0.00058675622901919,-0.0382683157921436,
-0.0140881609082087));
#42833=CARTESIAN_POINT('Ctrl Pts',(-0.000553502921073503,-0.0382710572738542,
-0.0140980493054214));
#42834=CARTESIAN_POINT('Ctrl Pts',(-0.000479603364999026,-0.0382771674742592,
-0.014117947979369));
#42835=CARTESIAN_POINT('Ctrl Pts',(-0.000438867166580089,-0.0382805473791945,
-0.0141275567149277));
#42836=CARTESIAN_POINT('Ctrl Pts',(-0.00028081590054678,-0.0382937222060191,
-0.0141596392710825));
#42837=CARTESIAN_POINT('Ctrl Pts',(-0.000161895817778599,-0.03830378332686,
-0.0141728623356128));
#42838=CARTESIAN_POINT('Ctrl Pts',(7.05325538605727E-5,-0.0383235685854632,
-0.0141778056755301));
#42839=CARTESIAN_POINT('Ctrl Pts',(0.000183600635649123,-0.0383332437427695,
-0.0141706171883384));
#42840=CARTESIAN_POINT('Ctrl Pts',(0.000323159407938675,-0.038344907592274,
-0.0141497712793331));
#42841=CARTESIAN_POINT('Ctrl Pts',(0.000350768658249815,-0.0383472004703621,
-0.0141450525720751));
#42842=CARTESIAN_POINT('Ctrl Pts',(0.000397840836073238,-0.0383510751404662,
-0.0141359858915574));
#42843=CARTESIAN_POINT('Ctrl Pts',(0.000417352300280133,-0.0383526702886812,
-0.0141319244302668));
#42844=CARTESIAN_POINT('Ctrl Pts',(0.000464017986272079,-0.0383564602177103,
-0.0141214804571578));
#42845=CARTESIAN_POINT('Ctrl Pts',(0.000491105055873706,-0.0383586407149533,
-0.0141148204943532));
#42846=CARTESIAN_POINT('Ctrl Pts',(0.000551156226446959,-0.0383634498457881,
-0.0140987162431857));
#42847=CARTESIAN_POINT('Ctrl Pts',(0.000584034979678977,-0.0383660659261672,
-0.0140889864722992));
#42848=CARTESIAN_POINT('Ctrl Pts',(0.000692782076354716,-0.0383747117753444,
-0.0140537398831911));
#42849=CARTESIAN_POINT('Ctrl Pts',(0.000767369744519523,-0.0383806325754964,
-0.0140245150544803));
#42850=CARTESIAN_POINT('Ctrl Pts',(0.000940729463619783,-0.0383947875991112,
-0.0139442835154794));
#42851=CARTESIAN_POINT('Ctrl Pts',(0.00103738482507462,-0.0384030139209357,
-0.0138893720281325));
#42852=CARTESIAN_POINT('Ctrl Pts',(0.00116535119373253,-0.0384148691110817,
-0.0138018600371267));
#42853=CARTESIAN_POINT('Ctrl Pts',(0.00120088617449846,-0.03841827413626,
-0.0137757949156857));
#42854=CARTESIAN_POINT('Ctrl Pts',(0.00126280191070961,-0.0384244379026909,
-0.013727154089493));
#42855=CARTESIAN_POINT('Ctrl Pts',(0.00128951092926202,-0.038427178847001,
-0.013705024341986));
#42856=CARTESIAN_POINT('Ctrl Pts',(0.00134714257232176,-0.0384332879193722,
-0.0136546898122304));
#42857=CARTESIAN_POINT('Ctrl Pts',(0.00137778161647662,-0.0384366672335894,
-0.0136261869984806));
#42858=CARTESIAN_POINT('Ctrl Pts',(0.00144068024534243,-0.0384438997234916,
-0.0135638811471868));
#42859=CARTESIAN_POINT('Ctrl Pts',(0.00147269431986616,-0.0384477601675629,
-0.0135298664699847));
#42860=CARTESIAN_POINT('Ctrl Pts',(0.00156554601470379,-0.0384595163259991,
-0.0134240206792137));
#42861=CARTESIAN_POINT('Ctrl Pts',(0.0016225300483719,-0.0384675211216179,
-0.0133489899076143));
#42862=CARTESIAN_POINT('Ctrl Pts',(0.00172320968516587,-0.0384831932744022,
-0.0131949856253024));
#42863=CARTESIAN_POINT('Ctrl Pts',(0.00176727787477499,-0.0384908413644903,
-0.0131164988831206));
#42864=CARTESIAN_POINT('Ctrl Pts',(0.00181829914083528,-0.0385006670117318,
-0.0130092909552669));
#42865=CARTESIAN_POINT('Ctrl Pts',(0.00183011762917312,-0.0385030286043635,
-0.0129830086783471));
#42866=CARTESIAN_POINT('Ctrl Pts',(0.00184914858536509,-0.0385069730492785,
-0.0129381178088366));
#42867=CARTESIAN_POINT('Ctrl Pts',(0.00185665728260757,-0.038508570877622,
-0.0129196419273955));
#42868=CARTESIAN_POINT('Ctrl Pts',(0.00187373007036264,-0.0385123058288285,
-0.0128757619656744));
#42869=CARTESIAN_POINT('Ctrl Pts',(0.00188305564672636,-0.0385144302377396,
-0.0128502702064181));
#42870=CARTESIAN_POINT('Ctrl Pts',(0.00190255726831701,-0.0385190867654835,
-0.012793399565067));
#42871=CARTESIAN_POINT('Ctrl Pts',(0.00191248194411514,-0.0385216076079525,
-0.0127619425805678));
#42872=CARTESIAN_POINT('Ctrl Pts',(0.00194213069085138,-0.0385297100461789,
-0.0126591759170012));
#42873=CARTESIAN_POINT('Ctrl Pts',(0.00195867880380338,-0.0385351965342661,
-0.0125870115839811));
#42874=CARTESIAN_POINT('Ctrl Pts',(0.00199157150403463,-0.0385496109676425,
-0.0123953192453778));
#42875=CARTESIAN_POINT('Ctrl Pts',(0.00200117372027142,-0.0385585161049327,
-0.0122749595176973));
#42876=CARTESIAN_POINT('Ctrl Pts',(0.00199941647148352,-0.0385710900101807,
-0.0121105772634695));
#42877=CARTESIAN_POINT('Ctrl Pts',(0.0019975020771425,-0.0385744832550496,
-0.0120667106936694));
#42878=CARTESIAN_POINT('Ctrl Pts',(0.00199149496027503,-0.0385806350369663,
-0.0119883689046225));
#42879=CARTESIAN_POINT('Ctrl Pts',(0.00198794502271778,-0.0385833760892058,
-0.011953869360343));
#42880=CARTESIAN_POINT('Ctrl Pts',(0.00197811920335749,-0.0385894968676683,
-0.0118778488280213));
#42881=CARTESIAN_POINT('Ctrl Pts',(0.00197142908283395,-0.0385928880427132,
-0.0118363991877451));
#42882=CARTESIAN_POINT('Ctrl Pts',(0.0019407326261264,-0.0386060660318903,
-0.0116780670179382));
#42883=CARTESIAN_POINT('Ctrl Pts',(0.00190759372731417,-0.0386161178177868,
-0.011563226552101));
#42884=CARTESIAN_POINT('Ctrl Pts',(0.00182363663131297,-0.0386358613029376,
-0.0113469658975532));
#42885=CARTESIAN_POINT('Ctrl Pts',(0.00177403136633091,-0.0386455040279907,
-0.011245519170315));
#42886=CARTESIAN_POINT('Ctrl Pts',(0.00170174007060536,-0.038657140703491,
-0.0111247267953279));
#42887=CARTESIAN_POINT('Ctrl Pts',(0.00168683581550337,-0.0386594364849881,
-0.0111009712775625));
#42888=CARTESIAN_POINT('Ctrl Pts',(0.00166048637217388,-0.0386633148367904,
-0.0110608723201784));
#42889=CARTESIAN_POINT('Ctrl Pts',(0.00164928853731533,-0.0386649108110946,
-0.0110443741793974));
#42890=CARTESIAN_POINT('Ctrl Pts',(0.00162183762097585,-0.0386687017917325,
-0.011005203628449));
#42891=CARTESIAN_POINT('Ctrl Pts',(0.00160535380731262,-0.0386708825337648,
-0.0109826989485342));
#42892=CARTESIAN_POINT('Ctrl Pts',(0.00152853376919155,-0.0386806617268341,
-0.0108822954586132));
#42893=CARTESIAN_POINT('Ctrl Pts',(0.00146295583648381,-0.0386879864424875,
-0.0108085667429993));
#42894=CARTESIAN_POINT('Ctrl Pts',(0.00129992593189615,-0.0387048253973154,
-0.0106504969271482));
#42895=CARTESIAN_POINT('Ctrl Pts',(0.00119925030815946,-0.0387143018343294,
-0.0105701404332164));
#42896=CARTESIAN_POINT('Ctrl Pts',(0.00105482590507667,-0.0387274947805248,
-0.0104760694790257));
#42897=CARTESIAN_POINT('Ctrl Pts',(0.00101730987124912,-0.0387308866944521,
-0.0104533542950851));
#42898=CARTESIAN_POINT('Ctrl Pts',(0.000948848476877909,-0.0387370386136422,
-0.0104149192761649));
#42899=CARTESIAN_POINT('Ctrl Pts',(0.000918182503645546,-0.0387397811943162,
-0.0103987369095612));
#42900=CARTESIAN_POINT('Ctrl Pts',(0.000848831002929154,-0.0387459647772771,
-0.0103644145171097));
#42901=CARTESIAN_POINT('Ctrl Pts',(0.000809954729837285,-0.038749418609445,
-0.0103467012235863));
#42902=CARTESIAN_POINT('Ctrl Pts',(0.000656348837988446,-0.0387630341016132,
-0.0102825704688347));
#42903=CARTESIAN_POINT('Ctrl Pts',(0.000537993840605165,-0.0387734815002861,
-0.0102456028975493));
#42904=CARTESIAN_POINT('Ctrl Pts',(0.000314162457675591,-0.038792969085903,
-0.0101978848996542));
#42905=CARTESIAN_POINT('Ctrl Pts',(0.000209744086835203,-0.0388019493781763,
-0.0101841032912974));
#42906=CARTESIAN_POINT('Ctrl Pts',(7.62098950558415E-5,-0.0388130110308991,
-0.0101771019148088));
#42907=CARTESIAN_POINT('Ctrl Pts',(4.76700322510099E-5,-0.0388153501473621,
-0.0101762176181587));
#42908=CARTESIAN_POINT('Ctrl Pts',(-8.0978828752807E-7,-0.0388192710984081,
-0.0101757541551425));
#42909=CARTESIAN_POINT('Ctrl Pts',(-2.07402249733232E-5,-0.0388208673944913,
-0.010175861500156));
#42910=CARTESIAN_POINT('Ctrl Pts',(-6.80134958519161E-5,-0.0388246169837417,
-0.0101768229667554));
#42911=CARTESIAN_POINT('Ctrl Pts',(-9.53461652196843E-5,-0.0388267571028226,
-0.0101779400294083));
#42912=CARTESIAN_POINT('Ctrl Pts',(-0.00021910429435872,-0.0388363563210289,
-0.0101855437635411));
#42913=CARTESIAN_POINT('Ctrl Pts',(-0.000315015879592685,-0.0388435486839813,
-0.010198453860677));
#42914=CARTESIAN_POINT('Ctrl Pts',(-0.000539503968791133,-0.0388605581307301,
-0.0102454280303853));
#42915=CARTESIAN_POINT('Ctrl Pts',(-0.000666339487880301,-0.0388703281950098,
-0.0102854582655062));
#42916=CARTESIAN_POINT('Ctrl Pts',(-0.000828230377753176,-0.0388838160644624,
-0.0103548851839165));
#42917=CARTESIAN_POINT('Ctrl Pts',(-0.000867617073926069,-0.038887180490065,
-0.0103733188261862));
#42918=CARTESIAN_POINT('Ctrl Pts',(-0.000937227764646918,-0.0388933008146155,
-0.0104087079959825));
#42919=CARTESIAN_POINT('Ctrl Pts',(-0.000967671728618498,-0.0388960399147139,
-0.0104251935556203));
#42920=CARTESIAN_POINT('Ctrl Pts',(-0.00103487342660241,-0.0389022376515323,
-0.0104638721203979));
#42921=CARTESIAN_POINT('Ctrl Pts',(-0.00107137402146666,-0.0389057096215286,
-0.0104864748012229));
#42922=CARTESIAN_POINT('Ctrl Pts',(-0.00114756650722974,-0.0389131957874466,
-0.0105371189615908));
#42923=CARTESIAN_POINT('Ctrl Pts',(-0.00118702022961977,-0.0389172188178244,
-0.0105654678260557));
#42924=CARTESIAN_POINT('Ctrl Pts',(-0.00130710441675965,-0.0389299311215999,
-0.0106585643158108));
#42925=CARTESIAN_POINT('Ctrl Pts',(-0.00138376868745635,-0.0389387523314952,
-0.0107281417222787));
#42926=CARTESIAN_POINT('Ctrl Pts',(-0.00151106740732872,-0.0389545389278394,
-0.0108630621805033));
#42927=CARTESIAN_POINT('Ctrl Pts',(-0.0015637026512866,-0.0389614957662427,
-0.0109262205302713));
#42928=CARTESIAN_POINT('Ctrl Pts',(-0.00162747895202746,-0.038970375950535,
-0.0110131110317425));
#42929=CARTESIAN_POINT('Ctrl Pts',(-0.00164225117205757,-0.0389724687551532,
-0.0110340702234264));
#42930=CARTESIAN_POINT('Ctrl Pts',(-0.00166771936987987,-0.0389761347155219,
-0.011071722515502));
#42931=CARTESIAN_POINT('Ctrl Pts',(-0.0016785763962559,-0.0389777167945088,
-0.0110882991468602));
#42932=CARTESIAN_POINT('Ctrl Pts',(-0.00170521428469145,-0.0389816512994129,
-0.0111303197582263));
#42933=CARTESIAN_POINT('Ctrl Pts',(-0.00172067341628377,-0.038983984867415,
-0.0111559614363426));
#42934=CARTESIAN_POINT('Ctrl Pts',(-0.00175440504553163,-0.0389892178713042,
-0.0112148631019774));
#42935=CARTESIAN_POINT('Ctrl Pts',(-0.00177231872958831,-0.0389921008736996,
-0.0112483157364037));
#42936=CARTESIAN_POINT('Ctrl Pts',(-0.00183384494869554,-0.0390024734347505,
-0.0113715116800154));
#42937=CARTESIAN_POINT('Ctrl Pts',(-0.00187168042820106,-0.0390098052098159,
-0.011463977560093));
#42938=CARTESIAN_POINT('Ctrl Pts',(-0.00193185239169798,-0.039024293295583,
-0.0116495213394445));
#42939=CARTESIAN_POINT('Ctrl Pts',(-0.00195472805560331,-0.0390314244176959,
-0.0117421322785678));
#42940=CARTESIAN_POINT('Ctrl Pts',(-0.00197779129677471,-0.0390418652493989,
-0.0118758884714093));
#42941=CARTESIAN_POINT('Ctrl Pts',(-0.00198345468803974,-0.039045009713617,
-0.0119159602858768));
#42942=CARTESIAN_POINT('Ctrl Pts',(-0.0019917244849381,-0.0390509306214746,
-0.0119907943745484));
#42943=CARTESIAN_POINT('Ctrl Pts',(-0.00199464504219202,-0.0390536963278605,
-0.0120255067525328));
#42944=CARTESIAN_POINT('Ctrl Pts',(-0.00199937083401339,-0.039060255758042,
-0.012107146991131));
#42945=CARTESIAN_POINT('Ctrl Pts',(-0.00200043248984103,-0.0390640703900177,
-0.012154095191338));
#42946=CARTESIAN_POINT('Ctrl Pts',(-0.00199914063173659,-0.0390725095052458,
-0.0122566957420391));
#42947=CARTESIAN_POINT('Ctrl Pts',(-0.00199611627667757,-0.0390771493744292,
-0.0123122995149277));
#42948=CARTESIAN_POINT('Ctrl Pts',(-0.0019761031886314,-0.0390947112710543,
-0.0125199732177311));
#42949=CARTESIAN_POINT('Ctrl Pts',(-0.00194400827975716,-0.0391079186545807,
-0.0126700523661867));
#42950=CARTESIAN_POINT('Ctrl Pts',(-0.00188450618699411,-0.0391234094647331,
-0.0128464797337211));
#42951=CARTESIAN_POINT('Ctrl Pts',(-0.00187310730703759,-0.0391261459905812,
-0.0128776885765298));
#42952=CARTESIAN_POINT('Ctrl Pts',(-0.00185354202130938,-0.0391304824674267,
-0.0129273778656509));
#42953=CARTESIAN_POINT('Ctrl Pts',(-0.00184586449283688,-0.0391321063495913,
-0.0129460426449891));
#42954=CARTESIAN_POINT('Ctrl Pts',(-0.00182824197818174,-0.0391356649585445,
-0.0129871063988338));
#42955=CARTESIAN_POINT('Ctrl Pts',(-0.00181816558567162,-0.0391375924958856,
-0.0130094445599979));
#42956=CARTESIAN_POINT('Ctrl Pts',(-0.00178035220529878,-0.0391444751045524,
-0.0130893222113692));
#42957=CARTESIAN_POINT('Ctrl Pts',(-0.00175027099708755,-0.0391493157868255,
-0.0131457155108037));
#42958=CARTESIAN_POINT('Ctrl Pts',(-0.00163858331329163,-0.0391656487626147,
-0.0133329149747651));
#42959=CARTESIAN_POINT('Ctrl Pts',(-0.00154460123708137,-0.0391768630169473,
-0.0134556791309526));
#42960=CARTESIAN_POINT('Ctrl Pts',(-0.00140203440492122,-0.0391924390950184,
-0.01360305156302));
#42961=CARTESIAN_POINT('Ctrl Pts',(-0.00136522964147225,-0.0391963522425618,
-0.0136382973499277));
#42962=CARTESIAN_POINT('Ctrl Pts',(-0.00130069999596002,-0.0392030762145198,
-0.0136955331519979));
#42963=CARTESIAN_POINT('Ctrl Pts',(-0.00127366327754493,-0.0392058557164568,
-0.0137182633888239));
#42964=CARTESIAN_POINT('Ctrl Pts',(-0.00121565059777392,-0.039211753309896,
-0.0137644700040737));
#42965=CARTESIAN_POINT('Ctrl Pts',(-0.00118456401256669,-0.0392148761858583,
-0.0137877829167457));
#42966=CARTESIAN_POINT('Ctrl Pts',(-0.00108865866217099,-0.0392244125808423,
-0.0138554328099652));
#42967=CARTESIAN_POINT('Ctrl Pts',(-0.00102189614895441,-0.0392309245681077,
-0.0138968676099053));
#42968=CARTESIAN_POINT('Ctrl Pts',(-0.000821271249900922,-0.0392501283527807,
-0.0140055856613206));
#42969=CARTESIAN_POINT('Ctrl Pts',(-0.000682079727168703,-0.03926304420327,
-0.0140619000518252));
#42970=CARTESIAN_POINT('Ctrl Pts',(-0.000503581911005871,-0.039278502301198,
-0.0141117447326403));
#42971=CARTESIAN_POINT('Ctrl Pts',(-0.000468999049084978,-0.039281445824025,
-0.0141204125555864));
#42972=CARTESIAN_POINT('Ctrl Pts',(-0.000416004516991219,-0.0392858619195975,
-0.0141321987829423));
#42973=CARTESIAN_POINT('Ctrl Pts',(-0.000397751866308258,-0.0392873660366728,
-0.0141359912947632));
#42974=CARTESIAN_POINT('Ctrl Pts',(-0.000357560853455187,-0.0392906373508532,
-0.0141437575398385));
#42975=CARTESIAN_POINT('Ctrl Pts',(-0.000335603531156165,-0.0392923984221514,
-0.0141476208476875));
#42976=CARTESIAN_POINT('Ctrl Pts',(-0.000267570151130193,-0.0392977876116455,
-0.0141584215510888));
#42977=CARTESIAN_POINT('Ctrl Pts',(-0.000221309693191029,-0.0393013572144864,
-0.0141641172492253));
#42978=CARTESIAN_POINT('Ctrl Pts',(-9.88980477596605E-5,-0.0393106544945962,
-0.0141748625823675));
#42979=CARTESIAN_POINT('Ctrl Pts',(-2.25835548107882E-5,-0.0393163019321686,
-0.0141771804639402));
#42980=CARTESIAN_POINT('Ctrl Pts',(0.000170954832808541,-0.0393306361910164,
-0.0141719839168146));
#42981=CARTESIAN_POINT('Ctrl Pts',(0.000287712108264512,-0.0393393069220895,
-0.0141585234126676));
#42982=CARTESIAN_POINT('Ctrl Pts',(0.000445635672679678,-0.0393516298942125,
-0.0141260682093816));
#42983=CARTESIAN_POINT('Ctrl Pts',(0.000488355158622234,-0.0393550229659414,
-0.0141158115596219));
#42984=CARTESIAN_POINT('Ctrl Pts',(0.000563917641588812,-0.0393611558751002,
-0.0140950155808122));
#42985=CARTESIAN_POINT('Ctrl Pts',(0.000596891768233525,-0.0393638777338799,
-0.0140850172254602));
#42986=CARTESIAN_POINT('Ctrl Pts',(0.000668837126536266,-0.0393699272511997,
-0.0140611561073833));
#42987=CARTESIAN_POINT('Ctrl Pts',(0.000707668701079003,-0.0393732656475689,
-0.0140469263291254));
#42988=CARTESIAN_POINT('Ctrl Pts',(0.000858546179152205,-0.0393865441104755,
-0.0139862689568736));
#42989=CARTESIAN_POINT('Ctrl Pts',(0.000966697141236107,-0.0393967639454479,
-0.013930901308442));
#42990=CARTESIAN_POINT('Ctrl Pts',(0.0011637925083519,-0.0394166207138157,
-0.0138062298084821));
#42991=CARTESIAN_POINT('Ctrl Pts',(0.00125324523339048,-0.0394262037351952,
-0.0137385179806201));
#42992=CARTESIAN_POINT('Ctrl Pts',(0.0013574102062589,-0.0394377832544203,
-0.0136449423714233));
#42993=CARTESIAN_POINT('Ctrl Pts',(0.00137786138051014,-0.0394400785240584,
-0.0136257786146584));
#42994=CARTESIAN_POINT('Ctrl Pts',(0.00141211123224659,-0.0394439509147715,
-0.0135923053619283));
#42995=CARTESIAN_POINT('Ctrl Pts',(0.00142611010389813,-0.0394455415596819,
-0.0135782101187051));
#42996=CARTESIAN_POINT('Ctrl Pts',(0.00145907054647678,-0.0394493070334893,
-0.0135440185682288));
#42997=CARTESIAN_POINT('Ctrl Pts',(0.00147782980878293,-0.0394514680107137,
-0.0135237339854722));
#42998=CARTESIAN_POINT('Ctrl Pts',(0.00151858969053321,-0.0394562217629058,
-0.0134777854478266));
#42999=CARTESIAN_POINT('Ctrl Pts',(0.0015403724221204,-0.0394588024886933,
-0.0134519391380417));
#43000=CARTESIAN_POINT('Ctrl Pts',(0.00160992706431918,-0.039467226826154,
-0.013365031001043));
#43001=CARTESIAN_POINT('Ctrl Pts',(0.00165480677781664,-0.0394729671599579,
-0.0133017417542357));
#43002=CARTESIAN_POINT('Ctrl Pts',(0.00175738242048589,-0.0394873042258206,
-0.0131376534881175));
#43003=CARTESIAN_POINT('Ctrl Pts',(0.00181018557107691,-0.0394958875859548,
-0.0130341521249923));
#43004=CARTESIAN_POINT('Ctrl Pts',(0.00187034280351365,-0.0395081420186117,
-0.012885626680233));
#43005=CARTESIAN_POINT('Ctrl Pts',(0.00188559610556518,-0.0395115639560029,
-0.0128440503054837));
#43006=CARTESIAN_POINT('Ctrl Pts',(0.00191036306444168,-0.039517757296807,
-0.0127689187199605));
#43007=CARTESIAN_POINT('Ctrl Pts',(0.00192040277636825,-0.0395205107533981,
-0.0127355554633069));
#43008=CARTESIAN_POINT('Ctrl Pts',(0.00194062379721181,-0.0395266485841883,
-0.0126613906611914));
#43009=CARTESIAN_POINT('Ctrl Pts',(0.00195039963330021,-0.0395300441949069,
-0.0126204969751554));
#43010=CARTESIAN_POINT('Ctrl Pts',(0.00198632348889163,-0.0395445915931025,
-0.0124460860663658));
#43011=CARTESIAN_POINT('Ctrl Pts',(0.00200009662524726,-0.03955610137136,
-0.0123104149942915));
#43012=CARTESIAN_POINT('Ctrl Pts',(0.00199999948980097,-0.0395676761865485,
-0.0121744247222927));
#43013=CARTESIAN_POINT('',(0.000482654256486283,-0.0397787742883183,-0.0102349656368742));
#43014=CARTESIAN_POINT('Ctrl Pts',(0.00199999947635761,-0.0395674495244771,
-0.0121744060238692));
#43015=CARTESIAN_POINT('Ctrl Pts',(0.00199970133985987,-0.0396002714048904,
-0.0117624056013177));
#43016=CARTESIAN_POINT('Ctrl Pts',(0.00186786604409727,-0.0396330932853036,
-0.0113509752358264));
#43017=CARTESIAN_POINT('Ctrl Pts',(0.00162916607223383,-0.0396659151657169,
-0.0110157593640319));
#43018=CARTESIAN_POINT('Ctrl Pts',(0.00161171964220948,-0.0396683140962045,
-0.0109912586479042));
#43019=CARTESIAN_POINT('Ctrl Pts',(0.00159372379493088,-0.0396707130266921,
-0.0109671563065562));
#43020=CARTESIAN_POINT('Ctrl Pts',(0.00157519789408884,-0.0396731119571797,
-0.0109434768852674));
#43021=CARTESIAN_POINT('Ctrl Pts',(0.00132172873142575,-0.0397059338375929,
-0.0106194978713678));
#43022=CARTESIAN_POINT('Ctrl Pts',(0.000964809959487887,-0.0397387557180061,
-0.0103761444985597));
#43023=CARTESIAN_POINT('Ctrl Pts',(0.000569808126240931,-0.0397715775984193,
-0.0102587412138639));
#43024=CARTESIAN_POINT('Ctrl Pts',(0.000540938099421197,-0.0397739764950523,
-0.0102501604031116));
#43025=CARTESIAN_POINT('Ctrl Pts',(0.000511876681535767,-0.0397763753916852,
-0.010242232583956));
#43026=CARTESIAN_POINT('Ctrl Pts',(0.000482654256486283,-0.0397787742883183,
-0.0102349656368742));
#43027=CARTESIAN_POINT('',(0.00171294960380956,-0.0397787743898723,-0.0132082309571848));
#43028=CARTESIAN_POINT('Origin',(0.,-0.0397787743898823,-0.0121758532865581));
#43029=CARTESIAN_POINT('',(0.00200022123764237,-0.0388647801189106,-0.0121764013269251));
#43030=CARTESIAN_POINT('Ctrl Pts',(0.00171294960381192,-0.0397787743898746,
-0.0132082309571895));
#43031=CARTESIAN_POINT('Ctrl Pts',(0.00150023895600091,-0.0397459829392836,
-0.0135611696787567));
#43032=CARTESIAN_POINT('Ctrl Pts',(0.00117410400373796,-0.0397157788326738,
-0.0138446217122324));
#43033=CARTESIAN_POINT('Ctrl Pts',(0.000797086095659716,-0.0396816687630686,
-0.0140093584080663));
#43034=CARTESIAN_POINT('Ctrl Pts',(0.000736412247895586,-0.039676179397375,
-0.0140358696399999));
#43035=CARTESIAN_POINT('Ctrl Pts',(0.000674460279395142,-0.0396706371456081,
-0.0140593805035415));
#43036=CARTESIAN_POINT('Ctrl Pts',(0.000611556020093166,-0.0396651474264523,
-0.0140798888792547));
#43037=CARTESIAN_POINT('Ctrl Pts',(0.000445016881923535,-0.039650613385242,
-0.0141341848403619));
#43038=CARTESIAN_POINT('Ctrl Pts',(0.000271030019870124,-0.0396363857556918,
-0.0141675943600055));
#43039=CARTESIAN_POINT('Ctrl Pts',(9.55329015372549E-5,-0.0396224105418801,
-0.0141760494170015));
#43040=CARTESIAN_POINT('Ctrl Pts',(-0.000134486275857888,-0.0396040936189845,
-0.014187131224347));
#43041=CARTESIAN_POINT('Ctrl Pts',(-0.000367011478658409,-0.0395862103113343,
-0.0141552106327799));
#43042=CARTESIAN_POINT('Ctrl Pts',(-0.000586810089275476,-0.0395686390442518,
-0.0140872852007923));
#43043=CARTESIAN_POINT('Ctrl Pts',(-0.000656254715950111,-0.0395630874619223,
-0.0140658243905858));
#43044=CARTESIAN_POINT('Ctrl Pts',(-0.000724490650272098,-0.0395574729195111,
-0.01404062219394));
#43045=CARTESIAN_POINT('Ctrl Pts',(-0.00079111974273048,-0.0395517690003329,
-0.01401186117842));
#43046=CARTESIAN_POINT('Ctrl Pts',(-0.00111283477109543,-0.039524227930021,
-0.013872990145026));
#43047=CARTESIAN_POINT('Ctrl Pts',(-0.00140093978232607,-0.0394943332468839,
-0.0136494145148475));
#43048=CARTESIAN_POINT('Ctrl Pts',(-0.00160907269804482,-0.0394657536876124,
-0.0133670741484452));
#43049=CARTESIAN_POINT('Ctrl Pts',(-0.00164226047277757,-0.0394611965421374,
-0.0133220536458219));
#43050=CARTESIAN_POINT('Ctrl Pts',(-0.00167343521716749,-0.0394566728347468,
-0.013275530438109));
#43051=CARTESIAN_POINT('Ctrl Pts',(-0.00170259000105306,-0.0394521974394702,
-0.0132277122546873));
#43052=CARTESIAN_POINT('Ctrl Pts',(-0.00173976013966668,-0.0394464916498667,
-0.0131667476969321));
#43053=CARTESIAN_POINT('Ctrl Pts',(-0.0017736876517133,-0.0394409546118393,
-0.0131038721225565));
#43054=CARTESIAN_POINT('Ctrl Pts',(-0.00180431702090932,-0.0394355645485264,
-0.0130394962385674));
#43055=CARTESIAN_POINT('Ctrl Pts',(-0.00197895506842673,-0.0394048322756237,
-0.0126724472596901));
#43056=CARTESIAN_POINT('Ctrl Pts',(-0.0020388440641331,-0.0393726943386263,
-0.0122505409511816));
#43057=CARTESIAN_POINT('Ctrl Pts',(-0.00197333802583864,-0.0393387239466838,
-0.0118491932184949));
#43058=CARTESIAN_POINT('Ctrl Pts',(-0.00196182927015393,-0.0393327556886184,
-0.0117786804364619));
#43059=CARTESIAN_POINT('Ctrl Pts',(-0.00194654553881331,-0.0393268034253514,
-0.011708817545723));
#43060=CARTESIAN_POINT('Ctrl Pts',(-0.00192778629130493,-0.039321097665926,
-0.0116399298725016));
#43061=CARTESIAN_POINT('Ctrl Pts',(-0.00191507534885312,-0.0393172315417828,
-0.0115932527736699));
#43062=CARTESIAN_POINT('Ctrl Pts',(-0.00190064394040254,-0.0393134035700773,
-0.0115470667176046));
#43063=CARTESIAN_POINT('Ctrl Pts',(-0.0018844539399446,-0.0393096042577624,
-0.0115015044103732));
#43064=CARTESIAN_POINT('Ctrl Pts',(-0.00176464438577769,-0.0392814885133697,
-0.0111643333441717));
#43065=CARTESIAN_POINT('Ctrl Pts',(-0.00154755482971262,-0.0392549422502329,
-0.0108606452113747));
#43066=CARTESIAN_POINT('Ctrl Pts',(-0.00127120349410412,-0.0392261183157976,
-0.010632760170493));
#43067=CARTESIAN_POINT('Ctrl Pts',(-0.00121609041974493,-0.0392203699243945,
-0.0105873127867277));
#43068=CARTESIAN_POINT('Ctrl Pts',(-0.00115860135483299,-0.0392145367366959,
-0.010544809906072));
#43069=CARTESIAN_POINT('Ctrl Pts',(-0.00109906668667438,-0.0392086411984728,
-0.0105054936416087));
#43070=CARTESIAN_POINT('Ctrl Pts',(-0.000912724758827148,-0.0391901883206427,
-0.0103824347795632));
#43071=CARTESIAN_POINT('Ctrl Pts',(-0.000705466934213524,-0.0391718322911769,
-0.0102884889069067));
#43072=CARTESIAN_POINT('Ctrl Pts',(-0.000488260829398752,-0.0391539022648083,
-0.0102339312550549));
#43073=CARTESIAN_POINT('Ctrl Pts',(-0.000310359136001515,-0.039139216756515,
-0.0101892460531335));
#43074=CARTESIAN_POINT('Ctrl Pts',(-0.000125860786950418,-0.0391248170262699,
-0.0101709505916726));
#43075=CARTESIAN_POINT('Ctrl Pts',(5.72982369894981E-5,-0.0391108839264696,
-0.0101767492571837));
#43076=CARTESIAN_POINT('Ctrl Pts',(0.000128621592728783,-0.0391054582837017,
-0.0101790072965321));
#43077=CARTESIAN_POINT('Ctrl Pts',(0.000199778699520524,-0.0391000352921531,
-0.0101850193738325));
#43078=CARTESIAN_POINT('Ctrl Pts',(0.000270361469596534,-0.039094544851949,
-0.0101947616994797));
#43079=CARTESIAN_POINT('Ctrl Pts',(0.000665306963198104,-0.0390638231246187,
-0.0102492748279304));
#43080=CARTESIAN_POINT('Ctrl Pts',(0.00104544158884886,-0.0390292888960902,
-0.0104228400803495));
#43081=CARTESIAN_POINT('Ctrl Pts',(0.00134169711478715,-0.0389972610858596,
-0.0106906329936509));
#43082=CARTESIAN_POINT('Ctrl Pts',(0.00134641586989222,-0.0389967509472131,
-0.0106948983965417));
#43083=CARTESIAN_POINT('Ctrl Pts',(0.00135111369317754,-0.0389962414444471,
-0.0106991880265136));
#43084=CARTESIAN_POINT('Ctrl Pts',(0.00135579052697412,-0.038995732603096,
-0.0107035016074603));
#43085=CARTESIAN_POINT('Ctrl Pts',(0.00140924983375533,-0.0389899162095538,
-0.0107528086936603));
#43086=CARTESIAN_POINT('Ctrl Pts',(0.0014597357188015,-0.0389841037191059,
-0.0108052585006679));
#43087=CARTESIAN_POINT('Ctrl Pts',(0.00150735437408238,-0.0389785280511923,
-0.0108600840695627));
#43088=CARTESIAN_POINT('Ctrl Pts',(0.00177724857175393,-0.0389469261420425,
-0.011170825791299));
#43089=CARTESIAN_POINT('Ctrl Pts',(0.00194813388996565,-0.0389156432761473,
-0.0115672436940755));
#43090=CARTESIAN_POINT('Ctrl Pts',(0.00199002028125891,-0.0388811955851008,
-0.0119772040445301));
#43091=CARTESIAN_POINT('Ctrl Pts',(0.0019967610977407,-0.0388756518856701,
-0.0120431793506355));
#43092=CARTESIAN_POINT('Ctrl Pts',(0.00200023005550795,-0.0388700852750759,
-0.0121094851408837));
#43093=CARTESIAN_POINT('Ctrl Pts',(0.00200038122575368,-0.0388645498389405,
-0.0121757929019176));
#43094=CARTESIAN_POINT('',(0.0019999997328271,-0.0378650183082204,-0.0121752053157853));
#43095=CARTESIAN_POINT('Ctrl Pts',(0.00199999951611709,-0.0388650992552875,
-0.0121772445203322));
#43096=CARTESIAN_POINT('Ctrl Pts',(0.00199971375497249,-0.0388324006779061,
-0.0125880469041955));
#43097=CARTESIAN_POINT('Ctrl Pts',(0.0018685951062426,-0.0387997021005247,
-0.0129985667414531));
#43098=CARTESIAN_POINT('Ctrl Pts',(0.00163102667195928,-0.0387670035231434,
-0.0133333298501901));
#43099=CARTESIAN_POINT('Ctrl Pts',(0.00156586986390711,-0.0387580354338581,
-0.013425143797126));
#43100=CARTESIAN_POINT('Ctrl Pts',(0.00149299350802138,-0.0387490673445728,
-0.0135113667208478));
#43101=CARTESIAN_POINT('Ctrl Pts',(0.00141349983230828,-0.0387400992552875,
-0.01359078021897));
#43102=CARTESIAN_POINT('Ctrl Pts',(0.00112899622298658,-0.0387080029438829,
-0.0138749968769863));
#43103=CARTESIAN_POINT('Ctrl Pts',(0.000754664908831541,-0.0386759066324783,
-0.0140714186061737));
#43104=CARTESIAN_POINT('Ctrl Pts',(0.000357828226795811,-0.0386438103210738,
-0.0141435826785498));
#43105=CARTESIAN_POINT('Ctrl Pts',(0.000239500984134324,-0.0386342399658117,
-0.0141651002853892));
#43106=CARTESIAN_POINT('Ctrl Pts',(0.000119335163155483,-0.0386246696105496,
-0.0141758907958467));
#43107=CARTESIAN_POINT('Ctrl Pts',(-6.26990510425628E-7,-0.0386150992552875,
-0.0141758531882788));
#43108=CARTESIAN_POINT('Ctrl Pts',(-0.000404434472395409,-0.0385828842529636,
-0.014175726596543));
#43109=CARTESIAN_POINT('Ctrl Pts',(-0.000809412778774544,-0.0385506692506397,
-0.0140490048166835));
#43110=CARTESIAN_POINT('Ctrl Pts',(-0.00114175084775083,-0.0385184542483158,
-0.0138179266715383));
#43111=CARTESIAN_POINT('Ctrl Pts',(-0.00123925659506402,-0.038509002583973,
-0.0137501299027253));
#43112=CARTESIAN_POINT('Ctrl Pts',(-0.00133062013334003,-0.0384995509196303,
-0.0136736807710986));
#43113=CARTESIAN_POINT('Ctrl Pts',(-0.0014143867001888,-0.0384900992552875,
-0.0135898936899162));
#43114=CARTESIAN_POINT('Ctrl Pts',(-0.001699842495272,-0.0384578903148794,
-0.0133043679870447));
#43115=CARTESIAN_POINT('Ctrl Pts',(-0.00189665011598153,-0.0384256813744713,
-0.0129285118578515));
#43116=CARTESIAN_POINT('Ctrl Pts',(-0.00196835538740126,-0.0383934724340632,
-0.0125302218360774));
#43117=CARTESIAN_POINT('Ctrl Pts',(-0.00198941068508536,-0.0383840147078046,
-0.0124132692772625));
#43118=CARTESIAN_POINT('Ctrl Pts',(-0.00199999185979339,-0.038374556981546,
-0.0122945381296574));
#43119=CARTESIAN_POINT('Ctrl Pts',(-0.00199999999529041,-0.0383650992552875,
-0.012175990539403));
#43120=CARTESIAN_POINT('Ctrl Pts',(-0.00200002770128779,-0.0383328903148794,
-0.0117722685278277));
#43121=CARTESIAN_POINT('Ctrl Pts',(-0.00187351208327366,-0.0383006813744713,
-0.0113673119004809));
#43122=CARTESIAN_POINT('Ctrl Pts',(-0.00164264075488384,-0.0382684724340632,
-0.0110349188667098));
#43123=CARTESIAN_POINT('Ctrl Pts',(-0.00157484846500414,-0.0382590147078046,
-0.010937316080532));
#43124=CARTESIAN_POINT('Ctrl Pts',(-0.00149838955109543,-0.0382495569815461,
-0.0108458593477331));
#43125=CARTESIAN_POINT('Ctrl Pts',(-0.00141458076793401,-0.0382400992552875,
-0.0107620070251169));
#43126=CARTESIAN_POINT('Ctrl Pts',(-0.00112911044763666,-0.0382078842529635,
-0.0104763884002906));
#43127=CARTESIAN_POINT('Ctrl Pts',(-0.000753248182734186,-0.0381756692506395,
-0.0102794205933449));
#43128=CARTESIAN_POINT('Ctrl Pts',(-0.00035490072884417,-0.0381434542483154,
-0.010207593783173));
#43129=CARTESIAN_POINT('Ctrl Pts',(-0.000238028273332784,-0.0381340025839728,
-0.0101865202816497));
#43130=CARTESIAN_POINT('Ctrl Pts',(-0.000119375880855756,-0.0381245509196302,
-0.01017590689184));
#43131=CARTESIAN_POINT('Ctrl Pts',(-9.01496180030455E-7,-0.0381150992552875,
-0.010175853489732));
#43132=CARTESIAN_POINT('Ctrl Pts',(0.000401418201829956,-0.0380830029438829,
-0.0101756721448781));
#43133=CARTESIAN_POINT('Ctrl Pts',(0.000805137298915929,-0.0380509066324782,
-0.0103011892691929));
#43134=CARTESIAN_POINT('Ctrl Pts',(0.00113689908351052,-0.0380188103210737,
-0.0105304170301468));
#43135=CARTESIAN_POINT('Ctrl Pts',(0.00123582254237512,-0.0380092399658116,
-0.0105987672863677));
#43136=CARTESIAN_POINT('Ctrl Pts',(0.00132846178825258,-0.0379996696105496,
-0.0106759973698235));
#43137=CARTESIAN_POINT('Ctrl Pts',(0.00141330561624802,-0.0379900992552875,
-0.010760732360601));
#43138=CARTESIAN_POINT('Ctrl Pts',(0.00170318748573643,-0.0379574006779062,
-0.0110502423711461));
#43139=CARTESIAN_POINT('Ctrl Pts',(0.00190167861782618,-0.037924702100525,
-0.0114324535509333));
#43140=CARTESIAN_POINT('Ctrl Pts',(0.00197119882455475,-0.0378920035231438,
-0.0118376592681693));
#43141=CARTESIAN_POINT('Ctrl Pts',(0.00199026581373331,-0.0378830354338584,
-0.0119487931872009));
#43142=CARTESIAN_POINT('Ctrl Pts',(0.00199990546780057,-0.0378740673445729,
-0.0120615186677999));
#43143=CARTESIAN_POINT('Ctrl Pts',(0.00199999930632796,-0.0378650992552875,
-0.0121741875471745));
#43144=CARTESIAN_POINT('',(0.00199999975724282,-0.0368651541991762,-0.0121765544739802));
#43145=CARTESIAN_POINT('Ctrl Pts',(0.00199999999997258,-0.0378649676055565,
-0.0121758428136169));
#43146=CARTESIAN_POINT('Ctrl Pts',(0.00200000215106864,-0.0378322885229654,
-0.0125866340168838));
#43147=CARTESIAN_POINT('Ctrl Pts',(0.00186917812243619,-0.0377996106305976,
-0.0129972356615072));
#43148=CARTESIAN_POINT('Ctrl Pts',(0.00163185633020602,-0.0377669292674898,
-0.0133321598711483));
#43149=CARTESIAN_POINT('Ctrl Pts',(0.0015666975511292,-0.0377579563126732,
-0.0134241162497783));
#43150=CARTESIAN_POINT('Ctrl Pts',(0.00149379912816242,-0.0377489830962234,
-0.0135104753770261));
#43151=CARTESIAN_POINT('Ctrl Pts',(0.00141426605178541,-0.037740009521673,
-0.0135900143575706));
#43152=CARTESIAN_POINT('Ctrl Pts',(0.00112991319882504,-0.0377079264985973,
-0.0138743883195708));
#43153=CARTESIAN_POINT('Ctrl Pts',(0.000755682143339694,-0.0376758388980586,
-0.0140710149774864));
#43154=CARTESIAN_POINT('Ctrl Pts',(0.000358876233171651,-0.0376437599461721,
-0.0141433918120423));
#43155=CARTESIAN_POINT('Ctrl Pts',(0.000240460523385157,-0.037634186873394,
-0.0141649906693587));
#43156=CARTESIAN_POINT('Ctrl Pts',(0.000120197207218872,-0.0376246145708288,
-0.0141758452605839));
#43157=CARTESIAN_POINT('Ctrl Pts',(1.33621037764426E-7,-0.037615043389977,
-0.0141758532820945));
#43158=CARTESIAN_POINT('Ctrl Pts',(-0.000403695574715009,-0.0375828510959709,
-0.0141758802621326));
#43159=CARTESIAN_POINT('Ctrl Pts',(-0.000808740639887077,-0.0375506714917629,
-0.0140492994009556));
#43160=CARTESIAN_POINT('Ctrl Pts',(-0.00114117588555066,-0.037518455536669,
-0.0138183262994985));
#43161=CARTESIAN_POINT('Ctrl Pts',(-0.00123877723638862,-0.0375089970909214,
-0.0137505137344847));
#43162=CARTESIAN_POINT('Ctrl Pts',(-0.00133023040427276,-0.0374995355117976,
-0.0136740338122211));
#43163=CARTESIAN_POINT('Ctrl Pts',(-0.00141407707748936,-0.037490069558209,
-0.0135902033206441));
#43164=CARTESIAN_POINT('Ctrl Pts',(-0.00169937545959153,-0.0374578605135292,
-0.0133049599985155));
#43165=CARTESIAN_POINT('Ctrl Pts',(-0.00189619771625313,-0.0374256008220651,
-0.0129294796373532));
#43166=CARTESIAN_POINT('Ctrl Pts',(-0.00196811542615174,-0.0373934727199154,
-0.0125315521329768));
#43167=CARTESIAN_POINT('Ctrl Pts',(-0.00198932393384032,-0.0373839981537422,
-0.0124142034500451));
#43168=CARTESIAN_POINT('Ctrl Pts',(-0.00199998497219453,-0.0373745350313396,
-0.0122950597653228));
#43169=CARTESIAN_POINT('Ctrl Pts',(-0.00199999998407383,-0.0373650880263686,
-0.0121761056844425));
#43170=CARTESIAN_POINT('Ctrl Pts',(-0.00200005102695467,-0.0373329666417254,
-0.0117716420688781));
#43171=CARTESIAN_POINT('Ctrl Pts',(-0.00187311158569394,-0.0373010315927791,
-0.0113660240936564));
#43172=CARTESIAN_POINT('Ctrl Pts',(-0.00164149534947217,-0.037269036273748,
-0.0110332715530873));
#43173=CARTESIAN_POINT('Ctrl Pts',(-0.00157400171920308,-0.0372597127467438,
-0.0109363065159611));
#43174=CARTESIAN_POINT('Ctrl Pts',(-0.00149794572979849,-0.037250384101868,
-0.0108454195059611));
#43175=CARTESIAN_POINT('Ctrl Pts',(-0.0014146164566859,-0.0372410442369463,
-0.0107620427333108));
#43176=CARTESIAN_POINT('Ctrl Pts',(-0.00112956846034967,-0.0372090949629093,
-0.0104768322532812));
#43177=CARTESIAN_POINT('Ctrl Pts',(-0.000754297942754812,-0.0371770143977276,
-0.0102799430662898));
#43178=CARTESIAN_POINT('Ctrl Pts',(-0.000356493832770366,-0.0371448730653759,
-0.0102078817046503));
#43179=CARTESIAN_POINT('Ctrl Pts',(-0.000238930692126867,-0.0371353743299911,
-0.0101865853937758));
#43180=CARTESIAN_POINT('Ctrl Pts',(-0.000119558078688254,-0.037125870287316,
-0.0101758755274922));
#43181=CARTESIAN_POINT('Ctrl Pts',(-3.72633079933872E-7,-0.0371163627576488,
-0.010175853321272));
#43182=CARTESIAN_POINT('Ctrl Pts',(0.000402000380372829,-0.0370842651022417,
-0.010175778352523));
#43183=CARTESIAN_POINT('Ctrl Pts',(0.000805732491409436,-0.0370521277036917,
-0.0103014342785915));
#43184=CARTESIAN_POINT('Ctrl Pts',(0.00113745747156368,-0.0370199314595979,
-0.0105308029832592));
#43185=CARTESIAN_POINT('Ctrl Pts',(0.00123647545702504,-0.0370103210671936,
-0.0105992682132624));
#43186=CARTESIAN_POINT('Ctrl Pts',(0.00132919144468881,-0.0370007054317224,
-0.0106766325077531));
#43187=CARTESIAN_POINT('Ctrl Pts',(0.00141408952576617,-0.0369910840451469,
-0.010761515698456));
#43188=CARTESIAN_POINT('Ctrl Pts',(0.00170382515047177,-0.0369582486922789,
-0.011051200506089));
#43189=CARTESIAN_POINT('Ctrl Pts',(0.0019021080795554,-0.0369253463572291,
-0.0114335426878814));
#43190=CARTESIAN_POINT('Ctrl Pts',(0.0019713954509908,-0.0368923837711043,
-0.0118388073315122));
#43191=CARTESIAN_POINT('Ctrl Pts',(0.00199042635448992,-0.0368833300607004,
-0.0119501198573703));
#43192=CARTESIAN_POINT('Ctrl Pts',(0.00200000049791846,-0.0368742718048616,
-0.0120630233263041));
#43193=CARTESIAN_POINT('Ctrl Pts',(0.00199999999998053,-0.036865209143065,
-0.0121758621122101));
#43194=CARTESIAN_POINT('',(0.00199999993113723,-0.0358650692048068,-0.0121754868239693));
#43195=CARTESIAN_POINT('Ctrl Pts',(0.0019999995145051,-0.0368650992552875,
-0.0121772468357502));
#43196=CARTESIAN_POINT('Ctrl Pts',(0.00199971327855225,-0.0368324031647462,
-0.0125880480977315));
#43197=CARTESIAN_POINT('Ctrl Pts',(0.00186859482625184,-0.036799707074205,
-0.0129985668623653));
#43198=CARTESIAN_POINT('Ctrl Pts',(0.0016310271184896,-0.0367670109836637,
-0.0133333292209738));
#43199=CARTESIAN_POINT('Ctrl Pts',(0.00156584748471249,-0.0367580404075383,
-0.0134251754072337));
#43200=CARTESIAN_POINT('Ctrl Pts',(0.00149294287498649,-0.0367490698314129,
-0.013511426630081));
#43201=CARTESIAN_POINT('Ctrl Pts',(0.00141341672260997,-0.0367400992552875,
-0.0135908632399671));
#43202=CARTESIAN_POINT('Ctrl Pts',(0.00112889816887164,-0.036708005468915,
-0.0138750614399711));
#43203=CARTESIAN_POINT('Ctrl Pts',(0.000754557696843852,-0.0366759116825424,
-0.0140714608728529));
#43204=CARTESIAN_POINT('Ctrl Pts',(0.000357718917181035,-0.0366438178961698,
-0.0141436025531799));
#43205=CARTESIAN_POINT('Ctrl Pts',(0.000239350517464174,-0.0366342450158757,
-0.0141651208515188));
#43206=CARTESIAN_POINT('Ctrl Pts',(0.000119142893453722,-0.0366246721355816,
-0.01417590468007));
#43207=CARTESIAN_POINT('Ctrl Pts',(-8.59619391707486E-7,-0.0366150992552875,
-0.0141758531018217));
#43208=CARTESIAN_POINT('Ctrl Pts',(-0.00040466476463091,-0.0365828867771829,
-0.014175679542439));
#43209=CARTESIAN_POINT('Ctrl Pts',(-0.000809626539648802,-0.0365506742990785,
-0.014048912036177));
#43210=CARTESIAN_POINT('Ctrl Pts',(-0.0011419369127495,-0.0365184618209739,
-0.0138177972829539));
#43211=CARTESIAN_POINT('Ctrl Pts',(-0.00123946821469572,-0.0365090076324118,
-0.0137499663495692));
#43212=CARTESIAN_POINT('Ctrl Pts',(-0.00133085212103917,-0.0364995534438496,
-0.0136734778336607));
#43213=CARTESIAN_POINT('Ctrl Pts',(-0.00141463257027406,-0.0364900992552875,
-0.0135896477168484));
#43214=CARTESIAN_POINT('Ctrl Pts',(-0.00170003711586502,-0.036457892834635,
-0.0133040739748339));
#43215=CARTESIAN_POINT('Ctrl Pts',(-0.00189677909075885,-0.0364256864139827,
-0.0129281858052638));
#43216=CARTESIAN_POINT('Ctrl Pts',(-0.00196841594664184,-0.0363934799933302,
-0.012529885292182));
#43217=CARTESIAN_POINT('Ctrl Pts',(-0.0019894584054625,-0.036384019747316,
-0.0124128893402874));
#43218=CARTESIAN_POINT('Ctrl Pts',(-0.00200001928488183,-0.0363745595013017,
-0.0122941153820976));
#43219=CARTESIAN_POINT('Ctrl Pts',(-0.00199999997348158,-0.0363650992552875,
-0.0121755275970281));
#43220=CARTESIAN_POINT('Ctrl Pts',(-0.00199993422983402,-0.0363328928346353,
-0.0117718078539671));
#43221=CARTESIAN_POINT('Ctrl Pts',(-0.0018733262230654,-0.0363006864139831,
-0.0113668822653373));
#43222=CARTESIAN_POINT('Ctrl Pts',(-0.00164237995384072,-0.0362684799933309,
-0.0110345434744465));
#43223=CARTESIAN_POINT('Ctrl Pts',(-0.00157454228424741,-0.0362590197473164,
-0.0109369229795792));
#43224=CARTESIAN_POINT('Ctrl Pts',(-0.00149803348157776,-0.036249559501302,
-0.0108454547200247));
#43225=CARTESIAN_POINT('Ctrl Pts',(-0.00141417203720899,-0.0362400992552875,
-0.0107615982002402));
#43226=CARTESIAN_POINT('Ctrl Pts',(-0.00112862080139359,-0.0362078867771829,
-0.0104760637328111));
#43227=CARTESIAN_POINT('Ctrl Pts',(-0.000752703850683686,-0.0361756742990784,
-0.0102792048728464));
#43228=CARTESIAN_POINT('Ctrl Pts',(-0.000354337681183733,-0.0361434618209737,
-0.0102074923420936));
#43229=CARTESIAN_POINT('Ctrl Pts',(-0.000237419359315358,-0.0361340076324117,
-0.0101864451011517));
#43230=CARTESIAN_POINT('Ctrl Pts',(-0.000118722882568433,-0.0361245534438496,
-0.0101758656371648));
#43231=CARTESIAN_POINT('Ctrl Pts',(-2.08240354928347E-7,-0.0361150992552875,
-0.0101758532973991));
#43232=CARTESIAN_POINT('Ctrl Pts',(0.000402109058929343,-0.036083005468915,
-0.0101758114080503));
#43233=CARTESIAN_POINT('Ctrl Pts',(0.000805782738187552,-0.0360509116825423,
-0.0103014670235892));
#43234=CARTESIAN_POINT('Ctrl Pts',(0.0011374641750515,-0.0360188178961697,
-0.0105308076183548));
#43235=CARTESIAN_POINT('Ctrl Pts',(0.00123639755280903,-0.0360092450158756,
-0.0105992149428997));
#43236=CARTESIAN_POINT('Ctrl Pts',(0.00132903940203891,-0.0359996721355816,
-0.0106765059496287));
#43237=CARTESIAN_POINT('Ctrl Pts',(0.00141387750156739,-0.0359900992552875,
-0.0107613037432188));
#43238=CARTESIAN_POINT('Ctrl Pts',(0.00170364130288576,-0.0359574031647456,
-0.0110509298799503));
#43239=CARTESIAN_POINT('Ctrl Pts',(0.00190197781676828,-0.0359247070742038,
-0.0114332199240294));
#43240=CARTESIAN_POINT('Ctrl Pts',(0.00197133477400979,-0.035892010983662,
-0.0118384526215028));
#43241=CARTESIAN_POINT('Ctrl Pts',(0.00199036371154978,-0.0358830404075371,
-0.0119496332152899));
#43242=CARTESIAN_POINT('Ctrl Pts',(0.00199995803787705,-0.0358740698314123,
-0.012062402698519));
#43243=CARTESIAN_POINT('Ctrl Pts',(0.00199999986229583,-0.0358650992552875,
-0.0121751111163331));
#43244=CARTESIAN_POINT('',(0.00199999998396862,-0.0348650992552875,-0.0121756000563658));
#43245=CARTESIAN_POINT('Ctrl Pts',(0.00199999999997863,-0.0358650391543261,
-0.0121758625316054));
#43246=CARTESIAN_POINT('Ctrl Pts',(0.00199999810105016,-0.0358323500840859,
-0.0125866616126267));
#43247=CARTESIAN_POINT('Ctrl Pts',(0.00186916518615,-0.0357996610138456,
-0.0129972691594506));
#43248=CARTESIAN_POINT('Ctrl Pts',(0.00163183150648035,-0.0357669719436053,
-0.0133321949032346));
#43249=CARTESIAN_POINT('Ctrl Pts',(0.00156666930865016,-0.0357579968513856,
-0.0134241519217465));
#43250=CARTESIAN_POINT('Ctrl Pts',(0.00149376720214781,-0.035749021759166,
-0.0135105113347003));
#43251=CARTESIAN_POINT('Ctrl Pts',(0.00141423022479208,-0.0357400466669462,
-0.0135900501863159));
#43252=CARTESIAN_POINT('Ctrl Pts',(0.00112987870759773,-0.0357079599423248,
-0.0138744084041501));
#43253=CARTESIAN_POINT('Ctrl Pts',(0.000755656078176272,-0.0356758732177034,
-0.0140710224466294));
#43254=CARTESIAN_POINT('Ctrl Pts',(0.000358863204303028,-0.0356437864930819,
-0.0141433941884449));
#43255=CARTESIAN_POINT('Ctrl Pts',(0.000240426089604611,-0.0356342090552434,
-0.0141649961396156));
#43256=CARTESIAN_POINT('Ctrl Pts',(0.000120140973166075,-0.0356246316174049,
-0.0141758499009532));
#43257=CARTESIAN_POINT('Ctrl Pts',(5.63737627424982E-8,-0.0356150541795664,
-0.0141758532857636));
#43258=CARTESIAN_POINT('Ctrl Pts',(-0.000403744092267254,-0.0355828487686996,
-0.0141758646676394));
#43259=CARTESIAN_POINT('Ctrl Pts',(-0.000808760244496433,-0.0355506433578327,
-0.0140492854455321));
#43260=CARTESIAN_POINT('Ctrl Pts',(-0.00114117477149515,-0.0355184379469659,
-0.013818327073534));
#43261=CARTESIAN_POINT('Ctrl Pts',(-0.00123880514950277,-0.0355089791953728,
-0.0137504944388842));
#43262=CARTESIAN_POINT('Ctrl Pts',(-0.00133028359890378,-0.0354995204437797,
-0.0136739893304062));
#43263=CARTESIAN_POINT('Ctrl Pts',(-0.00141415049894442,-0.0354900616921866,
-0.0135901299095478));
#43264=CARTESIAN_POINT('Ctrl Pts',(-0.00169964914213271,-0.0354578623293297,
-0.0133046567268976));
#43265=CARTESIAN_POINT('Ctrl Pts',(-0.00189651867363536,-0.035425662966473,
-0.012928840079799));
#43266=CARTESIAN_POINT('Ctrl Pts',(-0.0019682930311079,-0.0353934636036161,
-0.0125305680222149));
#43267=CARTESIAN_POINT('Ctrl Pts',(-0.00198939065074527,-0.035383998804013,
-0.0124134984631273));
#43268=CARTESIAN_POINT('Ctrl Pts',(-0.00199999275787943,-0.0353745340044099,
-0.0122946447989551));
#43269=CARTESIAN_POINT('Ctrl Pts',(-0.00199999999627945,-0.0353650692048068,
-0.0121759752791308));
#43270=CARTESIAN_POINT('Ctrl Pts',(-0.00200002462140399,-0.0353328698419498,
-0.0117722601357449));
#43271=CARTESIAN_POINT('Ctrl Pts',(-0.00187350998838232,-0.0353006704790928,
-0.0113673097625285));
#43272=CARTESIAN_POINT('Ctrl Pts',(-0.0016426421671473,-0.0352684711162358,
-0.0110349208999945));
#43273=CARTESIAN_POINT('Ctrl Pts',(-0.00157478002737553,-0.0352590063166328,
-0.0109372172905127));
#43274=CARTESIAN_POINT('Ctrl Pts',(-0.00149823330755494,-0.0352495415170299,
-0.0108456724683233));
#43275=CARTESIAN_POINT('Ctrl Pts',(-0.00141432301966507,-0.0352400767174269,
-0.0107617491899494));
#43276=CARTESIAN_POINT('Ctrl Pts',(-0.00112880558550729,-0.03520787130656,
-0.0104761875537067));
#43277=CARTESIAN_POINT('Ctrl Pts',(-0.000752914192981799,-0.035175665895693,
-0.0102792891629694));
#43278=CARTESIAN_POINT('Ctrl Pts',(-0.000354559808701529,-0.0351434604848261,
-0.010207532341678));
#43279=CARTESIAN_POINT('Ctrl Pts',(-0.000237562848704204,-0.0351340017332331,
-0.0101864573133077));
#43280=CARTESIAN_POINT('Ctrl Pts',(-0.00011878408890704,-0.0351245429816401,
-0.0101758644203822));
#43281=CARTESIAN_POINT('Ctrl Pts',(-1.87611382613396E-7,-0.0351150842300471,
-0.0101758532953576));
#43282=CARTESIAN_POINT('Ctrl Pts',(0.000402124731635335,-0.0350829975054256,
-0.01017581555617));
#43283=CARTESIAN_POINT('Ctrl Pts',(0.000805793279976232,-0.0350509107808041,
-0.010301472403883));
#43284=CARTESIAN_POINT('Ctrl Pts',(0.00113747058010921,-0.0350188240561825,
-0.0105308120471401));
#43285=CARTESIAN_POINT('Ctrl Pts',(0.00123647160816373,-0.0350092466183441,
-0.010599266718132));
#43286=CARTESIAN_POINT('Ctrl Pts',(0.00132917239425267,-0.0349996691805057,
-0.0106766172816647));
#43287=CARTESIAN_POINT('Ctrl Pts',(0.0014140576927508,-0.0349900917426673,
-0.0107614838717402));
#43288=CARTESIAN_POINT('Ctrl Pts',(0.00170378251600591,-0.034957402672427,
-0.0110511448406587));
#43289=CARTESIAN_POINT('Ctrl Pts',(0.00190207010452223,-0.0349247136021869,
-0.0114334574315659));
#43290=CARTESIAN_POINT('Ctrl Pts',(0.00197137654199078,-0.0348920245319466,
-0.0118386967506753));
#43291=CARTESIAN_POINT('Ctrl Pts',(0.00199040527737932,-0.0348830494397269,
-0.0119499590237631));
#43292=CARTESIAN_POINT('Ctrl Pts',(0.00199998570320917,-0.0348740743475072,
-0.0120628112991658));
#43293=CARTESIAN_POINT('Ctrl Pts',(0.00199999998396862,-0.0348650992552875,
-0.0121756000563658));
#43294=CARTESIAN_POINT('',(0.00151022347084785,-0.033978774491363,-0.0108646610549993));
#43295=CARTESIAN_POINT('Ctrl Pts',(0.00199999999999937,-0.0348650793296435,
-0.0121758517007548));
#43296=CARTESIAN_POINT('Ctrl Pts',(0.00200000032705075,-0.0348322521293468,
-0.012588325784795));
#43297=CARTESIAN_POINT('Ctrl Pts',(0.0018681630713516,-0.0347994249290503,
-0.0130003324786179));
#43298=CARTESIAN_POINT('Ctrl Pts',(0.00162913623717455,-0.0347665977287537,
-0.0133359891065054));
#43299=CARTESIAN_POINT('Ctrl Pts',(0.00159926749830595,-0.0347624956492662,
-0.0133779326824323));
#43300=CARTESIAN_POINT('Ctrl Pts',(0.00156778734423012,-0.0347583935697786,
-0.0134187091307775));
#43301=CARTESIAN_POINT('Ctrl Pts',(0.00153479466821863,-0.0347542914902911,
-0.0134581969715379));
#43302=CARTESIAN_POINT('Ctrl Pts',(0.00127462777450834,-0.0347219441512135,
-0.0137695821064207));
#43303=CARTESIAN_POINT('Ctrl Pts',(0.000915968269259364,-0.0346895968121359,
-0.0139996029213947));
#43304=CARTESIAN_POINT('Ctrl Pts',(0.000523877086159381,-0.0346572494730582,
-0.0141060223979567));
#43305=CARTESIAN_POINT('Ctrl Pts',(0.000468336811576201,-0.0346526674264021,
-0.0141210968683962));
#43306=CARTESIAN_POINT('Ctrl Pts',(0.000412168092072666,-0.034648085379746,
-0.0141337662396896));
#43307=CARTESIAN_POINT('Ctrl Pts',(0.000355589182912084,-0.0346435033330899,
-0.0141439885291154));
#43308=CARTESIAN_POINT('Ctrl Pts',(-4.50978435600636E-5,-0.034611053668064,
-0.0142163819141155));
#43309=CARTESIAN_POINT('Ctrl Pts',(-0.000469128586302042,-0.0345786040030382,
-0.0141623070471811));
#43310=CARTESIAN_POINT('Ctrl Pts',(-0.000839059891153366,-0.0345461543380124,
-0.0139913362798846));
#43311=CARTESIAN_POINT('Ctrl Pts',(-0.000890129414537668,-0.0345416746173045,
-0.0139677335312554));
#43312=CARTESIAN_POINT('Ctrl Pts',(-0.000940182994600609,-0.0345371948965965,
-0.0139419834046748));
#43313=CARTESIAN_POINT('Ctrl Pts',(-0.000989039558319999,-0.0345327151758886,
-0.0139141860372357));
#43314=CARTESIAN_POINT('Ctrl Pts',(-0.00134282545405926,-0.0345002760953913,
-0.0137128964705946));
#43315=CARTESIAN_POINT('Ctrl Pts',(-0.0016334871013328,-0.0344678370148941,
-0.013399653616246));
#43316=CARTESIAN_POINT('Ctrl Pts',(-0.00180776228675333,-0.0344353979343968,
-0.0130314206507045));
#43317=CARTESIAN_POINT('Ctrl Pts',(-0.00183188592915287,-0.0344309076291604,
-0.012980448847926));
#43318=CARTESIAN_POINT('Ctrl Pts',(-0.00185384300905548,-0.0344264173239238,
-0.0129284757178915));
#43319=CARTESIAN_POINT('Ctrl Pts',(-0.00187355828541564,-0.0344219270186873,
-0.0128756956624903));
#43320=CARTESIAN_POINT('Ctrl Pts',(-0.00201598633945715,-0.0343894879381893,
-0.0124943994307929));
#43321=CARTESIAN_POINT('Ctrl Pts',(-0.0020382020764351,-0.0343570488576914,
-0.01206765550411));
#43322=CARTESIAN_POINT('Ctrl Pts',(-0.00193583731724208,-0.0343246097771934,
-0.0116733257936057));
#43323=CARTESIAN_POINT('Ctrl Pts',(-0.00192166771048669,-0.0343201194719576,
-0.0116187416088349));
#43324=CARTESIAN_POINT('Ctrl Pts',(-0.00190519331909169,-0.0343156291667219,
-0.0115647779859285));
#43325=CARTESIAN_POINT('Ctrl Pts',(-0.00188648100612665,-0.0343111388614861,
-0.0115116323793869));
#43326=CARTESIAN_POINT('Ctrl Pts',(-0.00175125450020657,-0.0342786891964616,
-0.0111275700408051));
#43327=CARTESIAN_POINT('Ctrl Pts',(-0.00149456243379751,-0.0342462395314371,
-0.0107857583555539));
#43328=CARTESIAN_POINT('Ctrl Pts',(-0.00116302081515074,-0.0342137898664127,
-0.0105487753586376));
#43329=CARTESIAN_POINT('Ctrl Pts',(-0.00111725104051885,-0.0342093101457034,
-0.0105160595312711));
#43330=CARTESIAN_POINT('Ctrl Pts',(-0.00107011722766352,-0.0342048304249941,
-0.0104852886495492));
#43331=CARTESIAN_POINT('Ctrl Pts',(-0.00102179595564649,-0.0342003507042848,
-0.0104565705800132));
#43332=CARTESIAN_POINT('Ctrl Pts',(-0.000672875861731956,-0.0341680033652071,
-0.0102492020422803));
#43333=CARTESIAN_POINT('Ctrl Pts',(-0.000258148398025065,-0.0341356560261293,
-0.0101514162840617));
#43334=CARTESIAN_POINT('Ctrl Pts',(0.000146938291752795,-0.0341033086870516,
-0.0101812583055114));
#43335=CARTESIAN_POINT('Ctrl Pts',(0.000204319398366628,-0.0340987266403956,
-0.0101854854703568));
#43336=CARTESIAN_POINT('Ctrl Pts',(0.000261492385574115,-0.0340941445937395,
-0.010192188646196));
#43337=CARTESIAN_POINT('Ctrl Pts',(0.000318237676841534,-0.0340895625470835,
-0.0102013344132529));
#43338=CARTESIAN_POINT('Ctrl Pts',(0.000724778513515946,-0.0340567353461015,
-0.0102668575202505));
#43339=CARTESIAN_POINT('Ctrl Pts',(0.00111065972736407,-0.0340239081451195,
-0.0104621803986175));
#43340=CARTESIAN_POINT('Ctrl Pts',(0.00140441949822839,-0.0339910809441375,
-0.0107519130234164));
#43341=CARTESIAN_POINT('Ctrl Pts',(0.00144112829092725,-0.0339869787932127,
-0.0107881185761051));
#43342=CARTESIAN_POINT('Ctrl Pts',(0.00147643170979932,-0.0339828766422878,
-0.0108257399041348));
#43343=CARTESIAN_POINT('Ctrl Pts',(0.00151022347084785,-0.033978774491363,
-0.0108646610549993));
#43344=CARTESIAN_POINT('',(-0.00169751808661698,-0.0339787743898723,-0.0111182936685657));
#43345=CARTESIAN_POINT('Origin',(0.,-0.0339787743898823,-0.0121758532865581));
#43346=CARTESIAN_POINT('',(0.0020000130015625,-0.0345673401423348,-0.0121758452034492));
#43347=CARTESIAN_POINT('Ctrl Pts',(-0.00169751808661312,-0.0339787743898749,
-0.0111182936685678));
#43348=CARTESIAN_POINT('Ctrl Pts',(-0.0019133302484519,-0.03401125030809,
-0.0114646937499832));
#43349=CARTESIAN_POINT('Ctrl Pts',(-0.00201817591253676,-0.034041195055471,
-0.0118800195650646));
#43350=CARTESIAN_POINT('Ctrl Pts',(-0.00199618519646481,-0.0340749668219992,
-0.012287326618901));
#43351=CARTESIAN_POINT('Ctrl Pts',(-0.00198495985050248,-0.0340922059042464,
-0.0124952399300115));
#43352=CARTESIAN_POINT('Ctrl Pts',(-0.00194135350589726,-0.0341100889178837,
-0.012701077025495));
#43353=CARTESIAN_POINT('Ctrl Pts',(-0.00186710706940351,-0.0341270620260995,
-0.0128946273200806));
#43354=CARTESIAN_POINT('Ctrl Pts',(-0.00185372474489184,-0.034130121292683,
-0.0129295132078591));
#43355=CARTESIAN_POINT('Ctrl Pts',(-0.00183936109686421,-0.0341331408248404,
-0.0129640224176434));
#43356=CARTESIAN_POINT('Ctrl Pts',(-0.00182399630821732,-0.0341361278602697,
-0.0129980955529474));
#43357=CARTESIAN_POINT('Ctrl Pts',(-0.00167662706547824,-0.0341647775969737,
-0.0133249033120966));
#43358=CARTESIAN_POINT('Ctrl Pts',(-0.0014356238739396,-0.0341904378226505,
-0.0136128782517713));
#43359=CARTESIAN_POINT('Ctrl Pts',(-0.0011393861182615,-0.0342194947185986,
-0.0138186255099517));
#43360=CARTESIAN_POINT('Ctrl Pts',(-0.00095945763406348,-0.0342371432564478,
-0.0139435919991406));
#43361=CARTESIAN_POINT('Ctrl Pts',(-0.000759448108284487,-0.0342558025273501,
-0.0140389235176684));
#43362=CARTESIAN_POINT('Ctrl Pts',(-0.000550305419734492,-0.034273777241299,
-0.0140995996071181));
#43363=CARTESIAN_POINT('Ctrl Pts',(-0.00047822934401059,-0.034279971800873,
-0.0141205101847153));
#43364=CARTESIAN_POINT('Ctrl Pts',(-0.000404945039041054,-0.0342860347339131,
-0.0141374504388133));
#43365=CARTESIAN_POINT('Ctrl Pts',(-0.000330820056329016,-0.0342920074279103,
-0.0141499875472947));
#43366=CARTESIAN_POINT('Ctrl Pts',(-1.38987420090911E-5,-0.0343175436771257,
-0.0142035899462743));
#43367=CARTESIAN_POINT('Ctrl Pts',(0.000319303757953489,-0.034341430366152,
-0.0141758977409307));
#43368=CARTESIAN_POINT('Ctrl Pts',(0.000625857835872285,-0.0343669021623781,
-0.0140747561372667));
#43369=CARTESIAN_POINT('Ctrl Pts',(0.000833909794261486,-0.0343841893474794,
-0.0140061134075409));
#43370=CARTESIAN_POINT('Ctrl Pts',(0.00103028204907868,-0.0344024350641547,
-0.0139035910702775));
#43371=CARTESIAN_POINT('Ctrl Pts',(0.00120436386342799,-0.0344205562780359,
-0.0137730316152375));
#43372=CARTESIAN_POINT('Ctrl Pts',(0.00129433949622915,-0.034429922378063,
-0.0137055508756249));
#43373=CARTESIAN_POINT('Ctrl Pts',(0.00137898091997455,-0.0344389951962281,
-0.0136307290564667));
#43374=CARTESIAN_POINT('Ctrl Pts',(0.0014564302820324,-0.0344478989440412,
-0.0135488195897293));
#43375=CARTESIAN_POINT('Ctrl Pts',(0.00165855072246001,-0.0344711351513078,
-0.013335059565731));
#43376=CARTESIAN_POINT('Ctrl Pts',(0.00181152170565784,-0.0344932198896048,
-0.0130723078730732));
#43377=CARTESIAN_POINT('Ctrl Pts',(0.00190227021810968,-0.0345163608536293,
-0.0127910916953787));
#43378=CARTESIAN_POINT('Ctrl Pts',(0.00196634393264011,-0.0345326997167445,
-0.0125925367592799));
#43379=CARTESIAN_POINT('Ctrl Pts',(0.0019995103779209,-0.0345498932533823,
-0.0123841045160361));
#43380=CARTESIAN_POINT('Ctrl Pts',(0.0020000130015625,-0.0345673401423348,
-0.0121758452034492));
#43381=CARTESIAN_POINT('Ctrl Pts',(0.00199999995026977,-0.0345673849471511,
-0.0121754072810601));
#43382=CARTESIAN_POINT('Ctrl Pts',(0.00199997483940943,-0.0345769756133014,
-0.0120628039170363));
#43383=CARTESIAN_POINT('Ctrl Pts',(0.00199044020054723,-0.0345866097090282,
-0.0119503946982784));
#43384=CARTESIAN_POINT('Ctrl Pts',(0.00196689070359113,-0.0345981735004672,
-0.0118124124127049));
#43385=CARTESIAN_POINT('Ctrl Pts',(0.00196173542751688,-0.0346004120463131,
-0.0117855423331393));
#43386=CARTESIAN_POINT('Ctrl Pts',(0.0019519162326337,-0.0346042167170265,
-0.0117394908298653));
#43387=CARTESIAN_POINT('Ctrl Pts',(0.00194751723602006,-0.0346057952830513,
-0.0117202592932969));
#43388=CARTESIAN_POINT('Ctrl Pts',(0.00193622838000297,-0.0346095634041527,
-0.0116740625413711));
#43389=CARTESIAN_POINT('Ctrl Pts',(0.0019290591281148,-0.0346117384194698,
-0.0116471705825984));
#43390=CARTESIAN_POINT('Ctrl Pts',(0.00188992727544227,-0.0346226345829043,
-0.0115118037274921));
#43391=CARTESIAN_POINT('Ctrl Pts',(0.00184936335889547,-0.0346309859424247,
-0.011406016331714));
#43392=CARTESIAN_POINT('Ctrl Pts',(0.00174871055688625,-0.0346480914081593,
-0.0111981529790634));
#43393=CARTESIAN_POINT('Ctrl Pts',(0.00168808606614052,-0.0346568196365459,
-0.011096850275457));
#43394=CARTESIAN_POINT('Ctrl Pts',(0.00159420933613803,-0.0346690772020404,
-0.0109674390119659));
#43395=CARTESIAN_POINT('Ctrl Pts',(0.00156845062042185,-0.0346723350491007,
-0.0109341888235039));
#43396=CARTESIAN_POINT('Ctrl Pts',(0.0015198909108764,-0.0346783141498106,
-0.0108754303230239));
#43397=CARTESIAN_POINT('Ctrl Pts',(0.00149744660900956,-0.0346810206556933,
-0.0108496475581069));
#43398=CARTESIAN_POINT('Ctrl Pts',(0.00144520509277452,-0.0346872046453558,
-0.0107926529359178));
#43399=CARTESIAN_POINT('Ctrl Pts',(0.00141503726758382,-0.0346906966565683,
-0.0107618059292982));
#43400=CARTESIAN_POINT('Ctrl Pts',(0.0012870616409788,-0.0347052139341774,
-0.010639147773148));
#43401=CARTESIAN_POINT('Ctrl Pts',(0.00118114979711425,-0.0347165846630359,
-0.0105563271783615));
#43402=CARTESIAN_POINT('Ctrl Pts',(0.000987151030180866,-0.0347361398669616,
-0.0104338362117405));
#43403=CARTESIAN_POINT('Ctrl Pts',(0.000902987008983808,-0.0347442619514332,
-0.0103887582938902));
#43404=CARTESIAN_POINT('Ctrl Pts',(0.000790806107578523,-0.0347544167303081,
-0.0103386319094809));
#43405=CARTESIAN_POINT('Ctrl Pts',(0.000765460603026857,-0.0347566686338392,
-0.0103279282403209));
#43406=CARTESIAN_POINT('Ctrl Pts',(0.000721582832399333,-0.0347604858640932,
-0.0103104560210856));
#43407=CARTESIAN_POINT('Ctrl Pts',(0.000703158745241538,-0.0347620639457492,
-0.0103034332983042));
#43408=CARTESIAN_POINT('Ctrl Pts',(0.000658663085280927,-0.0347658175142602,
-0.0102872223561991));
#43409=CARTESIAN_POINT('Ctrl Pts',(0.000632499734172252,-0.034767978883676,
-0.0102783000826411));
#43410=CARTESIAN_POINT('Ctrl Pts',(0.00049542523263479,-0.0347791082681094,
-0.0102347052184396));
#43411=CARTESIAN_POINT('Ctrl Pts',(0.000381818583535505,-0.0347876849627012,
-0.010209200331013));
#43412=CARTESIAN_POINT('Ctrl Pts',(0.000152699183736938,-0.0348048163840472,
-0.0101783805649375));
#43413=CARTESIAN_POINT('Ctrl Pts',(3.76752542759658E-5,-0.0348133421599191,
-0.0101729077919167));
#43414=CARTESIAN_POINT('Ctrl Pts',(-0.000119663222632085,-0.0348254146126436,
-0.010178983556825));
#43415=CARTESIAN_POINT('Ctrl Pts',(-0.000162085934081661,-0.0348287088161045,
-0.0101819787509695));
#43416=CARTESIAN_POINT('Ctrl Pts',(-0.000238718750367696,-0.0348347518383239,
-0.010189851002067));
#43417=CARTESIAN_POINT('Ctrl Pts',(-0.000272959951319575,-0.0348374856203169,
-0.0101942669799029));
#43418=CARTESIAN_POINT('Ctrl Pts',(-0.000350188852032124,-0.0348437374656436,
-0.0102062665053244));
#43419=CARTESIAN_POINT('Ctrl Pts',(-0.000393075562394101,-0.0348472703156863,
-0.0102143754414659));
#43420=CARTESIAN_POINT('Ctrl Pts',(-0.000561439542848433,-0.0348613991661833,
-0.010251952482215));
#43421=CARTESIAN_POINT('Ctrl Pts',(-0.000684191800726341,-0.0348723039615588,
-0.0102921123733125));
#43422=CARTESIAN_POINT('Ctrl Pts',(-0.000893472808505717,-0.0348917542728829,
-0.010383750454362));
#43423=CARTESIAN_POINT('Ctrl Pts',(-0.000981632432394317,-0.0349002397578543,
-0.0104304800640631));
#43424=CARTESIAN_POINT('Ctrl Pts',(-0.00108875635346201,-0.0349106863121,
-0.010497956926511));
#43425=CARTESIAN_POINT('Ctrl Pts',(-0.00111127305248858,-0.0349128897294522,
-0.0105127841343851));
#43426=CARTESIAN_POINT('Ctrl Pts',(-0.00114985736006802,-0.034916670317033,
-0.0105393255720873));
#43427=CARTESIAN_POINT('Ctrl Pts',(-0.00116606079257463,-0.034918258806829,
-0.0105508310641559));
#43428=CARTESIAN_POINT('Ctrl Pts',(-0.00120531444845609,-0.0349221110952953,
-0.0105795933214726));
#43429=CARTESIAN_POINT('Ctrl Pts',(-0.00122816824723893,-0.0349243586670241,
-0.0105971095450949));
#43430=CARTESIAN_POINT('Ctrl Pts',(-0.00131300200722041,-0.0349327541595328,
-0.0106650877875477));
#43431=CARTESIAN_POINT('Ctrl Pts',(-0.00137232240937095,-0.0349387352068917,
-0.0107187600380388));
#43432=CARTESIAN_POINT('Ctrl Pts',(-0.00149853119746944,-0.0349521372694498,
-0.0108475171474998));
#43433=CARTESIAN_POINT('Ctrl Pts',(-0.00156328883612012,-0.0349595204109482,
-0.0109243741651363));
#43434=CARTESIAN_POINT('Ctrl Pts',(-0.00166076931043963,-0.0349720322915117,
-0.0110595039264108));
#43435=CARTESIAN_POINT('Ctrl Pts',(-0.00169683695489829,-0.0349770647267152,
-0.0111151302090635));
#43436=CARTESIAN_POINT('Ctrl Pts',(-0.00174870684972281,-0.034985067715539,
-0.0112045636919352));
#43437=CARTESIAN_POINT('Ctrl Pts',(-0.00176643891152485,-0.034987970477539,
-0.0112371987444787));
#43438=CARTESIAN_POINT('Ctrl Pts',(-0.00179918394341318,-0.034993685646959,
-0.0113016820149685));
#43439=CARTESIAN_POINT('Ctrl Pts',(-0.00181428474557568,-0.0349964937921137,
-0.0113334704610511));
#43440=CARTESIAN_POINT('Ctrl Pts',(-0.00185067358125213,-0.0350037348267818,
-0.0114155948575722));
#43441=CARTESIAN_POINT('Ctrl Pts',(-0.00187075009031881,-0.0350082049994866,
-0.0114664319964782));
#43442=CARTESIAN_POINT('Ctrl Pts',(-0.00193419812995889,-0.0350241963055464,
-0.011648599706018));
#43443=CARTESIAN_POINT('Ctrl Pts',(-0.00196600887230118,-0.0350360251620521,
-0.0117835285781764));
#43444=CARTESIAN_POINT('Ctrl Pts',(-0.00198996515492455,-0.0350519731611638,
-0.0119697260665178));
#43445=CARTESIAN_POINT('Ctrl Pts',(-0.00199445707108768,-0.035056157491469,
-0.0120190370210945));
#43446=CARTESIAN_POINT('Ctrl Pts',(-0.00199903654565857,-0.0350632737818721,
-0.0121042034331366));
#43447=CARTESIAN_POINT('Ctrl Pts',(-0.00199999873973495,-0.0350662302741379,
-0.012139988480039));
#43448=CARTESIAN_POINT('Ctrl Pts',(-0.00200000065241236,-0.0350706548672094,
-0.012194366349962));
#43449=CARTESIAN_POINT('Ctrl Pts',(-0.00199974229911636,-0.0350721548928912,
-0.0122129502063218));
#43450=CARTESIAN_POINT('Ctrl Pts',(-0.00199860808936163,-0.0350754121797412,
-0.0122536777462656));
#43451=CARTESIAN_POINT('Ctrl Pts',(-0.00199762321779275,-0.0350771635311815,
-0.0122758160272709));
#43452=CARTESIAN_POINT('Ctrl Pts',(-0.0019934803562801,-0.0350824765634891,
-0.0123435598832444));
#43453=CARTESIAN_POINT('Ctrl Pts',(-0.00198912655141246,-0.0350859825684029,
-0.0123890804093612));
#43454=CARTESIAN_POINT('Ctrl Pts',(-0.0019736725436104,-0.0350950380550717,
-0.0125076150744442));
#43455=CARTESIAN_POINT('Ctrl Pts',(-0.00196008325081081,-0.0351005129899465,
-0.0125802346121602));
#43456=CARTESIAN_POINT('Ctrl Pts',(-0.0019137695678505,-0.035114931685053,
-0.0127692015068076));
#43457=CARTESIAN_POINT('Ctrl Pts',(-0.00187447486150728,-0.0351238520759617,
-0.0128836074782262));
#43458=CARTESIAN_POINT('Ctrl Pts',(-0.00180723040578281,-0.0351364284662211,
-0.0130336581885925));
#43459=CARTESIAN_POINT('Ctrl Pts',(-0.00178805117458491,-0.0351398071943819,
-0.0130729505283266));
#43460=CARTESIAN_POINT('Ctrl Pts',(-0.00175149615408346,-0.0351459238130408,
-0.0131420034616443));
#43461=CARTESIAN_POINT('Ctrl Pts',(-0.00173460920616686,-0.0351486442047253,
-0.0131720036533968));
#43462=CARTESIAN_POINT('Ctrl Pts',(-0.00169568658560429,-0.0351547029606944,
-0.013237157800672));
#43463=CARTESIAN_POINT('Ctrl Pts',(-0.00167331483111333,-0.0351580522666305,
-0.0132720910509075));
#43464=CARTESIAN_POINT('Ctrl Pts',(-0.00158051715943771,-0.0351714607924919,
-0.0134075281256136));
#43465=CARTESIAN_POINT('Ctrl Pts',(-0.00150200227905443,-0.0351818052950829,
-0.0135021401457446));
#43466=CARTESIAN_POINT('Ctrl Pts',(-0.00133778802172592,-0.0352015913119727,
-0.0136666141690022));
#43467=CARTESIAN_POINT('Ctrl Pts',(-0.00125397812454458,-0.0352109749229107,
-0.0137377711810139));
#43468=CARTESIAN_POINT('Ctrl Pts',(-0.00114182175525152,-0.035222384656903,
-0.0138181195134375));
#43469=CARTESIAN_POINT('Ctrl Pts',(-0.00111855024356905,-0.0352246947194777,
-0.0138340573963449));
#43470=CARTESIAN_POINT('Ctrl Pts',(-0.00107838833744979,-0.0352285756230006,
-0.0138603324864408));
#43471=CARTESIAN_POINT('Ctrl Pts',(-0.00106166919308336,-0.0352301604434166,
-0.0138709197193575));
#43472=CARTESIAN_POINT('Ctrl Pts',(-0.00102158310188005,-0.0352338884136959,
-0.0138954779170239));
#43473=CARTESIAN_POINT('Ctrl Pts',(-0.000998083357425043,-0.0352360184463566,
-0.0139092230484048));
#43474=CARTESIAN_POINT('Ctrl Pts',(-0.000889279314656027,-0.0352456650693163,
-0.0139699162735517));
#43475=CARTESIAN_POINT('Ctrl Pts',(-0.000800888487752885,-0.0352529103857152,
-0.0140110813988215));
#43476=CARTESIAN_POINT('Ctrl Pts',(-0.000586615777225301,-0.0352699090418459,
-0.0140924269270901));
#43477=CARTESIAN_POINT('Ctrl Pts',(-0.000459081788695746,-0.0352796175782822,
-0.0141269073572777));
#43478=CARTESIAN_POINT('Ctrl Pts',(-0.000286248237428606,-0.0352930338543174,
-0.0141557392557054));
#43479=CARTESIAN_POINT('Ctrl Pts',(-0.000243188114020568,-0.0352963945638124,
-0.0141614880783893));
#43480=CARTESIAN_POINT('Ctrl Pts',(-0.000165713831305937,-0.0353024965358647,
-0.0141692736644648));
#43481=CARTESIAN_POINT('Ctrl Pts',(-0.000131368843978521,-0.0353052208480643,
-0.0141718311962366));
#43482=CARTESIAN_POINT('Ctrl Pts',(-5.45483947135336E-5,-0.0353113669895284,
-0.0141755604897042));
#43483=CARTESIAN_POINT('Ctrl Pts',(-1.20684192265568E-5,-0.0353148015805928,
-0.014176267802333));
#43484=CARTESIAN_POINT('Ctrl Pts',(7.83048016157863E-5,-0.0353221937572267,
-0.0141748940247873));
#43485=CARTESIAN_POINT('Ctrl Pts',(0.000126165274681745,-0.0353261597189562,
-0.0141724446682545));
#43486=CARTESIAN_POINT('Ctrl Pts',(0.00027393749543109,-0.0353385616109294,
-0.0141595479101425));
#43487=CARTESIAN_POINT('Ctrl Pts',(0.000373179803022596,-0.0353471219346769,
-0.0141432932043279));
#43488=CARTESIAN_POINT('Ctrl Pts',(0.000548378756239798,-0.035362467552961,
-0.0141008615326838));
#43489=CARTESIAN_POINT('Ctrl Pts',(0.000624797031384798,-0.0353692413967702,
-0.0140774334156359));
#43490=CARTESIAN_POINT('Ctrl Pts',(0.000726573730253065,-0.0353782323347577,
-0.014039430136805));
#43491=CARTESIAN_POINT('Ctrl Pts',(0.000753313452461783,-0.0353805911473329,
-0.0140287826303499));
#43492=CARTESIAN_POINT('Ctrl Pts',(0.000798070260597117,-0.0353845234895327,
-0.0140098316993986));
#43493=CARTESIAN_POINT('Ctrl Pts',(0.00081620873945973,-0.0353861120986209,
-0.0140018314816055));
#43494=CARTESIAN_POINT('Ctrl Pts',(0.000858565343023737,-0.0353898098612445,
-0.0139823921396538));
#43495=CARTESIAN_POINT('Ctrl Pts',(0.000882677875008957,-0.0353919068556627,
-0.0139707340770382));
#43496=CARTESIAN_POINT('Ctrl Pts',(0.000994736329718761,-0.0354016484619153,
-0.0139137506661006));
#43497=CARTESIAN_POINT('Ctrl Pts',(0.001079485148541,-0.0354090088379031,
-0.0138624192183537));
#43498=CARTESIAN_POINT('Ctrl Pts',(0.00126680944704866,-0.0354260636087769,
-0.013729029416039));
#43499=CARTESIAN_POINT('Ctrl Pts',(0.00136578886684921,-0.0354357153013449,
-0.0136427474726699));
#43500=CARTESIAN_POINT('Ctrl Pts',(0.00148544052246622,-0.0354490731896195,
-0.0135157628432833));
#43501=CARTESIAN_POINT('Ctrl Pts',(0.00151422094899876,-0.0354524377619177,
-0.0134831503312042));
#43502=CARTESIAN_POINT('Ctrl Pts',(0.00156383602610512,-0.0354585423023707,
-0.0134230909067011));
#43503=CARTESIAN_POINT('Ctrl Pts',(0.0015850681169543,-0.0354612651874825,
-0.0133959940877483));
#43504=CARTESIAN_POINT('Ctrl Pts',(0.00163086033395229,-0.0354674020236707,
-0.0133343397489836));
#43505=CARTESIAN_POINT('Ctrl Pts',(0.00165504141611922,-0.035470828589713,
-0.0132995230256753));
#43506=CARTESIAN_POINT('Ctrl Pts',(0.00170407702405112,-0.0354781992810384,
-0.0132238999679976));
#43507=CARTESIAN_POINT('Ctrl Pts',(0.00172861195724907,-0.0354821516636666,
-0.0131829185097587));
#43508=CARTESIAN_POINT('Ctrl Pts',(0.00179973977550545,-0.0354944722425904,
-0.0130538414235223));
#43509=CARTESIAN_POINT('Ctrl Pts',(0.00184123316714173,-0.0355029629885641,
-0.0129631167484504));
#43510=CARTESIAN_POINT('Ctrl Pts',(0.00190616342975048,-0.0355188990899091,
-0.0127875767393077));
#43511=CARTESIAN_POINT('Ctrl Pts',(0.00193111423094824,-0.0355263276072942,
-0.0127035516828114));
#43512=CARTESIAN_POINT('Ctrl Pts',(0.00195615753835482,-0.03553565914942,
-0.0125931144816554));
#43513=CARTESIAN_POINT('Ctrl Pts',(0.00196135334137623,-0.0355377554687445,
-0.0125679661213739));
#43514=CARTESIAN_POINT('Ctrl Pts',(0.00196970595692743,-0.0355414285559199,
-0.0125232042463192));
#43515=CARTESIAN_POINT('Ctrl Pts',(0.001973057165011,-0.0355430142357201,
-0.0125036333072206));
#43516=CARTESIAN_POINT('Ctrl Pts',(0.00197923994578229,-0.0355461881986183,
-0.0124639853683421));
#43517=CARTESIAN_POINT('Ctrl Pts',(0.00198205861943998,-0.0355477760296057,
-0.0124439103299233));
#43518=CARTESIAN_POINT('Ctrl Pts',(0.00198821423343565,-0.0355516338130169,
-0.0123946396116975));
#43519=CARTESIAN_POINT('Ctrl Pts',(0.00199121403430999,-0.0355538891471154,
-0.0123654058551468));
#43520=CARTESIAN_POINT('Ctrl Pts',(0.00199783185008784,-0.0355601727511544,
-0.0122830837495095));
#43521=CARTESIAN_POINT('Ctrl Pts',(0.00199997753046282,-0.0355641540731492,
-0.0122299001841672));
#43522=CARTESIAN_POINT('Ctrl Pts',(0.00199999982444772,-0.0355681130672164,
-0.0121766912657388));
#43523=CARTESIAN_POINT('Ctrl Pts',(0.00191,-0.0443987743898723,-0.0121758532865581));
#43524=CARTESIAN_POINT('Ctrl Pts',(0.00191,-0.0443987743898723,-0.0116043826229051));
#43525=CARTESIAN_POINT('Ctrl Pts',(0.00136396443998201,-0.0443987743898723,
-0.0104664461719892));
#43526=CARTESIAN_POINT('Ctrl Pts',(-0.000486154511932736,-0.0443987743898723,
-0.0100448167983067));
#43527=CARTESIAN_POINT('Ctrl Pts',(-0.00197136971063077,-0.0443987743898723,
-0.0112269996519921));
#43528=CARTESIAN_POINT('Ctrl Pts',(-0.00196863290544544,-0.0443987743898723,
-0.0131236113412357));
#43529=CARTESIAN_POINT('Ctrl Pts',(-0.00048737056446968,-0.0443987743898723,
-0.014309575135295));
#43530=CARTESIAN_POINT('Ctrl Pts',(0.00136372235516645,-0.0443987743898723,
-0.0138834315669214));
#43531=CARTESIAN_POINT('Ctrl Pts',(0.00191,-0.0443987743898723,-0.0127473239502111));
#43532=CARTESIAN_POINT('Ctrl Pts',(0.00191,-0.0443987743898723,-0.0121758532865581));
#43533=CARTESIAN_POINT('Ctrl Pts',(0.00192589648945146,-0.0443775790706037,
-0.0121758532865581));
#43534=CARTESIAN_POINT('Ctrl Pts',(0.00192589648945146,-0.0443775790706037,
-0.0115996618695963));
#43535=CARTESIAN_POINT('Ctrl Pts',(0.00137530035187607,-0.0443775790706037,
-0.0104522100376602));
#43536=CARTESIAN_POINT('Ctrl Pts',(-0.00049019929686441,-0.0443775790706037,
-0.0100270915893122));
#43537=CARTESIAN_POINT('Ctrl Pts',(-0.001987759617862,-0.0443775790706037,
-0.0112191030790215));
#43538=CARTESIAN_POINT('Ctrl Pts',(-0.00198501905754235,-0.0443775790706037,
-0.0131315055658264));
#43539=CARTESIAN_POINT('Ctrl Pts',(-0.000491417921724576,-0.0443775790706037,
-0.0143273048600502));
#43540=CARTESIAN_POINT('Ctrl Pts',(0.00137506056245648,-0.0443775790706037,
-0.0138976640310167));
#43541=CARTESIAN_POINT('Ctrl Pts',(0.00192589648945146,-0.0443775790706037,
-0.0127520447035199));
#43542=CARTESIAN_POINT('Ctrl Pts',(0.00192589648945146,-0.0443775790706037,
-0.0121758532865581));
#43543=CARTESIAN_POINT('Ctrl Pts',(0.00195438855983192,-0.0443409009516712,
-0.0121758532865581));
#43544=CARTESIAN_POINT('Ctrl Pts',(0.00195438855983192,-0.0443409009516712,
-0.0115910921262162));
#43545=CARTESIAN_POINT('Ctrl Pts',(0.00139566737358033,-0.0443409009516712,
-0.0104267218465327));
#43546=CARTESIAN_POINT('Ctrl Pts',(-0.000497453148499854,-0.0443409009516712,
-0.00999528841693408));
#43547=CARTESIAN_POINT('Ctrl Pts',(-0.00201718914033432,-0.0443409009516712,
-0.0112049480760704));
#43548=CARTESIAN_POINT('Ctrl Pts',(-0.00201438365174801,-0.0443409009516711,
-0.0131456356479581));
#43549=CARTESIAN_POINT('Ctrl Pts',(-0.000498699477980959,-0.0443409009516712,
-0.0143591706870349));
#43550=CARTESIAN_POINT('Ctrl Pts',(0.00139541851169272,-0.0443409009516711,
-0.0139231103056061));
#43551=CARTESIAN_POINT('Ctrl Pts',(0.00195438855983192,-0.0443409009516712,
-0.0127606144469));
#43552=CARTESIAN_POINT('Ctrl Pts',(0.00195438855983192,-0.0443409009516712,
-0.0121758532865581));
#43553=CARTESIAN_POINT('Ctrl Pts',(0.00201714899795489,-0.0442974094567112,
-0.0121758532865581));
#43554=CARTESIAN_POINT('Ctrl Pts',(0.00201714899795489,-0.0442974094567112,
-0.0115723431648622));
#43555=CARTESIAN_POINT('Ctrl Pts',(0.00144047261468403,-0.0442974094567112,
-0.0103705452165039));
#43556=CARTESIAN_POINT('Ctrl Pts',(-0.000513426520915583,-0.0442974094567112,
-0.00992527387087597));
#43557=CARTESIAN_POINT('Ctrl Pts',(-0.00208195197224179,-0.0442974094567112,
-0.0111737702411527));
#43558=CARTESIAN_POINT('Ctrl Pts',(-0.00207907206613982,-0.0442974094567112,
-0.0131767830034219));
#43559=CARTESIAN_POINT('Ctrl Pts',(-0.000514706653486131,-0.0442974094567112,
-0.0144292589295152));
#43560=CARTESIAN_POINT('Ctrl Pts',(0.00144021931264795,-0.0442974094567112,
-0.0139792362605124));
#43561=CARTESIAN_POINT('Ctrl Pts',(0.00201714899795489,-0.0442974094567112,
-0.0127793634082539));
#43562=CARTESIAN_POINT('Ctrl Pts',(0.00201714899795489,-0.0442974094567112,
-0.0121758532865581));
#43563=CARTESIAN_POINT('Ctrl Pts',(0.00208712894978359,-0.0442779545242776,
-0.0121758532865581));
#43564=CARTESIAN_POINT('Ctrl Pts',(0.00208712894978359,-0.0442779545242776,
-0.0115513687696672));
#43565=CARTESIAN_POINT('Ctrl Pts',(0.00149046301531559,-0.0442779545242776,
-0.0103079241157742));
#43566=CARTESIAN_POINT('Ctrl Pts',(-0.000531240003705059,-0.0442779545242776,
-0.00984718420843915));
#43567=CARTESIAN_POINT('Ctrl Pts',(-0.00215419825785711,-0.0442779545242776,
-0.0111390049289695));
#43568=CARTESIAN_POINT('Ctrl Pts',(-0.00215119853182699,-0.0442779545242776,
-0.0132115012185179));
#43569=CARTESIAN_POINT('Ctrl Pts',(-0.000532572447509192,-0.0442779545242776,
-0.0145074653054627));
#43570=CARTESIAN_POINT('Ctrl Pts',(0.00149019641460847,-0.0442779545242776,
-0.0140417784860521));
#43571=CARTESIAN_POINT('Ctrl Pts',(0.00208712894978359,-0.0442779545242776,
-0.012800337803449));
#43572=CARTESIAN_POINT('Ctrl Pts',(0.00208712894978359,-0.0442779545242776,
-0.0121758532865581));
#43573=CARTESIAN_POINT('Ctrl Pts',(0.00213650829037307,-0.0442788253127506,
-0.0121758532865581));
#43574=CARTESIAN_POINT('Ctrl Pts',(0.00213650829037307,-0.0442788253127506,
-0.0115366660068379));
#43575=CARTESIAN_POINT('Ctrl Pts',(0.00152569330952636,-0.0442788253127506,
-0.0102637123012538));
#43576=CARTESIAN_POINT('Ctrl Pts',(-0.000543805828570658,-0.0442788253127506,
-0.00979211240677498));
#43577=CARTESIAN_POINT('Ctrl Pts',(-0.00220512921753389,-0.0442788253127506,
-0.0111144752032848));
#43578=CARTESIAN_POINT('Ctrl Pts',(-0.00220209708826565,-0.0442788253127506,
-0.0132360162688478));
#43579=CARTESIAN_POINT('Ctrl Pts',(-0.000545154492334908,-0.0442788253127506,
-0.0145625705770762));
#43580=CARTESIAN_POINT('Ctrl Pts',(0.00152542913999413,-0.0442788253127506,
-0.0140859663070167));
#43581=CARTESIAN_POINT('Ctrl Pts',(0.00213650829037307,-0.0442788253127506,
-0.0128150405662783));
#43582=CARTESIAN_POINT('Ctrl Pts',(0.00213650829037307,-0.0442788253127506,
-0.0121758532865581));
#43583=CARTESIAN_POINT('Ctrl Pts',(0.00215960599488205,-0.0442787671797737,
-0.0121758532865581));
#43584=CARTESIAN_POINT('Ctrl Pts',(0.00215960599488205,-0.0442787671797737,
-0.0115296726592007));
#43585=CARTESIAN_POINT('Ctrl Pts',(0.00154222513336241,-0.0442787671797737,
-0.0102430616280669));
#43586=CARTESIAN_POINT('Ctrl Pts',(-0.000549688095030464,-0.0442787671797737,
-0.00976631629653212));
#43587=CARTESIAN_POINT('Ctrl Pts',(-0.0022290094390271,-0.0442787671797737,
-0.0111029994762258));
#43588=CARTESIAN_POINT('Ctrl Pts',(-0.00222589994608779,-0.0442787671797737,
-0.0132474629929249));
#43589=CARTESIAN_POINT('Ctrl Pts',(-0.000551069030812133,-0.0442787671797737,
-0.0145884406624534));
#43590=CARTESIAN_POINT('Ctrl Pts',(0.00154194800605399,-0.0442787671797737,
-0.0141065679844921));
#43591=CARTESIAN_POINT('Ctrl Pts',(0.00215960599488205,-0.0442787671797737,
-0.0128220339139153));
#43592=CARTESIAN_POINT('Ctrl Pts',(0.00215960599488205,-0.0442787671797737,
-0.0121758532865581));
#43593=CARTESIAN_POINT('Ctrl Pts',(-0.00190884695647825,-0.0443979099380992,
-0.0121758537542897));
#43594=CARTESIAN_POINT('Ctrl Pts',(-0.0019086387602771,-0.0443977537577689,
-0.0124605928222598));
#43595=CARTESIAN_POINT('Ctrl Pts',(-0.00184659890197118,-0.0443980578198581,
-0.0127480326817812));
#43596=CARTESIAN_POINT('Ctrl Pts',(-0.00162944389721798,-0.0443983362855908,
-0.0131986267652795));
#43597=CARTESIAN_POINT('Ctrl Pts',(-0.00150149968284053,-0.0443983738682118,
-0.0133748516475149));
#43598=CARTESIAN_POINT('Ctrl Pts',(-0.00109784916003133,-0.0443975727756485,
-0.0137769070334325));
#43599=CARTESIAN_POINT('Ctrl Pts',(-0.00077347669762607,-0.0443981434538313,
-0.0139620860896191));
#43600=CARTESIAN_POINT('Ctrl Pts',(-0.000286256574005507,-0.0443982288725065,
-0.0140731128679073));
#43601=CARTESIAN_POINT('Ctrl Pts',(-0.000142992270597617,-0.0443981711685123,
-0.0140879545366855));
#43602=CARTESIAN_POINT('Ctrl Pts',(0.000427615134630929,-0.0443972050126916,
-0.0140840813965754));
#43603=CARTESIAN_POINT('Ctrl Pts',(0.000857946456805267,-0.0443983417280292,
-0.0139371451114233));
#43604=CARTESIAN_POINT('Ctrl Pts',(0.00124787970615935,-0.044398339904063,
-0.0136260912098367));
#43605=CARTESIAN_POINT('Ctrl Pts',(0.00130109284701091,-0.0443983077589567,
-0.0135781506662894));
#43606=CARTESIAN_POINT('Ctrl Pts',(0.00170253954223259,-0.0443976850210757,
-0.0131724039571971));
#43607=CARTESIAN_POINT('Ctrl Pts',(0.00191,-0.0443987743898723,-0.0126747526877388));
#43608=CARTESIAN_POINT('Ctrl Pts',(0.00191,-0.0443987743898723,-0.0121758532865581));
#43609=CARTESIAN_POINT('Origin',(0.,-0.0442787743898823,-0.0121758532865581));
#43610=CARTESIAN_POINT('Origin',(0.,-0.0442787743898723,-0.0121758532865581));
#43611=CARTESIAN_POINT('',(0.00379145188432738,-0.0442787743898723,-0.0117428405846659));
#43612=CARTESIAN_POINT('',(0.00379145188432738,-0.0442787743898723,-0.0126088659884503));
#43613=CARTESIAN_POINT('',(0.00379145188433738,-0.0442787743898823,-0.0121758532865681));
#43614=CARTESIAN_POINT('',(0.00227072594216369,-0.0442787743898723,-0.00910886598845032));
#43615=CARTESIAN_POINT('',(0.00404145188433738,-0.0442787743898823,-0.0121758532865681));
#43616=CARTESIAN_POINT('',(0.00152072594216369,-0.0442787743898723,-0.0086758532865581));
#43617=CARTESIAN_POINT('',(0.00189572594217369,-0.0442787743898823,-0.00889235963749421));
#43618=CARTESIAN_POINT('',(-0.00152072594216369,-0.0442787743898723,-0.0086758532865581));
#43619=CARTESIAN_POINT('',(0.00202072594217369,-0.0442787743898823,-0.0086758532865481));
#43620=CARTESIAN_POINT('',(-0.00227072594216369,-0.0442787743898723,-0.00910886598845032));
#43621=CARTESIAN_POINT('',(-0.00189572594217369,-0.0442787743898823,-0.00889235963749421));
#43622=CARTESIAN_POINT('',(-0.00379145188432738,-0.0442787743898723,-0.0117428405846659));
#43623=CARTESIAN_POINT('',(-0.00202072594217369,-0.0442787743898823,-0.0086758532865481));
#43624=CARTESIAN_POINT('',(-0.00379145188432738,-0.0442787743898723,-0.0126088659884503));
#43625=CARTESIAN_POINT('',(-0.00379145188433738,-0.0442787743898823,-0.0121758532865481));
#43626=CARTESIAN_POINT('',(-0.00227072594216369,-0.0442787743898723,-0.0152428405846659));
#43627=CARTESIAN_POINT('',(-0.00404145188433738,-0.0442787743898823,-0.0121758532865481));
#43628=CARTESIAN_POINT('',(-0.0015207259421637,-0.0442787743898723,-0.0156758532865581));
#43629=CARTESIAN_POINT('',(-0.0018957259421737,-0.0442787743898823,-0.015459346935622));
#43630=CARTESIAN_POINT('',(0.00152072594216369,-0.0442787743898723,-0.0156758532865581));
#43631=CARTESIAN_POINT('',(-0.00202072594217369,-0.0442787743898823,-0.0156758532865681));
#43632=CARTESIAN_POINT('',(0.00227072594216369,-0.0442787743898723,-0.0152428405846659));
#43633=CARTESIAN_POINT('',(0.0018957259421737,-0.0442787743898823,-0.015459346935622));
#43634=CARTESIAN_POINT('',(0.00202072594217369,-0.0442787743898823,-0.0156758532865681));
#43635=CARTESIAN_POINT('Origin',(0.,-0.0452787743898723,-0.0121758532865581));
#43636=CARTESIAN_POINT('',(0.000499999999998797,-0.0462787743898739,-0.0121758532865581));
#43637=CARTESIAN_POINT('',(0.00125,-0.0452787743898723,-0.0121758532865581));
#43638=CARTESIAN_POINT('Origin',(0.,-0.0462787743898823,-0.0121758532865581));
#43639=CARTESIAN_POINT('Origin',(0.00389145188432738,-0.0441787743898723,
-0.0121758532865581));
#43640=CARTESIAN_POINT('',(0.00399145188432738,-0.0440787743898723,-0.0122624558269365));
#43641=CARTESIAN_POINT('',(0.00347816150747191,-0.0445920647667478,-0.0131515008387137));
#43642=CARTESIAN_POINT('',(0.00399145188432738,-0.0440787743898723,-0.0120892507461797));
#43643=CARTESIAN_POINT('',(0.00399145188433738,-0.0440787743898823,-0.0121758532865681));
#43644=CARTESIAN_POINT('',(0.00428645188433738,-0.0437837743898823,-0.0126002057344225));
#43645=CARTESIAN_POINT('Origin',(0.00202072594216369,-0.0412787743898723,
-0.0156758532865581));
#43646=CARTESIAN_POINT('',(0.00207072594216369,-0.0440787743898723,-0.0155892507461796));
#43647=CARTESIAN_POINT('',(0.00177572594217369,-0.0437837743898823,-0.0161002057344224));
#43648=CARTESIAN_POINT('',(0.00207072594216369,-0.0414787743898723,-0.0155892507461796));
#43649=CARTESIAN_POINT('',(0.00207072594217369,-0.0412787743898823,-0.0155892507461896));
#43650=CARTESIAN_POINT('',(0.00227072594216369,-0.0412787743898723,-0.0152428405846659));
#43651=CARTESIAN_POINT('',(0.00207572594217369,-0.0414737743898823,-0.0155805904921518));
#43652=CARTESIAN_POINT('',(0.00379145188432738,-0.0412787743898723,-0.0126088659884503));
#43653=CARTESIAN_POINT('',(0.00202072594217369,-0.0412787743898823,-0.0156758532865681));
#43654=CARTESIAN_POINT('',(0.00399145188432738,-0.0414787743898723,-0.0122624558269365));
#43655=CARTESIAN_POINT('',(0.0031781615074719,-0.0406654840130169,-0.0136711160809844));
#43656=CARTESIAN_POINT('',(0.00399145188433738,-0.0412787743898823,-0.0122624558269465));
#43657=CARTESIAN_POINT('',(0.00265608891323529,-0.0427787743898723,-0.0145753723394213));
#43658=CARTESIAN_POINT('Origin',(0.00303108891325554,-0.0427787743898823,
-0.0139258532865681));
#43659=CARTESIAN_POINT('Origin',(0.00194572594216369,-0.0441787743898723,
-0.00880575709712576));
#43660=CARTESIAN_POINT('',(0.00207072594216369,-0.0440787743898723,-0.00876245582693654));
#43661=CARTESIAN_POINT('',(0.00258401631903916,-0.0445920647667478,-0.00965150083869371));
#43662=CARTESIAN_POINT('',(0.00192072594216369,-0.0440787743898723,-0.0086758532865581));
#43663=CARTESIAN_POINT('',(0.00199572594217369,-0.0440787743898823,-0.00871915455673732));
#43664=CARTESIAN_POINT('',(0.00251072594217369,-0.0437837743898823,-0.0086758532865481));
#43665=CARTESIAN_POINT('Origin',(0.00202072594216369,-0.0412787743898723,
-0.0086758532865581));
#43666=CARTESIAN_POINT('',(0.00192072594216369,-0.0414787743898723,-0.0086758532865581));
#43667=CARTESIAN_POINT('',(0.00192072594217369,-0.0412787743898823,-0.0086758532865481));
#43668=CARTESIAN_POINT('',(0.00152072594216369,-0.0412787743898723,-0.0086758532865581));
#43669=CARTESIAN_POINT('',(0.00191072594217369,-0.0414737743898823,-0.0086758532865481));
#43670=CARTESIAN_POINT('',(-0.00152072594216369,-0.0412787743898723,-0.0086758532865581));
#43671=CARTESIAN_POINT('',(0.00202072594217369,-0.0412787743898823,-0.0086758532865481));
#43672=CARTESIAN_POINT('',(-0.00192072594216369,-0.0414787743898723,-0.0086758532865581));
#43673=CARTESIAN_POINT('',(-0.000294145188442734,-0.0406654840130169,-0.0086758532865481));
#43674=CARTESIAN_POINT('',(-0.00192072594216369,-0.0440787743898723,-0.0086758532865581));
#43675=CARTESIAN_POINT('',(-0.00192072594217369,-0.0412787743898823,-0.0086758532865481));
#43676=CARTESIAN_POINT('',(-0.000894145188442733,-0.0445920647667478,-0.0086758532865481));
#43677=CARTESIAN_POINT('',(0.000750000000026109,-0.0427787743898723,-0.00867585328655462));
#43678=CARTESIAN_POINT('Origin',(1.00022748892833E-14,-0.0427787743898823,
-0.0086758532865481));
#43679=CARTESIAN_POINT('Origin',(-0.00194572594216369,-0.0441787743898723,
-0.00880575709712576));
#43680=CARTESIAN_POINT('',(-0.00207072594216369,-0.0440787743898723,-0.00876245582693654));
#43681=CARTESIAN_POINT('',(-0.00199572594217369,-0.0440787743898823,-0.00871915455673732));
#43682=CARTESIAN_POINT('',(-0.00177572594217369,-0.0437837743898823,-0.00825150083869372));
#43683=CARTESIAN_POINT('Origin',(-0.00389145188432738,-0.0441787743898723,
-0.0121758532865581));
#43684=CARTESIAN_POINT('',(-0.00399145188432738,-0.0440787743898723,-0.0120892507461797));
#43685=CARTESIAN_POINT('',(-0.00347816150747191,-0.0445920647667478,-0.0112002057344025));
#43686=CARTESIAN_POINT('',(-0.00399145188432738,-0.0440787743898723,-0.0122624558269365));
#43687=CARTESIAN_POINT('',(-0.00399145188433738,-0.0440787743898823,-0.0121758532865481));
#43688=CARTESIAN_POINT('',(-0.00428645188433738,-0.0437837743898823,-0.0117515008386937));
#43689=CARTESIAN_POINT('Origin',(-0.00404145188432738,-0.0412787743898723,
-0.0121758532865581));
#43690=CARTESIAN_POINT('',(-0.00399145188432738,-0.0414787743898723,-0.0122624558269365));
#43691=CARTESIAN_POINT('',(-0.00399145188433738,-0.0412787743898823,-0.0122624558269465));
#43692=CARTESIAN_POINT('',(-0.00379145188432738,-0.0412787743898723,-0.0126088659884503));
#43693=CARTESIAN_POINT('',(-0.00398645188433738,-0.0414737743898823,-0.0122711160809844));
#43694=CARTESIAN_POINT('',(-0.00227072594216369,-0.0412787743898723,-0.0152428405846659));
#43695=CARTESIAN_POINT('',(-0.00404145188433738,-0.0412787743898823,-0.0121758532865481));
#43696=CARTESIAN_POINT('',(-0.00207072594216369,-0.0414787743898723,-0.0155892507461796));
#43697=CARTESIAN_POINT('',(-0.00288401631903917,-0.0406654840130169,-0.0141805904921518));
#43698=CARTESIAN_POINT('',(-0.00207072594216369,-0.0440787743898723,-0.0155892507461796));
#43699=CARTESIAN_POINT('',(-0.00207072594217369,-0.0412787743898823,-0.0155892507461896));
#43700=CARTESIAN_POINT('',(-0.00258401631903917,-0.0445920647667478,-0.0147002057344225));
#43701=CARTESIAN_POINT('Origin',(-0.0019457259421637,-0.0441787743898723,
-0.0155459494759905));
#43702=CARTESIAN_POINT('',(-0.00192072594216369,-0.0440787743898723,-0.0156758532865581));
#43703=CARTESIAN_POINT('',(-0.0019957259421737,-0.0440787743898823,-0.0156325520163788));
#43704=CARTESIAN_POINT('',(-0.0025107259421737,-0.0437837743898823,-0.0156758532865681));
#43705=CARTESIAN_POINT('Origin',(0.0019457259421637,-0.0441787743898723,
-0.0155459494759905));
#43706=CARTESIAN_POINT('',(0.00192072594216369,-0.0440787743898723,-0.0156758532865581));
#43707=CARTESIAN_POINT('',(0.00089414518844275,-0.0445920647667478,-0.0156758532865681));
#43708=CARTESIAN_POINT('',(0.0019957259421737,-0.0440787743898823,-0.0156325520163788));
#43709=CARTESIAN_POINT('Origin',(0.0019457259421637,-0.0413787743898723,
-0.0155459494759905));
#43710=CARTESIAN_POINT('',(0.00192072594216369,-0.0414787743898723,-0.0156758532865581));
#43711=CARTESIAN_POINT('',(0.0019957259421737,-0.0414787743898823,-0.0156325520163788));
#43712=CARTESIAN_POINT('',(0.00152072594216369,-0.0412787743898723,-0.0156758532865581));
#43713=CARTESIAN_POINT('',(0.000294145188442746,-0.0406654840130168,-0.0156758532865681));
#43714=CARTESIAN_POINT('',(0.0018957259421737,-0.0412787743898823,-0.015459346935622));
#43715=CARTESIAN_POINT('Origin',(0.,-0.0412787743898723,-0.0121758532865581));
#43716=CARTESIAN_POINT('',(-0.0015207259421637,-0.0412787743898723,-0.0156758532865581));
#43717=CARTESIAN_POINT('',(-0.00202072594217369,-0.0412787743898823,-0.0156758532865681));
#43718=CARTESIAN_POINT('',(-0.0018957259421737,-0.0412787743898823,-0.015459346935622));
#43719=CARTESIAN_POINT('',(-0.00379145188432738,-0.0412787743898723,-0.0117428405846659));
#43720=CARTESIAN_POINT('',(-0.00379145188433738,-0.0412787743898823,-0.0121758532865481));
#43721=CARTESIAN_POINT('',(-0.00227072594216369,-0.0412787743898723,-0.00910886598845032));
#43722=CARTESIAN_POINT('',(-0.00202072594217369,-0.0412787743898823,-0.0086758532865481));
#43723=CARTESIAN_POINT('',(-0.00189572594217369,-0.0412787743898823,-0.00889235963749421));
#43724=CARTESIAN_POINT('',(0.00227072594216369,-0.0412787743898723,-0.00910886598845032));
#43725=CARTESIAN_POINT('',(0.00189572594217369,-0.0412787743898823,-0.00889235963749421));
#43726=CARTESIAN_POINT('',(0.00379145188432738,-0.0412787743898723,-0.0117428405846659));
#43727=CARTESIAN_POINT('',(0.00404145188433738,-0.0412787743898823,-0.0121758532865681));
#43728=CARTESIAN_POINT('',(0.00379145188433738,-0.0412787743898823,-0.0121758532865681));
#43729=CARTESIAN_POINT('',(0.00270000000001,-0.0412787743898823,-0.0121758532865581));
#43730=CARTESIAN_POINT('Origin',(5.55111512312578E-19,-0.0412787743898823,
-0.0121758532865581));
#43731=CARTESIAN_POINT('Origin',(-0.0019457259421637,-0.0413787743898723,
-0.0155459494759905));
#43732=CARTESIAN_POINT('',(-0.00192072594216369,-0.0414787743898723,-0.0156758532865581));
#43733=CARTESIAN_POINT('',(-0.00191072594217369,-0.0414737743898823,-0.0156758532865681));
#43734=CARTESIAN_POINT('',(-0.0019957259421737,-0.0414787743898823,-0.0156325520163788));
#43735=CARTESIAN_POINT('Origin',(-0.00389145188432738,-0.0413787743898723,
-0.0121758532865581));
#43736=CARTESIAN_POINT('',(-0.00399145188432738,-0.0414787743898723,-0.0120892507461797));
#43737=CARTESIAN_POINT('',(-0.00399145188433738,-0.0414787743898823,-0.0121758532865481));
#43738=CARTESIAN_POINT('',(-0.0031781615074719,-0.0406654840130169,-0.0106805904921318));
#43739=CARTESIAN_POINT('Origin',(-0.00194572594216369,-0.0413787743898723,
-0.00880575709712576));
#43740=CARTESIAN_POINT('',(-0.00207072594216369,-0.0414787743898723,-0.00876245582693654));
#43741=CARTESIAN_POINT('',(-0.00207572594217369,-0.0414737743898823,-0.00877111608096439));
#43742=CARTESIAN_POINT('',(-0.00199572594217369,-0.0414787743898823,-0.00871915455673732));
#43743=CARTESIAN_POINT('Origin',(0.00194572594216369,-0.0413787743898723,
-0.00880575709712576));
#43744=CARTESIAN_POINT('',(0.00207072594216369,-0.0414787743898723,-0.00876245582693654));
#43745=CARTESIAN_POINT('',(0.00199572594217369,-0.0414787743898823,-0.00871915455673732));
#43746=CARTESIAN_POINT('',(0.00288401631903916,-0.0406654840130168,-0.0101711160809644));
#43747=CARTESIAN_POINT('Origin',(0.00404145188432738,-0.0412787743898723,
-0.0121758532865581));
#43748=CARTESIAN_POINT('',(0.00399145188432738,-0.0414787743898723,-0.0120892507461797));
#43749=CARTESIAN_POINT('',(0.00399145188433738,-0.0412787743898823,-0.0120892507461697));
#43750=CARTESIAN_POINT('',(0.00398645188433738,-0.0414737743898823,-0.0120805904921318));
#43751=CARTESIAN_POINT('',(0.00207072594217369,-0.0412787743898823,-0.00876245582692654));
#43752=CARTESIAN_POINT('',(0.00340608891326195,-0.0427787743898723,-0.0110753723394177));
#43753=CARTESIAN_POINT('Origin',(0.00303108891325554,-0.0427787743898823,
-0.0104258532865481));
#43754=CARTESIAN_POINT('Origin',(0.00199572594216369,-0.0412787743898723,
-0.00871915455674732));
#43755=CARTESIAN_POINT('Origin',(-0.00199572594216369,-0.0412787743898723,
-0.00871915455674732));
#43756=CARTESIAN_POINT('',(-0.00207072594217369,-0.0412787743898823,-0.00876245582692654));
#43757=CARTESIAN_POINT('Origin',(-0.00202072594216369,-0.0412787743898723,
-0.0086758532865581));
#43758=CARTESIAN_POINT('',(-0.00399145188433738,-0.0412787743898823,-0.0120892507461696));
#43759=CARTESIAN_POINT('Origin',(-0.00399145188432738,-0.0412787743898723,
-0.0121758532865581));
#43760=CARTESIAN_POINT('Origin',(-0.00199572594216369,-0.0412787743898723,
-0.0156325520163689));
#43761=CARTESIAN_POINT('',(-0.00192072594217369,-0.0412787743898823,-0.0156758532865681));
#43762=CARTESIAN_POINT('Origin',(-0.00202072594216369,-0.0412787743898723,
-0.0156758532865581));
#43763=CARTESIAN_POINT('',(0.00192072594217369,-0.0412787743898823,-0.0156758532865681));
#43764=CARTESIAN_POINT('Origin',(0.00199572594216369,-0.0412787743898723,
-0.0156325520163689));
#43765=CARTESIAN_POINT('Origin',(0.00389145188432738,-0.0413787743898723,
-0.0121758532865581));
#43766=CARTESIAN_POINT('',(0.00399145188433738,-0.0414787743898823,-0.0121758532865681));
#43767=CARTESIAN_POINT('Origin',(0.00399145188432738,-0.0412787743898723,
-0.0121758532865581));
#43768=CARTESIAN_POINT('Ctrl Pts',(0.00270918054975648,-0.0412787503570556,
-0.0121758532865581));
#43769=CARTESIAN_POINT('Ctrl Pts',(0.00270918054975648,-0.0412787503570556,
-0.0113652728041599));
#43770=CARTESIAN_POINT('Ctrl Pts',(0.00193513294480066,-0.0412787503570556,
-0.00975168114383156));
#43771=CARTESIAN_POINT('Ctrl Pts',(-0.00069000520119527,-0.0412787503570556,
-0.00915299470268466));
#43772=CARTESIAN_POINT('Ctrl Pts',(-0.00279540565516726,-0.0412787503570556,
-0.0108302679555478));
#43773=CARTESIAN_POINT('Ctrl Pts',(-0.00279272352454856,-0.0412787503570556,
-0.0135201078666651));
#43774=CARTESIAN_POINT('Ctrl Pts',(-0.000690883461576721,-0.0412787503570556,
-0.0152020993353227));
#43775=CARTESIAN_POINT('Ctrl Pts',(0.00193418739257031,-0.0412787503570556,
-0.01459810269407));
#43776=CARTESIAN_POINT('Ctrl Pts',(0.00270918054975648,-0.0412787503570556,
-0.0129864337689563));
#43777=CARTESIAN_POINT('Ctrl Pts',(0.00270918054975648,-0.0412787503570556,
-0.0121758532865581));
#43778=CARTESIAN_POINT('Ctrl Pts',(0.00267614195234609,-0.0412788886794323,
-0.0121758532865581));
#43779=CARTESIAN_POINT('Ctrl Pts',(0.00267614195234609,-0.0412788886794323,
-0.0113751391161252));
#43780=CARTESIAN_POINT('Ctrl Pts',(0.00191154067064816,-0.0412788886794323,
-0.00978125017196854));
#43781=CARTESIAN_POINT('Ctrl Pts',(-0.000681589977327022,-0.0412788886794323,
-0.00918985318007107));
#43782=CARTESIAN_POINT('Ctrl Pts',(-0.00276132283802881,-0.0412788886794323,
-0.0108466776255854));
#43783=CARTESIAN_POINT('Ctrl Pts',(-0.00275866480260235,-0.0412788886794323,
-0.013503712356313));
#43784=CARTESIAN_POINT('Ctrl Pts',(-0.000682462010447489,-0.0412788886794323,
-0.0151652074941981));
#43785=CARTESIAN_POINT('Ctrl Pts',(0.00191060490329316,-0.0412788886794323,
-0.014568552060673));
#43786=CARTESIAN_POINT('Ctrl Pts',(0.00267614195234609,-0.0412788886794323,
-0.012976567456991));
#43787=CARTESIAN_POINT('Ctrl Pts',(0.00267614195234609,-0.0412788886794323,
-0.0121758532865581));
#43788=CARTESIAN_POINT('Ctrl Pts',(0.00261368928777976,-0.0412787942793926,
-0.0121758532865581));
#43789=CARTESIAN_POINT('Ctrl Pts',(0.00261368928777976,-0.0412787942793926,
-0.0113938502436242));
#43790=CARTESIAN_POINT('Ctrl Pts',(0.00186692234954223,-0.0412787942793926,
-0.00983712445344849));
#43791=CARTESIAN_POINT('Ctrl Pts',(-0.000665684594985857,-0.0412787942793926,
-0.00925954420041668));
#43792=CARTESIAN_POINT('Ctrl Pts',(-0.00269687259383373,-0.0412787942793926,
-0.0108776961201086));
#43793=CARTESIAN_POINT('Ctrl Pts',(-0.00269428806701916,-0.0412787942793926,
-0.0134727273438823));
#43794=CARTESIAN_POINT('Ctrl Pts',(-0.000666530303291745,-0.0412787942793926,
-0.0150954276100709));
#43795=CARTESIAN_POINT('Ctrl Pts',(0.00186601074701434,-0.0412787942793926,
-0.0145127289543036));
#43796=CARTESIAN_POINT('Ctrl Pts',(0.00261368928777976,-0.0412787942793926,
-0.012957856329492));
#43797=CARTESIAN_POINT('Ctrl Pts',(0.00261368928777976,-0.0412787942793926,
-0.0121758532865581));
#43798=CARTESIAN_POINT('Ctrl Pts',(0.00253433766292927,-0.0412183037740197,
-0.0121758532865581));
#43799=CARTESIAN_POINT('Ctrl Pts',(0.00253433766292927,-0.0412183037740197,
-0.0114175510782768));
#43800=CARTESIAN_POINT('Ctrl Pts',(0.00181025729792705,-0.0412183037740197,
-0.00990814158877628));
#43801=CARTESIAN_POINT('Ctrl Pts',(-0.000645473156809493,-0.0412183037740197,
-0.00934807153777405));
#43802=CARTESIAN_POINT('Ctrl Pts',(-0.00261501139357923,-0.0412183037740197,
-0.0109171085874015));
#43803=CARTESIAN_POINT('Ctrl Pts',(-0.00261248660679668,-0.0412183037740197,
-0.0134333493339249));
#43804=CARTESIAN_POINT('Ctrl Pts',(-0.000646302936028143,-0.0412183037740197,
-0.0150068184163061));
#43805=CARTESIAN_POINT('Ctrl Pts',(0.00180936957537367,-0.0412183037740197,
-0.0144417570953774));
#43806=CARTESIAN_POINT('Ctrl Pts',(0.00253433766292927,-0.0412183037740197,
-0.0129341554948394));
#43807=CARTESIAN_POINT('Ctrl Pts',(0.00253433766292927,-0.0412183037740197,
-0.0121758532865581));
#43808=CARTESIAN_POINT('Ctrl Pts',(0.00250057355266071,-0.0411453162532137,
-0.0121758532865581));
#43809=CARTESIAN_POINT('Ctrl Pts',(0.00250057355266071,-0.0411453162532137,
-0.011427734754967));
#43810=CARTESIAN_POINT('Ctrl Pts',(0.00178611059073584,-0.0411453162532137,
-0.00993832706908355));
#43811=CARTESIAN_POINT('Ctrl Pts',(-0.000636876223173571,-0.0411453162532137,
-0.00938576861420257));
#43812=CARTESIAN_POINT('Ctrl Pts',(-0.00258014094469067,-0.0411453162532137,
-0.0109338776021103));
#43813=CARTESIAN_POINT('Ctrl Pts',(-0.00257768702246746,-0.0411453162532137,
-0.0134166058963254));
#43814=CARTESIAN_POINT('Ctrl Pts',(-0.00063767557125981,-0.0411453162532137,
-0.014969044583688));
#43815=CARTESIAN_POINT('Ctrl Pts',(0.00178524224201209,-0.0411453162532137,
-0.0144116175405293));
#43816=CARTESIAN_POINT('Ctrl Pts',(0.00250057355266071,-0.0411453162532137,
-0.0129239718181492));
#43817=CARTESIAN_POINT('Ctrl Pts',(0.00250057355266071,-0.0411453162532137,
-0.0121758532865581));
#43818=CARTESIAN_POINT('Ctrl Pts',(0.0025,-0.041101214337398,-0.0121758532865581));
#43819=CARTESIAN_POINT('Ctrl Pts',(0.0025,-0.041101214337398,-0.0114277797728648));
#43820=CARTESIAN_POINT('Ctrl Pts',(0.00178574661104337,-0.041101214337398,
-0.00993888160219718));
#43821=CARTESIAN_POINT('Ctrl Pts',(-0.000636726266562143,-0.041101214337398,
-0.00938637186566609));
#43822=CARTESIAN_POINT('Ctrl Pts',(-0.0025795983978868,-0.041101214337398,
-0.0109341637345287));
#43823=CARTESIAN_POINT('Ctrl Pts',(-0.00257708691874699,-0.041101214337398,
-0.0134163060846059));
#43824=CARTESIAN_POINT('Ctrl Pts',(-0.000637555681479932,-0.041101214337398,
-0.0149684942391342));
#43825=CARTESIAN_POINT('Ctrl Pts',(0.00178486667912529,-0.041101214337398,
-0.0144110293156704));
#43826=CARTESIAN_POINT('Ctrl Pts',(0.0025,-0.041101214337398,-0.0129239268002514));
#43827=CARTESIAN_POINT('Ctrl Pts',(0.0025,-0.041101214337398,-0.0121758532865581));
#43828=CARTESIAN_POINT('Ctrl Pts',(0.0025,-0.0410787743898723,-0.0121758532865581));
#43829=CARTESIAN_POINT('Ctrl Pts',(0.0025,-0.0410787743898723,-0.0114278550357034));
#43830=CARTESIAN_POINT('Ctrl Pts',(0.00178571943910354,-0.0410787743898723,
-0.00993885703610024));
#43831=CARTESIAN_POINT('Ctrl Pts',(-0.000636728572014028,-0.0410787743898723,
-0.00938639369106591));
#43832=CARTESIAN_POINT('Ctrl Pts',(-0.0025795691101196,-0.0410787743898723,
-0.0109341629839093));
#43833=CARTESIAN_POINT('Ctrl Pts',(-0.00257709218909681,-0.0410787743898723,
-0.0134163151357684));
#43834=CARTESIAN_POINT('Ctrl Pts',(-0.000637540000123396,-0.0410787743898723,
-0.0149684405315022));
#43835=CARTESIAN_POINT('Ctrl Pts',(0.00178484651300112,-0.0410787743898723,
-0.0144110741552401));
#43836=CARTESIAN_POINT('Ctrl Pts',(0.0025,-0.0410787743898723,-0.0129238515374128));
#43837=CARTESIAN_POINT('Ctrl Pts',(0.0025,-0.0410787743898723,-0.0121758532865581));
#43838=CARTESIAN_POINT('Ctrl Pts',(0.0025,-0.0410787743898723,-0.0121758532865581));
#43839=CARTESIAN_POINT('Ctrl Pts',(0.0025,-0.041101214337398,-0.0121758532865581));
#43840=CARTESIAN_POINT('Ctrl Pts',(0.00250057355266071,-0.0411453162532137,
-0.0121758532865581));
#43841=CARTESIAN_POINT('Ctrl Pts',(0.00253433766292927,-0.0412183037740197,
-0.0121758532865581));
#43842=CARTESIAN_POINT('Ctrl Pts',(0.00261084648764158,-0.0412766271855573,
-0.0121758532865581));
#43843=CARTESIAN_POINT('Ctrl Pts',(0.00267008006997241,-0.0412787743898725,
-0.0121758532865581));
#43844=CARTESIAN_POINT('Ctrl Pts',(0.00270000000001,-0.0412787743898723,
-0.0121758532865581));
#43845=CARTESIAN_POINT('Origin',(2.27488928325654E-18,-0.0427787743898723,
-0.0086758532865581));
#43846=CARTESIAN_POINT('',(2.23368293997689E-18,-0.0427787743898723,-0.0087758532865581));
#43847=CARTESIAN_POINT('',(0.000750000000000002,-0.0427787743898723,-0.0086758532865581));
#43848=CARTESIAN_POINT('Origin',(0.00303108891324554,-0.0427787743898723,
-0.0104258532865581));
#43849=CARTESIAN_POINT('',(0.00294448637286709,-0.0427787743898723,-0.0104758532865581));
#43850=CARTESIAN_POINT('',(0.00340608891324554,-0.0427787743898723,-0.0110753723393964));
#43851=CARTESIAN_POINT('Origin',(0.00303108891324554,-0.0427787743898723,
-0.0139258532865581));
#43852=CARTESIAN_POINT('',(0.00294448637286709,-0.0427787743898723,-0.0138758532865581));
#43853=CARTESIAN_POINT('',(0.00265608891324554,-0.0427787743898723,-0.0145753723393964));
#43854=CARTESIAN_POINT('Origin',(0.,-0.0444787743898723,-0.0121758532865581));
#43855=CARTESIAN_POINT('',(0.000199999999998,-0.0456787743898783,-0.0121758532865581));
#43856=CARTESIAN_POINT('Origin',(0.,-0.0456787743898823,-0.0121758532865581));
#43857=CARTESIAN_POINT('',(0.000999999999998,-0.0432787743898783,-0.0121758532865581));
#43858=CARTESIAN_POINT('',(0.0006,-0.0444787743898723,-0.0121758532865581));
#43859=CARTESIAN_POINT('',(-0.001,-0.0432787743898823,-0.0121758532865581));
#43860=CARTESIAN_POINT('Origin',(0.,-0.0432787743898823,-0.0121758532865581));
#43861=CARTESIAN_POINT('Origin',(0.,-0.0432787743898823,-0.0121758532865581));
#43862=CARTESIAN_POINT('Origin',(0.,-0.0462787743898723,-0.0121758532865581));
#43863=CARTESIAN_POINT('',(0.0002,-0.0462787743898823,-0.0121758532865581));
#43864=CARTESIAN_POINT('Origin',(0.,-0.0462787743898823,-0.0121758532865581));
#43865=CARTESIAN_POINT('',(0.0002,-0.0462787743898723,-0.0121758532865581));
#43866=CARTESIAN_POINT('Origin',(0.,-0.0340287743898723,-0.0121758532865581));
#43867=CARTESIAN_POINT('',(-0.000999999999999024,-0.0342787743898735,-0.0121758532865581));
#43868=CARTESIAN_POINT('Origin',(0.,-0.0342787743898823,-0.0121758532865581));
#43869=CARTESIAN_POINT('',(-0.0014000000000039,-0.0337787743898674,-0.0121758532865581));
#43870=CARTESIAN_POINT('',(-0.0012,-0.0340287743898723,-0.0121758532865581));
#43871=CARTESIAN_POINT('Origin',(0.,-0.0337787743898723,-0.0121758532865581));
#43872=CARTESIAN_POINT('Origin',(0.,-0.0337787743898723,-0.0121758532865581));
#43873=CARTESIAN_POINT('',(-0.002300000000005,-0.0337787743898773,-0.0121758532865581));
#43874=CARTESIAN_POINT('Origin',(0.,-0.0337787743898723,-0.0121758532865581));
#43875=CARTESIAN_POINT('Origin',(0.,-0.0337787743898723,-0.0121758532865581));
#43876=CARTESIAN_POINT('',(-0.001,-0.0337787743898723,-0.0121758532865581));
#43877=CARTESIAN_POINT('Origin',(0.,-0.0338787743898723,-0.0121758532865581));
#43878=CARTESIAN_POINT('',(-0.000786711117161713,-0.0339787743898823,-0.0145488441458292));
#43879=CARTESIAN_POINT('',(-0.00250000000001,-0.0339787743898823,-0.0121758532865581));
#43880=CARTESIAN_POINT('Origin',(0.,-0.0339787743898823,-0.0121758532865581));
#43881=CARTESIAN_POINT('',(-0.0024,-0.0338787743898723,-0.0121758532865581));
#43882=CARTESIAN_POINT('Origin',(0.,-0.0339787743898823,-0.0121758532865581));
#43883=CARTESIAN_POINT('Ctrl Pts',(-0.000771496087389042,-0.0339794895371937,
-0.014554586149909));
#43884=CARTESIAN_POINT('Ctrl Pts',(-0.000773967688123329,-0.0339793735894346,
-0.0145536626403178));
#43885=CARTESIAN_POINT('Ctrl Pts',(-0.000776437811893427,-0.0339792576009297,
-0.0145527351854424));
#43886=CARTESIAN_POINT('Ctrl Pts',(-0.000781509664634019,-0.0339790192212365,
-0.0145508216205089));
#43887=CARTESIAN_POINT('Ctrl Pts',(-0.000784111224758069,-0.0339788968258219,
-0.014549835070045));
#43888=CARTESIAN_POINT('Ctrl Pts',(-0.000786711117158984,-0.0339787743898754,
-0.0145488441458229));
#43889=CARTESIAN_POINT('Origin',(-2.24345254752611E-19,-0.0397787743898723,
-0.0121758532865581));
#43890=CARTESIAN_POINT('Ctrl Pts',(-0.00175719004339857,-0.0397787743898739,
-0.0139541342405783));
#43891=CARTESIAN_POINT('Ctrl Pts',(-0.00169307291765995,-0.0397787746017101,
-0.0140038566338397));
#43892=CARTESIAN_POINT('Ctrl Pts',(-0.00162653221361426,-0.0397787743898809,
-0.0140503442714278));
#43893=CARTESIAN_POINT('Ctrl Pts',(-0.00155787560922398,-0.0397787743898809,
-0.0140935098107271));
#43894=CARTESIAN_POINT('Ctrl Pts',(-0.00143215670016973,-0.0397787743898808,
-0.0141725513619027));
#43895=CARTESIAN_POINT('Ctrl Pts',(-0.00129934194595018,-0.0397787743898807,
-0.0142404794281288));
#43896=CARTESIAN_POINT('Ctrl Pts',(-0.00116123097203325,-0.0397787743898805,
-0.0142964185823052));
#43897=CARTESIAN_POINT('Ctrl Pts',(-0.00113108173522323,-0.0397787743898805,
-0.0143086299421876));
#43898=CARTESIAN_POINT('Ctrl Pts',(-0.00110068007533138,-0.0397787743898804,
-0.0143202682758157));
#43899=CARTESIAN_POINT('Ctrl Pts',(-0.00107004492089912,-0.0397787743898804,
-0.0143313215520188));
#43900=CARTESIAN_POINT('Ctrl Pts',(-0.00105495584662179,-0.0397787743898804,
-0.014336765745421));
#43901=CARTESIAN_POINT('Ctrl Pts',(-0.00103980846841194,-0.0397787743898804,
-0.0143420684573587));
#43902=CARTESIAN_POINT('Ctrl Pts',(-0.00102462359856661,-0.0397787743898804,
-0.014347222153839));
#43903=CARTESIAN_POINT('Ctrl Pts',(-0.000814784928526715,-0.0397787743898801,
-0.0144184407303709));
#43904=CARTESIAN_POINT('Ctrl Pts',(-0.000596993519393736,-0.0397787743898798,
-0.0144616995548158));
#43905=CARTESIAN_POINT('Ctrl Pts',(-0.000377446859808482,-0.0397787743898794,
-0.0144737272746223));
#43906=CARTESIAN_POINT('Ctrl Pts',(-0.000348131916821991,-0.0397787743898793,
-0.0144753332745544));
#43907=CARTESIAN_POINT('Ctrl Pts',(-0.000318786529917582,-0.0397787743898793,
-0.0144763786947731));
#43908=CARTESIAN_POINT('Ctrl Pts',(-0.000289426596251435,-0.0397787743898792,
-0.0144768522077377));
#43909=CARTESIAN_POINT('Ctrl Pts',(-0.000275910077730923,-0.0397787743898792,
-0.0144770702002859));
#43910=CARTESIAN_POINT('Ctrl Pts',(-0.000262390406744024,-0.0397787743898792,
-0.0144771668815114));
#43911=CARTESIAN_POINT('Ctrl Pts',(-0.000248883867653849,-0.0397787743898792,
-0.0144771413739509));
#43912=CARTESIAN_POINT('Ctrl Pts',(-0.000169711581607006,-0.039778774389879,
-0.0144769918543837));
#43913=CARTESIAN_POINT('Ctrl Pts',(-9.08628147936332E-5,-0.0397787743898786,
-0.0144726507129251));
#43914=CARTESIAN_POINT('Ctrl Pts',(-1.26284316727756E-5,-0.0397787743898793,
-0.0144639743441833));
#43915=CARTESIAN_POINT('Ctrl Pts',(2.79176950103316E-5,-0.0397787743898796,
-0.014459477687699));
#43916=CARTESIAN_POINT('Ctrl Pts',(6.82986355817335E-5,-0.0397787743898797,
-0.0144538157856816));
#43917=CARTESIAN_POINT('Ctrl Pts',(0.000108472229486668,-0.0397787743898798,
-0.0144469633457009));
#43918=CARTESIAN_POINT('Ctrl Pts',(0.000264185840183674,-0.0397787743898801,
-0.014420403158579));
#43919=CARTESIAN_POINT('Ctrl Pts',(0.000416825422655187,-0.0397787743898803,
-0.0143759995156889));
#43920=CARTESIAN_POINT('Ctrl Pts',(0.000563929584611809,-0.0397787743898805,
-0.0143151782020699));
#43921=CARTESIAN_POINT('Ctrl Pts',(0.00057535801717517,-0.0397787743898805,
-0.0143104530313347));
#43922=CARTESIAN_POINT('Ctrl Pts',(0.000586751212388327,-0.0397787743898805,
-0.0143056290827273));
#43923=CARTESIAN_POINT('Ctrl Pts',(0.000598097161382955,-0.0397787743898805,
-0.0143007118517534));
#43924=CARTESIAN_POINT('Ctrl Pts',(0.00084134323732603,-0.0397787743898808,
-0.0141952912175276));
#43925=CARTESIAN_POINT('Ctrl Pts',(0.00106470216535388,-0.0397787743898811,
-0.0140467805829466));
#43926=CARTESIAN_POINT('Ctrl Pts',(0.00125595755705645,-0.039778774389881,
-0.0138622743458417));
#43927=CARTESIAN_POINT('Ctrl Pts',(0.00126478613523544,-0.039778774389881,
-0.0138537573167305));
#43928=CARTESIAN_POINT('Ctrl Pts',(0.00127354488019596,-0.039778774389881,
-0.0138451632153568));
#43929=CARTESIAN_POINT('Ctrl Pts',(0.00128222281185596,-0.039778774389881,
-0.0138365023680465));
#43930=CARTESIAN_POINT('Ctrl Pts',(0.00143780054712722,-0.0397787743898809,
-0.0136812309205574));
#43931=CARTESIAN_POINT('Ctrl Pts',(0.00156853257307188,-0.0397787743898809,
-0.013503836767471));
#43932=CARTESIAN_POINT('Ctrl Pts',(0.00166648651957269,-0.0397787743898807,
-0.013308227265951));
#43933=CARTESIAN_POINT('Ctrl Pts',(0.00168292296901946,-0.0397787743898806,
-0.0132754044364695));
#43934=CARTESIAN_POINT('Ctrl Pts',(0.00169842718748885,-0.0397787743898806,
-0.0132420666686444));
#43935=CARTESIAN_POINT('Ctrl Pts',(0.00171294960382052,-0.0397787743898806,
-0.0132082309571952));
#43936=CARTESIAN_POINT('Ctrl Pts',(0.000483041833372184,-0.0397787743898692,
-0.0102334017947949));
#43937=CARTESIAN_POINT('Ctrl Pts',(0.000414177013520476,-0.0397787743898693,
-0.0102065664006364));
#43938=CARTESIAN_POINT('Ctrl Pts',(0.000343834095042283,-0.0397787743898694,
-0.0101837221474513));
#43939=CARTESIAN_POINT('Ctrl Pts',(0.000272408372401186,-0.0397787743898695,
-0.0101647601900402));
#43940=CARTESIAN_POINT('Ctrl Pts',(0.000200790353882954,-0.0397787743898696,
-0.0101457471823058));
#43941=CARTESIAN_POINT('Ctrl Pts',(0.000128082810507698,-0.0397787743898699,
-0.0101306371703763));
#43942=CARTESIAN_POINT('Ctrl Pts',(5.4645348325696E-5,-0.0397787743898706,
-0.0101193622655315));
#43943=CARTESIAN_POINT('Ctrl Pts',(-2.60214829574234E-7,-0.0397787743898712,
-0.0101109325760838));
#43944=CARTESIAN_POINT('Ctrl Pts',(-5.55746772423925E-5,-0.0397787743898709,
-0.0101046474835075));
#43945=CARTESIAN_POINT('Ctrl Pts',(-0.00011115731807598,-0.0397787743898708,
-0.0101004949795128));
#43946=CARTESIAN_POINT('Ctrl Pts',(-0.000133445379702656,-0.0397787743898708,
-0.0100988298685438));
#43947=CARTESIAN_POINT('Ctrl Pts',(-0.000155776632439193,-0.0397787743898707,
-0.0100975078244661));
#43948=CARTESIAN_POINT('Ctrl Pts',(-0.000178142233916201,-0.0397787743898706,
-0.0100965287355665));
#43949=CARTESIAN_POINT('Ctrl Pts',(-0.00019234388482969,-0.0397787743898706,
-0.0100959070362672));
#43950=CARTESIAN_POINT('Ctrl Pts',(-0.000206551772363642,-0.0397787743898706,
-0.0100954240005371));
#43951=CARTESIAN_POINT('Ctrl Pts',(-0.000220756779646141,-0.0397787743898706,
-0.0100950792693289));
#43952=CARTESIAN_POINT('Ctrl Pts',(-0.000425767795136176,-0.0397787743898701,
-0.0100901040029552));
#43953=CARTESIAN_POINT('Ctrl Pts',(-0.000630534063748425,-0.0397787743898698,
-0.0101137246364624));
#43954=CARTESIAN_POINT('Ctrl Pts',(-0.000828216436399461,-0.0397787743898695,
-0.0101651844785696));
#43955=CARTESIAN_POINT('Ctrl Pts',(-0.000847794356858231,-0.0397787743898695,
-0.0101702809203114));
#43956=CARTESIAN_POINT('Ctrl Pts',(-0.00086730325133829,-0.0397787743898694,
-0.010175652348327));
#43957=CARTESIAN_POINT('Ctrl Pts',(-0.00088673662891264,-0.0397787743898694,
-0.0101812993238104));
#43958=CARTESIAN_POINT('Ctrl Pts',(-0.000899127635869771,-0.0397787743898694,
-0.0101848999183151));
#43959=CARTESIAN_POINT('Ctrl Pts',(-0.000911479167813636,-0.0397787743898694,
-0.0101886100052308));
#43960=CARTESIAN_POINT('Ctrl Pts',(-0.000923787881901184,-0.0397787743898694,
-0.0101924287155602));
#43961=CARTESIAN_POINT('Ctrl Pts',(-0.0010006813909627,-0.0397787743898693,
-0.0102162845005941));
#43962=CARTESIAN_POINT('Ctrl Pts',(-0.00107592433438783,-0.0397787743898692,
-0.0102443815824418));
#43963=CARTESIAN_POINT('Ctrl Pts',(-0.001149122989709,-0.0397787743898691,
-0.0102766566890817));
#43964=CARTESIAN_POINT('Ctrl Pts',(-0.00118063222353515,-0.039778774389869,
-0.0102905498935049));
#43965=CARTESIAN_POINT('Ctrl Pts',(-0.00121176282517371,-0.039778774389869,
-0.0103052179143883));
#43966=CARTESIAN_POINT('Ctrl Pts',(-0.00124248380239654,-0.039778774389869,
-0.0103206586458563));
#43967=CARTESIAN_POINT('Ctrl Pts',(-0.00135026660817169,-0.0397787743898688,
-0.0103748315762539));
#43968=CARTESIAN_POINT('Ctrl Pts',(-0.00145301438322215,-0.0397787743898688,
-0.0104384928979925));
#43969=CARTESIAN_POINT('Ctrl Pts',(-0.00155024698053707,-0.0397787743898687,
-0.0105105042446334));
#43970=CARTESIAN_POINT('Ctrl Pts',(-0.00157849804471611,-0.0397787743898687,
-0.0105314272399226));
#43971=CARTESIAN_POINT('Ctrl Pts',(-0.00160628289122325,-0.0397787743898687,
-0.010553056998596));
#43972=CARTESIAN_POINT('Ctrl Pts',(-0.00163358791178077,-0.0397787743898687,
-0.0105753698802968));
#43973=CARTESIAN_POINT('Ctrl Pts',(-0.00164341407028885,-0.0397787743898687,
-0.0105833995359384));
#43974=CARTESIAN_POINT('Ctrl Pts',(-0.00165317745973684,-0.0397787743898687,
-0.0105915172646323));
#43975=CARTESIAN_POINT('Ctrl Pts',(-0.00166286744266842,-0.0397787743898687,
-0.010599713243512));
#43976=CARTESIAN_POINT('Ctrl Pts',(-0.00187591233938246,-0.0397787743898686,
-0.0107799108234484));
#43977=CARTESIAN_POINT('Ctrl Pts',(-0.00205500826442918,-0.0397787743898687,
-0.0109984408165224));
#43978=CARTESIAN_POINT('Ctrl Pts',(-0.00219419613869514,-0.0397787743898689,
-0.011242458169426));
#43979=CARTESIAN_POINT('Ctrl Pts',(-0.00220088488234335,-0.0397787743898689,
-0.0112541845466546));
#43980=CARTESIAN_POINT('Ctrl Pts',(-0.00220748074423558,-0.0397787743898689,
-0.0112659708583141));
#43981=CARTESIAN_POINT('Ctrl Pts',(-0.00221398281530691,-0.0397787743898689,
-0.011277815973893));
#43982=CARTESIAN_POINT('Ctrl Pts',(-0.00222015900819364,-0.0397787743898689,
-0.0112890674225127));
#43983=CARTESIAN_POINT('Ctrl Pts',(-0.0022262457661904,-0.0397787743898689,
-0.0113003631705176));
#43984=CARTESIAN_POINT('Ctrl Pts',(-0.00223224252299715,-0.0397787743898689,
-0.0113117017067491));
#43985=CARTESIAN_POINT('Ctrl Pts',(-0.0023529561855896,-0.0397787743898691,
-0.0115399444521286));
#43986=CARTESIAN_POINT('Ctrl Pts',(-0.00243745467686456,-0.0397787743898694,
-0.0117853097684529));
#43987=CARTESIAN_POINT('Ctrl Pts',(-0.00248078229039228,-0.0397787743898698,
-0.012039045318197));
#43988=CARTESIAN_POINT('Ctrl Pts',(-0.00248852509767497,-0.0397787743898699,
-0.0120843888140066));
#43989=CARTESIAN_POINT('Ctrl Pts',(-0.00249494460435551,-0.0397787743898701,
-0.0121300059194942));
#43990=CARTESIAN_POINT('Ctrl Pts',(-0.00250000000000001,-0.0397787743898723,
-0.0121758532865581));
#43991=CARTESIAN_POINT('Ctrl Pts',(0.000906555879570053,-0.0336884873565647,
-0.0139554885237476));
#43992=CARTESIAN_POINT('Ctrl Pts',(0.00148851471592875,-0.0337405323694969,
-0.0136590408284119));
#43993=CARTESIAN_POINT('Ctrl Pts',(0.00233007966486597,-0.0338446173408443,
-0.0124566928781431));
#43994=CARTESIAN_POINT('Ctrl Pts',(0.00152799326844162,-0.0340007422706073,
-0.0103918577137271));
#43995=CARTESIAN_POINT('Ctrl Pts',(-0.00063191986896287,-0.0341568621458532,
-0.00991565403964754));
#43996=CARTESIAN_POINT('Ctrl Pts',(-0.00223010102783316,-0.0343129820210993,
-0.0114427530396798));
#43997=CARTESIAN_POINT('Ctrl Pts',(-0.00184953643573394,-0.0344691018963453,
-0.0136218346413422));
#43998=CARTESIAN_POINT('Ctrl Pts',(0.000172737121026436,-0.0346252217715913,
-0.0145169013604168));
#43999=CARTESIAN_POINT('Ctrl Pts',(0.00204157869281899,-0.0347813416468374,
-0.013334655467512));
#44000=CARTESIAN_POINT('Ctrl Pts',(0.00209858523606372,-0.0349374615220834,
-0.0111237801770316));
#44001=CARTESIAN_POINT('Ctrl Pts',(0.000293061994614866,-0.0350935813973294,
-0.00984672032610751));
#44002=CARTESIAN_POINT('Ctrl Pts',(-0.00177253570391892,-0.0352497012725754,
-0.0106367143420735));
#44003=CARTESIAN_POINT('Ctrl Pts',(-0.0022650169213336,-0.0354058211478214,
-0.0127927219130861));
#44004=CARTESIAN_POINT('Ctrl Pts',(-0.000747290023119862,-0.0355619410230674,
-0.0144012441562325));
#44005=CARTESIAN_POINT('Ctrl Pts',(0.00143365440835409,-0.0357180608983135,
-0.0140347387897662));
#44006=CARTESIAN_POINT('Ctrl Pts',(0.00234223148318713,-0.0358741807735595,
-0.0120184681222078));
#44007=CARTESIAN_POINT('Ctrl Pts',(0.00117207673424978,-0.0360303006488055,
-0.010141878857636));
#44008=CARTESIAN_POINT('Ctrl Pts',(-0.00103829608658593,-0.0361864205240515,
-0.0100704414314441));
#44009=CARTESIAN_POINT('Ctrl Pts',(-0.0023271810267558,-0.0363425403992976,
-0.0118675581893953));
#44010=CARTESIAN_POINT('Ctrl Pts',(-0.00155069202014295,-0.0364986602745435,
-0.0139382866448643));
#44011=CARTESIAN_POINT('Ctrl Pts',(0.000602036529911888,-0.0366547801497896,
-0.0144448551399557));
#44012=CARTESIAN_POINT('Ctrl Pts',(0.00222045755410605,-0.0368109000250356,
-0.0129376837430793));
#44013=CARTESIAN_POINT('Ctrl Pts',(0.00186822176134942,-0.0369670199002817,
-0.0107543876576293));
#44014=CARTESIAN_POINT('Ctrl Pts',(-0.000142061225288998,-0.0371231397755276,
-0.00983264266723763));
#44015=CARTESIAN_POINT('Ctrl Pts',(-0.00202626513103703,-0.0372792596507737,
-0.0109904978707365));
#44016=CARTESIAN_POINT('Ctrl Pts',(-0.00211215758058384,-0.0374353795260197,
-0.0132003561920008));
#44017=CARTESIAN_POINT('Ctrl Pts',(-0.000323510645583594,-0.0375914994012657,
-0.0145009681811352));
#44018=CARTESIAN_POINT('Ctrl Pts',(0.00175225415004698,-0.0377476192765118,
-0.0137380394695316));
#44019=CARTESIAN_POINT('Ctrl Pts',(0.00227288891551885,-0.0379037391517577,
-0.0115886711349254));
#44020=CARTESIAN_POINT('Ctrl Pts',(0.000776341706463385,-0.0380598590270038,
-0.00996042508615809));
#44021=CARTESIAN_POINT('Ctrl Pts',(-0.00140922355039861,-0.0382159789022498,
-0.0102983761236881));
#44022=CARTESIAN_POINT('Ctrl Pts',(-0.00234407459792171,-0.0383720987774958,
-0.0123025811821577));
#44023=CARTESIAN_POINT('Ctrl Pts',(-0.00119861222885379,-0.0385282186527418,
-0.0141943295796207));
#44024=CARTESIAN_POINT('Ctrl Pts',(0.00101072130964566,-0.0386843385279879,
-0.0142946521179208));
#44025=CARTESIAN_POINT('Ctrl Pts',(0.00232284301417837,-0.0388404584032339,
-0.0125145929042303));
#44026=CARTESIAN_POINT('Ctrl Pts',(0.00157381725247728,-0.0389965782784799,
-0.0104338009448371));
#44027=CARTESIAN_POINT('Ctrl Pts',(-0.000572693408805765,-0.0391526981537259,
-0.00989927497122912));
#44028=CARTESIAN_POINT('Ctrl Pts',(-0.00220955263118552,-0.039308818028972,
-0.0113848409437049));
#44029=CARTESIAN_POINT('Ctrl Pts',(-0.00188811561699103,-0.0394649379042179,
-0.0135731446123589));
#44030=CARTESIAN_POINT('Ctrl Pts',(0.000114518372946742,-0.0396210666742362,
-0.0145200265170436));
#44031=CARTESIAN_POINT('Ctrl Pts',(0.00137369945946738,-0.039725155485839,
-0.0137659946183006));
#44032=CARTESIAN_POINT('Ctrl Pts',(0.00171075374050644,-0.0397772043390267,
-0.0132065165554317));
#44033=CARTESIAN_POINT('Ctrl Pts',(0.00098385440276809,-0.0337868080702585,
-0.0141072311562383));
#44034=CARTESIAN_POINT('Ctrl Pts',(0.00161543462444493,-0.0338388530831906,
-0.0137855065093421));
#44035=CARTESIAN_POINT('Ctrl Pts',(0.00252875657059996,-0.0339429380545382,
-0.0124806389868986));
#44036=CARTESIAN_POINT('Ctrl Pts',(0.00165827936085888,-0.034099062984301,
-0.0102397432922342));
#44037=CARTESIAN_POINT('Ctrl Pts',(-0.000685801238827782,-0.0342551828595471,
-0.0097229355676187));
#44038=CARTESIAN_POINT('Ctrl Pts',(-0.00242025314081233,-0.0344113027347931,
-0.0113802444092502));
#44039=CARTESIAN_POINT('Ctrl Pts',(-0.00200723927381052,-0.0345674226100391,
-0.0137451278942078));
#44040=CARTESIAN_POINT('Ctrl Pts',(0.000187465749076539,-0.0347235424852852,
-0.0147165135000796));
#44041=CARTESIAN_POINT('Ctrl Pts',(0.00221565623343605,-0.0348796623605312,
-0.0134334620598964));
#44042=CARTESIAN_POINT('Ctrl Pts',(0.00227752350474481,-0.0350357822357772,
-0.0110340739609059));
#44043=CARTESIAN_POINT('Ctrl Pts',(0.000318050260533953,-0.0351919021110232,
-0.00964812414220752));
#44044=CARTESIAN_POINT('Ctrl Pts',(-0.00192367298659113,-0.0353480219862693,
-0.0105054779008497));
#44045=CARTESIAN_POINT('Ctrl Pts',(-0.00245814617787837,-0.0355041418615152,
-0.0128453199215624));
#44046=CARTESIAN_POINT('Ctrl Pts',(-0.000811008561038556,-0.0356602617367613,
-0.0145909946521928));
#44047=CARTESIAN_POINT('Ctrl Pts',(0.00155589659004363,-0.0358163816120073,
-0.0141932387867663));
#44048=CARTESIAN_POINT('Ctrl Pts',(0.00254194452759889,-0.0359725014872533,
-0.0120050484962897));
#44049=CARTESIAN_POINT('Ctrl Pts',(0.00127201519659285,-0.0361286213624993,
-0.00996844970327133));
#44050=CARTESIAN_POINT('Ctrl Pts',(-0.00112682758910452,-0.0362847412377453,
-0.00989092108328737));
#44051=CARTESIAN_POINT('Ctrl Pts',(-0.00252561077679837,-0.0364408611129914,
-0.011841271055577));
#44052=CARTESIAN_POINT('Ctrl Pts',(-0.00168291354756704,-0.0365969809882374,
-0.0140885625394916));
#44053=CARTESIAN_POINT('Ctrl Pts',(0.000653369862718166,-0.0367531008634834,
-0.0146383241762873));
#44054=CARTESIAN_POINT('Ctrl Pts',(0.00240978740527609,-0.0369092207387295,
-0.0130026420876706));
#44055=CARTESIAN_POINT('Ctrl Pts',(0.00202751782507054,-0.0370653406139755,
-0.0106331847661483));
#44056=CARTESIAN_POINT('Ctrl Pts',(-0.000154174238028764,-0.0372214604892215,
-0.00963284613566438));
#44057=CARTESIAN_POINT('Ctrl Pts',(-0.00219903694330649,-0.0373775803644675,
-0.0108894271864326));
#44058=CARTESIAN_POINT('Ctrl Pts',(-0.00229225311073265,-0.0375337002397135,
-0.0132877116031647));
#44059=CARTESIAN_POINT('Ctrl Pts',(-0.000351095150528087,-0.0376898201149596,
-0.0146992217600561));
#44060=CARTESIAN_POINT('Ctrl Pts',(0.00190166210284798,-0.0378459399902055,
-0.0138712410598864));
#44061=CARTESIAN_POINT('Ctrl Pts',(0.00246668938664495,-0.0380020598654516,
-0.0115386043776605));
#44062=CARTESIAN_POINT('Ctrl Pts',(0.000842537369366294,-0.0381581797406976,
-0.00977152406857997));
#44063=CARTESIAN_POINT('Ctrl Pts',(-0.00152938260706192,-0.0383142996159437,
-0.0101382908875782));
#44064=CARTESIAN_POINT('Ctrl Pts',(-0.00254394479761788,-0.0384704194911896,
-0.0123133867810167));
#44065=CARTESIAN_POINT('Ctrl Pts',(-0.00130081327047237,-0.0386265393664357,
-0.0143664372677182));
#44066=CARTESIAN_POINT('Ctrl Pts',(0.00109690161729249,-0.0387826592416817,
-0.0144753139219078));
#44067=CARTESIAN_POINT('Ctrl Pts',(0.00252090287862051,-0.0389387791169277,
-0.0125434759248856));
#44068=CARTESIAN_POINT('Ctrl Pts',(0.00170801057926678,-0.0390948989921738,
-0.010285262860883));
#44069=CARTESIAN_POINT('Ctrl Pts',(-0.000621524766853903,-0.0392510188674198,
-0.00970515991921151));
#44070=CARTESIAN_POINT('Ctrl Pts',(-0.00239795266163922,-0.0394071387426657,
-0.0113173943722227));
#44071=CARTESIAN_POINT('Ctrl Pts',(-0.00204910795305066,-0.0395632586179118,
-0.0136922862542543));
#44072=CARTESIAN_POINT('Ctrl Pts',(0.000124282912902093,-0.03971938738793,
-0.014719905126758));
#44073=CARTESIAN_POINT('Ctrl Pts',(0.00149082951391602,-0.0398234761995329,
-0.0139015798363658));
#44074=CARTESIAN_POINT('Ctrl Pts',(0.00185662311345606,-0.0398755250527205,
-0.0132943972370243));
#44075=CARTESIAN_POINT('Ctrl Pts',(0.00106115292596612,-0.0338851287839525,
-0.0142589737887292));
#44076=CARTESIAN_POINT('Ctrl Pts',(0.00174235453296112,-0.0339371737968846,
-0.0139119721902721));
#44077=CARTESIAN_POINT('Ctrl Pts',(0.00272743347633392,-0.0340412587682322,
-0.012504585095654));
#44078=CARTESIAN_POINT('Ctrl Pts',(0.00178856545327616,-0.034197383697995,
-0.0100876288707415));
#44079=CARTESIAN_POINT('Ctrl Pts',(-0.000739682608692693,-0.034353503573241,
-0.00953021709558985));
#44080=CARTESIAN_POINT('Ctrl Pts',(-0.00261040525379151,-0.034509623448487,
-0.0113177357788206));
#44081=CARTESIAN_POINT('Ctrl Pts',(-0.00216494211188709,-0.0346657433237329,
-0.0138684211470736));
#44082=CARTESIAN_POINT('Ctrl Pts',(0.00020219437712664,-0.0348218631989791,
-0.0149161256397424));
#44083=CARTESIAN_POINT('Ctrl Pts',(0.00238973377405311,-0.0349779830742251,
-0.0135322686522809));
#44084=CARTESIAN_POINT('Ctrl Pts',(0.00245646177342591,-0.0351341029494712,
-0.0109443677447801));
#44085=CARTESIAN_POINT('Ctrl Pts',(0.000343038526453036,-0.035290222824717,
-0.00944952795830755));
#44086=CARTESIAN_POINT('Ctrl Pts',(-0.00207481026926333,-0.0354463426999631,
-0.010374241459626));
#44087=CARTESIAN_POINT('Ctrl Pts',(-0.00265127543442315,-0.0356024625752092,
-0.0128979179300387));
#44088=CARTESIAN_POINT('Ctrl Pts',(-0.000874727098957249,-0.0357585824504551,
-0.0147807451481533));
#44089=CARTESIAN_POINT('Ctrl Pts',(0.00167813877173317,-0.0359147023257013,
-0.0143517387837662));
#44090=CARTESIAN_POINT('Ctrl Pts',(0.00274165757201066,-0.0360708222009473,
-0.0119916288703718));
#44091=CARTESIAN_POINT('Ctrl Pts',(0.00137195365893592,-0.0362269420761933,
-0.00979502054890656));
#44092=CARTESIAN_POINT('Ctrl Pts',(-0.0012153590916231,-0.0363830619514392,
-0.00971140073513063));
#44093=CARTESIAN_POINT('Ctrl Pts',(-0.00272404052684096,-0.0365391818266853,
-0.0118149839217589));
#44094=CARTESIAN_POINT('Ctrl Pts',(-0.00181513507499112,-0.0366953017019313,
-0.0142388384341189));
#44095=CARTESIAN_POINT('Ctrl Pts',(0.000704703195524443,-0.0368514215771773,
-0.0148317932126191));
#44096=CARTESIAN_POINT('Ctrl Pts',(0.00259911725644613,-0.0370075414524233,
-0.0130676004322619));
#44097=CARTESIAN_POINT('Ctrl Pts',(0.00218681388879167,-0.0371636613276694,
-0.0105119818746673));
#44098=CARTESIAN_POINT('Ctrl Pts',(-0.000166287250768526,-0.0373197812029154,
-0.00943304960409114));
#44099=CARTESIAN_POINT('Ctrl Pts',(-0.00237180875557593,-0.0374759010781614,
-0.0107883565021288));
#44100=CARTESIAN_POINT('Ctrl Pts',(-0.00247234864088144,-0.0376320209534073,
-0.0133750670143283));
#44101=CARTESIAN_POINT('Ctrl Pts',(-0.000378679655472579,-0.0377881408286535,
-0.0148974753389772));
#44102=CARTESIAN_POINT('Ctrl Pts',(0.00205107005564896,-0.0379442607038995,
-0.0140044426502412));
#44103=CARTESIAN_POINT('Ctrl Pts',(0.00266048985777104,-0.0381003805791455,
-0.0114885376203958));
#44104=CARTESIAN_POINT('Ctrl Pts',(0.000908733032269202,-0.0382565004543916,
-0.00958262305100186));
#44105=CARTESIAN_POINT('Ctrl Pts',(-0.00164954166372522,-0.0384126203296376,
-0.00997820565146808));
#44106=CARTESIAN_POINT('Ctrl Pts',(-0.00274381499731402,-0.0385687402048836,
-0.0123241923798756));
#44107=CARTESIAN_POINT('Ctrl Pts',(-0.00140301431209096,-0.0387248600801295,
-0.0145385449558156));
#44108=CARTESIAN_POINT('Ctrl Pts',(0.00118308192493933,-0.0388809799553756,
-0.0146559757258947));
#44109=CARTESIAN_POINT('Ctrl Pts',(0.00271896274306265,-0.0390370998306216,
-0.0125723589455407));
#44110=CARTESIAN_POINT('Ctrl Pts',(0.00184220390605629,-0.0391932197058677,
-0.0101367247769288));
#44111=CARTESIAN_POINT('Ctrl Pts',(-0.000670356124902047,-0.0393493395811137,
-0.00951104486719392));
#44112=CARTESIAN_POINT('Ctrl Pts',(-0.00258635269209294,-0.0395054594563597,
-0.0112499478007406));
#44113=CARTESIAN_POINT('Ctrl Pts',(-0.00221010028911027,-0.0396615793316057,
-0.0138114278961496));
#44114=CARTESIAN_POINT('Ctrl Pts',(0.000134047452857446,-0.0398177081016239,
-0.0149197837364725));
#44115=CARTESIAN_POINT('Ctrl Pts',(0.00160795956836466,-0.039921796913227,
-0.0140371650544312));
#44116=CARTESIAN_POINT('Ctrl Pts',(0.00200249248640567,-0.0399738457664145,
-0.0133822779186168));
#44117=CARTESIAN_POINT('Ctrl Pts',(0.00113845144916417,-0.0339834494976463,
-0.0144107164212199));
#44118=CARTESIAN_POINT('Ctrl Pts',(0.00186927444147729,-0.0340354945105784,
-0.0140384378712023));
#44119=CARTESIAN_POINT('Ctrl Pts',(0.0029261103820679,-0.0341395794819259,
-0.0125285312044095));
#44120=CARTESIAN_POINT('Ctrl Pts',(0.00191885154569343,-0.0342957044116889,
-0.00993551444924871));
#44121=CARTESIAN_POINT('Ctrl Pts',(-0.000793563978557607,-0.0344518242869349,
-0.009337498623561));
#44122=CARTESIAN_POINT('Ctrl Pts',(-0.00280055736677067,-0.0346079441621809,
-0.011255227148391));
#44123=CARTESIAN_POINT('Ctrl Pts',(-0.00232264494996366,-0.0347640640374269,
-0.0139917143999392));
#44124=CARTESIAN_POINT('Ctrl Pts',(0.000216923005176743,-0.034920183912673,
-0.0151157377794053));
#44125=CARTESIAN_POINT('Ctrl Pts',(0.00256381131467016,-0.0350763037879189,
-0.0136310752446654));
#44126=CARTESIAN_POINT('Ctrl Pts',(0.00263540004210701,-0.035232423663165,
-0.0108546615286545));
#44127=CARTESIAN_POINT('Ctrl Pts',(0.00036802679237212,-0.035388543538411,
-0.00925093177440756));
#44128=CARTESIAN_POINT('Ctrl Pts',(-0.00222594755193554,-0.035544663413657,
-0.0102430050184023));
#44129=CARTESIAN_POINT('Ctrl Pts',(-0.00284440469096792,-0.035700783288903,
-0.0129505159385148));
#44130=CARTESIAN_POINT('Ctrl Pts',(-0.000938445636875939,-0.035856903164149,
-0.0149704956441137));
#44131=CARTESIAN_POINT('Ctrl Pts',(0.00180038095342271,-0.036013023039395,
-0.0145102387807663));
#44132=CARTESIAN_POINT('Ctrl Pts',(0.00294137061642242,-0.0361691429146411,
-0.0119782092444539));
#44133=CARTESIAN_POINT('Ctrl Pts',(0.00147189212127897,-0.0363252627898871,
-0.00962159139454179));
#44134=CARTESIAN_POINT('Ctrl Pts',(-0.00130389059414169,-0.0364813826651332,
-0.00953188038697389));
#44135=CARTESIAN_POINT('Ctrl Pts',(-0.00292247027688355,-0.0366375025403792,
-0.0117886967879408));
#44136=CARTESIAN_POINT('Ctrl Pts',(-0.0019473566024152,-0.0367936224156252,
-0.0143891143287463));
#44137=CARTESIAN_POINT('Ctrl Pts',(0.00075603652833072,-0.0369497422908712,
-0.0150252622489507));
#44138=CARTESIAN_POINT('Ctrl Pts',(0.00278844710761618,-0.0371058621661172,
-0.0131325587768532));
#44139=CARTESIAN_POINT('Ctrl Pts',(0.0023461099525128,-0.0372619820413633,
-0.0103907789831864));
#44140=CARTESIAN_POINT('Ctrl Pts',(-0.00017840026350829,-0.0374181019166092,
-0.00923325307251788));
#44141=CARTESIAN_POINT('Ctrl Pts',(-0.00254458056784538,-0.0375742217918553,
-0.0106872858178249));
#44142=CARTESIAN_POINT('Ctrl Pts',(-0.00265244417103022,-0.0377303416671013,
-0.0134624224254922));
#44143=CARTESIAN_POINT('Ctrl Pts',(-0.000406264160417076,-0.0378864615423473,
-0.0150957289178981));
#44144=CARTESIAN_POINT('Ctrl Pts',(0.00220047800844996,-0.0380425814175933,
-0.014137644240596));
#44145=CARTESIAN_POINT('Ctrl Pts',(0.00285429032889712,-0.0381987012928394,
-0.0114384708631308));
#44146=CARTESIAN_POINT('Ctrl Pts',(0.000974928695172114,-0.0383548211680854,
-0.00939372203342373));
#44147=CARTESIAN_POINT('Ctrl Pts',(-0.00176970072038853,-0.0385109410433314,
-0.00981812041535807));
#44148=CARTESIAN_POINT('Ctrl Pts',(-0.00294368519701017,-0.0386670609185775,
-0.0123349979787346));
#44149=CARTESIAN_POINT('Ctrl Pts',(-0.00150521535370954,-0.0388231807938234,
-0.0147106526439131));
#44150=CARTESIAN_POINT('Ctrl Pts',(0.00126926223258616,-0.0389793006690694,
-0.0148366375298816));
#44151=CARTESIAN_POINT('Ctrl Pts',(0.00291702260750478,-0.0391354205443155,
-0.012601241966196));
#44152=CARTESIAN_POINT('Ctrl Pts',(0.0019763972328458,-0.0392915404195615,
-0.00998818669297467));
#44153=CARTESIAN_POINT('Ctrl Pts',(-0.00071918748295019,-0.0394476602948075,
-0.0093169298151763));
#44154=CARTESIAN_POINT('Ctrl Pts',(-0.00277475272254664,-0.0396037801700536,
-0.0111825012292584));
#44155=CARTESIAN_POINT('Ctrl Pts',(-0.00237109262516989,-0.0397599000452996,
-0.0139305695380448));
#44156=CARTESIAN_POINT('Ctrl Pts',(0.000143811992812799,-0.0399160288153178,
-0.0151196623461868));
#44157=CARTESIAN_POINT('Ctrl Pts',(0.00172508962281328,-0.0400201176269206,
-0.0141727502724965));
#44158=CARTESIAN_POINT('Ctrl Pts',(0.00214836185935528,-0.0400721664801083,
-0.0134701586002094));
#44159=CARTESIAN_POINT('Ctrl Pts',(0.00151144094680255,-0.033978774389881,
-0.0108636057192968));
#44160=CARTESIAN_POINT('Ctrl Pts',(0.00166330063753257,-0.0339787743898811,
-0.0109989552134901));
#44161=CARTESIAN_POINT('Ctrl Pts',(0.00179339272885179,-0.033978774389881,
-0.011157796271544));
#44162=CARTESIAN_POINT('Ctrl Pts',(0.00189962202083712,-0.0339787743898808,
-0.0113327013342186));
#44163=CARTESIAN_POINT('Ctrl Pts',(0.00191122342101952,-0.0339787743898808,
-0.0113518028794524));
#44164=CARTESIAN_POINT('Ctrl Pts',(0.00192253879240254,-0.0339787743898808,
-0.0113710986315245));
#44165=CARTESIAN_POINT('Ctrl Pts',(0.0019335642210336,-0.0339787743898808,
-0.0113905806628577));
#44166=CARTESIAN_POINT('Ctrl Pts',(0.00194056621304015,-0.0339787743898807,
-0.0114029532455691));
#44167=CARTESIAN_POINT('Ctrl Pts',(0.0019474474664082,-0.0339787743898807,
-0.0114153943530156));
#44168=CARTESIAN_POINT('Ctrl Pts',(0.00195420415872564,-0.0339787743898807,
-0.011427895692725));
#44169=CARTESIAN_POINT('Ctrl Pts',(0.00205171004550552,-0.0339787743898806,
-0.0116083026369859));
#44170=CARTESIAN_POINT('Ctrl Pts',(0.00212362567593681,-0.0339787743898803,
-0.0118014738101103));
#44171=CARTESIAN_POINT('Ctrl Pts',(0.00216752041363818,-0.03397877438988,
-0.0120009720848389));
#44172=CARTESIAN_POINT('Ctrl Pts',(0.0021718675886441,-0.03397877438988,
-0.0120207296676162));
#44173=CARTESIAN_POINT('Ctrl Pts',(0.00217593841741397,-0.03397877438988,
-0.0120405505893999));
#44174=CARTESIAN_POINT('Ctrl Pts',(0.00217972945324975,-0.0339787743898799,
-0.0120604293217883));
#44175=CARTESIAN_POINT('Ctrl Pts',(0.00218214673490848,-0.0339787743898799,
-0.0120731046161624));
#44176=CARTESIAN_POINT('Ctrl Pts',(0.00218444853340343,-0.0339787743898799,
-0.0120857944484929));
#44177=CARTESIAN_POINT('Ctrl Pts',(0.00218663410517573,-0.0339787743898797,
-0.012098495444595));
#44178=CARTESIAN_POINT('Ctrl Pts',(0.00220028731583387,-0.0339787743898783,
-0.0121778382406302));
#44179=CARTESIAN_POINT('Ctrl Pts',(0.00220941217430585,-0.0339787743898788,
-0.0122576359088878));
#44180=CARTESIAN_POINT('Ctrl Pts',(0.00221388631338771,-0.0339787743898789,
-0.0123375089230316));
#44181=CARTESIAN_POINT('Ctrl Pts',(0.00221581226193364,-0.033978774389879,
-0.0123718912505887));
#44182=CARTESIAN_POINT('Ctrl Pts',(0.00221687594955819,-0.0339787743898791,
-0.0124062879804758));
#44183=CARTESIAN_POINT('Ctrl Pts',(0.00221706518265614,-0.0339787743898792,
-0.0124406705429053));
#44184=CARTESIAN_POINT('Ctrl Pts',(0.00221792199649984,-0.0339787743898795,
-0.0125963486763256));
#44185=CARTESIAN_POINT('Ctrl Pts',(0.00220091840700706,-0.0339787743898797,
-0.0127517267421406));
#44186=CARTESIAN_POINT('Ctrl Pts',(0.00216767342000132,-0.03397877438988,
-0.0129047836695825));
#44187=CARTESIAN_POINT('Ctrl Pts',(0.00216497993523347,-0.03397877438988,
-0.0129171842309847));
#44188=CARTESIAN_POINT('Ctrl Pts',(0.00216217948073034,-0.03397877438988,
-0.0129295688496655));
#44189=CARTESIAN_POINT('Ctrl Pts',(0.00215927597939003,-0.03397877438988,
-0.0129419235881118));
#44190=CARTESIAN_POINT('Ctrl Pts',(0.00210292817318756,-0.0339787743898804,
-0.0131816901065538));
#44191=CARTESIAN_POINT('Ctrl Pts',(0.00200786407849481,-0.0339787743898806,
-0.0134114392628006));
#44192=CARTESIAN_POINT('Ctrl Pts',(0.00188036716095463,-0.0339787743898808,
-0.0136235328573169));
#44193=CARTESIAN_POINT('Ctrl Pts',(0.00186342196383062,-0.0339787743898808,
-0.0136517215213031));
#44194=CARTESIAN_POINT('Ctrl Pts',(0.00184589784857195,-0.0339787743898808,
-0.0136795980104251));
#44195=CARTESIAN_POINT('Ctrl Pts',(0.00182780425197144,-0.0339787743898809,
-0.0137071434861153));
#44196=CARTESIAN_POINT('Ctrl Pts',(0.00182039269394275,-0.0339787743898809,
-0.013718426753672));
#44197=CARTESIAN_POINT('Ctrl Pts',(0.00181288556877312,-0.0339787743898808,
-0.0137296544738017));
#44198=CARTESIAN_POINT('Ctrl Pts',(0.00180528347101283,-0.0339787743898809,
-0.0137408253232928));
#44199=CARTESIAN_POINT('Ctrl Pts',(0.00179806238775325,-0.0339787743898809,
-0.0137514362936854));
#44200=CARTESIAN_POINT('Ctrl Pts',(0.00179076123317478,-0.0339787743898809,
-0.0137619876892948));
#44201=CARTESIAN_POINT('Ctrl Pts',(0.00178338109605654,-0.0339787743898809,
-0.0137724783202789));
#44202=CARTESIAN_POINT('Ctrl Pts',(0.0016348184319285,-0.033978774389881,
-0.0139836554383211));
#44203=CARTESIAN_POINT('Ctrl Pts',(0.00145455809974202,-0.033978774389881,
-0.0141703380238125));
#44204=CARTESIAN_POINT('Ctrl Pts',(0.00124814854542299,-0.0339787743898809,
-0.0143241368117442));
#44205=CARTESIAN_POINT('Ctrl Pts',(0.0012112623088025,-0.0339787743898809,
-0.0143516212879464));
#44206=CARTESIAN_POINT('Ctrl Pts',(0.00117353151163338,-0.0339787743898809,
-0.0143780508975888));
#44207=CARTESIAN_POINT('Ctrl Pts',(0.00113497624935288,-0.0339787743898726,
-0.014403369597027));
#44208=CARTESIAN_POINT('Origin',(2.24345254752611E-19,-0.0339787743898723,
-0.0121758532865581));
#44209=CARTESIAN_POINT('Ctrl Pts',(-0.000786711117161725,-0.0339787743898715,
-0.0145488441458292));
#44210=CARTESIAN_POINT('Ctrl Pts',(-0.000860123002178482,-0.0339787741780464,
-0.0145142886963759));
#44211=CARTESIAN_POINT('Ctrl Pts',(-0.000931752987587147,-0.033978774389869,
-0.0144761052423907));
#44212=CARTESIAN_POINT('Ctrl Pts',(-0.00100138356020524,-0.0339787743898689,
-0.0144345282803354));
#44213=CARTESIAN_POINT('Ctrl Pts',(-0.00112888556271287,-0.0339787743898688,
-0.0143583958327494));
#44214=CARTESIAN_POINT('Ctrl Pts',(-0.00124970686175793,-0.0339787743898688,
-0.0142708955021727));
#44215=CARTESIAN_POINT('Ctrl Pts',(-0.00136225039894955,-0.0339787743898687,
-0.0141732333563242));
#44216=CARTESIAN_POINT('Ctrl Pts',(-0.00139891908765987,-0.0339787743898687,
-0.0141414132899369));
#44217=CARTESIAN_POINT('Ctrl Pts',(-0.00143473026633101,-0.0339787743898687,
-0.0141084886236575));
#44218=CARTESIAN_POINT('Ctrl Pts',(-0.00146953555976837,-0.0339787743898687,
-0.0140745793427416));
#44219=CARTESIAN_POINT('Ctrl Pts',(-0.00162825693636651,-0.0339787743898687,
-0.0139199440210739));
#44220=CARTESIAN_POINT('Ctrl Pts',(-0.00176567645263645,-0.0339787743898687,
-0.0137455293399189));
#44221=CARTESIAN_POINT('Ctrl Pts',(-0.00187606559832088,-0.0339787743898689,
-0.0135553722231497));
#44222=CARTESIAN_POINT('Ctrl Pts',(-0.00189080530467026,-0.0339787743898689,
-0.0135299815015887));
#44223=CARTESIAN_POINT('Ctrl Pts',(-0.00190505934940457,-0.0339787743898689,
-0.0135043091584398));
#44224=CARTESIAN_POINT('Ctrl Pts',(-0.00191881042213725,-0.0339787743898689,
-0.0134783642158126));
#44225=CARTESIAN_POINT('Ctrl Pts',(-0.00192514106849106,-0.033978774389869,
-0.0134664198199363));
#44226=CARTESIAN_POINT('Ctrl Pts',(-0.00193136505545212,-0.033978774389869,
-0.0134544175408938));
#44227=CARTESIAN_POINT('Ctrl Pts',(-0.00193747420805989,-0.033978774389869,
-0.0134423714900749));
#44228=CARTESIAN_POINT('Ctrl Pts',(-0.00197328449032473,-0.0339787743898691,
-0.0133717606365416));
#44229=CARTESIAN_POINT('Ctrl Pts',(-0.00200521312322471,-0.0339787743898691,
-0.0132995351063943));
#44230=CARTESIAN_POINT('Ctrl Pts',(-0.00203300009904627,-0.0339787743898692,
-0.0132258888697933));
#44231=CARTESIAN_POINT('Ctrl Pts',(-0.00204740119244997,-0.0339787743898693,
-0.013187720400546));
#44232=CARTESIAN_POINT('Ctrl Pts',(-0.00206068903433681,-0.0339787743898693,
-0.0131491701053409));
#44233=CARTESIAN_POINT('Ctrl Pts',(-0.00207282194711271,-0.0339787743898694,
-0.0131102640679554));
#44234=CARTESIAN_POINT('Ctrl Pts',(-0.00211984913524711,-0.0339787743898696,
-0.01295946420864));
#44235=CARTESIAN_POINT('Ctrl Pts',(-0.00214958198481788,-0.0339787743898699,
-0.0128033026699766));
#44236=CARTESIAN_POINT('Ctrl Pts',(-0.00216217348592332,-0.0339787743898701,
-0.0126446198177156));
#44237=CARTESIAN_POINT('Ctrl Pts',(-0.00216315171282087,-0.0339787743898702,
-0.0126322918329138));
#44238=CARTESIAN_POINT('Ctrl Pts',(-0.00216402592998013,-0.0339787743898702,
-0.0126199504008421));
#44239=CARTESIAN_POINT('Ctrl Pts',(-0.00216479558205437,-0.0339787743898702,
-0.0126076087164675));
#44240=CARTESIAN_POINT('Ctrl Pts',(-0.00216967912507767,-0.0339787743898704,
-0.0125292991157523));
#44241=CARTESIAN_POINT('Ctrl Pts',(-0.00217036796979726,-0.0339787743898705,
-0.0124508477717779));
#44242=CARTESIAN_POINT('Ctrl Pts',(-0.00216693899131665,-0.0339787743898707,
-0.0123725957115567));
#44243=CARTESIAN_POINT('Ctrl Pts',(-0.00216352186151759,-0.0339787743898708,
-0.0122946140478242));
#44244=CARTESIAN_POINT('Ctrl Pts',(-0.00215601492434311,-0.0339787743898712,
-0.0122168292977697));
#44245=CARTESIAN_POINT('Ctrl Pts',(-0.00214444540087901,-0.0339787743898705,
-0.0121395948000181));
#44246=CARTESIAN_POINT('Ctrl Pts',(-0.00212839776258705,-0.0339787743898696,
-0.0120324658169251));
#44247=CARTESIAN_POINT('Ctrl Pts',(-0.00210453912761219,-0.0339787743898695,
-0.0119263875876493));
#44248=CARTESIAN_POINT('Ctrl Pts',(-0.00207280590838327,-0.0339787743898694,
-0.0118224055122139));
#44249=CARTESIAN_POINT('Ctrl Pts',(-0.0020692252405201,-0.0339787743898694,
-0.01181067253066));
#44250=CARTESIAN_POINT('Ctrl Pts',(-0.00206554419682896,-0.0339787743898694,
-0.0117989667807872));
#44251=CARTESIAN_POINT('Ctrl Pts',(-0.00206176699337699,-0.0339787743898693,
-0.0117873027340864));
#44252=CARTESIAN_POINT('Ctrl Pts',(-0.00199404940249818,-0.033978774389869,
-0.0115781900525698));
#44253=CARTESIAN_POINT('Ctrl Pts',(-0.00189534055859523,-0.0339787743898688,
-0.0113811715559088));
#44254=CARTESIAN_POINT('Ctrl Pts',(-0.00176552088862998,-0.0339787743898688,
-0.0112050888723163));
#44255=CARTESIAN_POINT('Ctrl Pts',(-0.00174373775123362,-0.0339787743898687,
-0.0111755430162003));
#44256=CARTESIAN_POINT('Ctrl Pts',(-0.00172107260431907,-0.0339787743898687,
-0.0111465939879031));
#44257=CARTESIAN_POINT('Ctrl Pts',(-0.00169751808662202,-0.0339787743898689,
-0.0111182936685626));
#44258=CARTESIAN_POINT('Ctrl Pts',(-0.00212815972946482,-0.0336854482808955,
-0.0108489132294999));
#44259=CARTESIAN_POINT('Ctrl Pts',(-0.00256222339942132,-0.033737507795067,
-0.0115450254415221));
#44260=CARTESIAN_POINT('Ctrl Pts',(-0.00268821701388861,-0.0338416072676536,
-0.0133839745614382));
#44261=CARTESIAN_POINT('Ctrl Pts',(-0.000486973306187236,-0.0339977466986558,
-0.0150849424241983));
#44262=CARTESIAN_POINT('Ctrl Pts',(0.00214464703375922,-0.0341538665739017,
-0.0141970646480211));
#44263=CARTESIAN_POINT('Ctrl Pts',(0.00287363000161765,-0.0343099864491478,
-0.0115187757733854));
#44264=CARTESIAN_POINT('Ctrl Pts',(0.00105188768346137,-0.0344661063243938,
-0.00942187655811136));
#44265=CARTESIAN_POINT('Ctrl Pts',(-0.00170320879371006,-0.0346222261996398,
-0.0097700531871246));
#44266=CARTESIAN_POINT('Ctrl Pts',(-0.00294680945920505,-0.0347783460748859,
-0.012252897597106));
#44267=CARTESIAN_POINT('Ctrl Pts',(-0.0015750623770788,-0.0349344659501319,
-0.0146676160102062));
#44268=CARTESIAN_POINT('Ctrl Pts',(0.00119452509052153,-0.0350905858253779,
-0.0148707633163185));
#44269=CARTESIAN_POINT('Ctrl Pts',(0.00290398577660606,-0.0352467057006239,
-0.0126822455683436));
#44270=CARTESIAN_POINT('Ctrl Pts',(0.00203615063089732,-0.0354028255758699,
-0.0100442688229747));
#44271=CARTESIAN_POINT('Ctrl Pts',(-0.000638764814960264,-0.0355589454511159,
-0.00929809254628702));
#44272=CARTESIAN_POINT('Ctrl Pts',(-0.00274677837741386,-0.035715065326362,
-0.0111059200285361));
#44273=CARTESIAN_POINT('Ctrl Pts',(-0.00241702425108935,-0.035871185201608,
-0.0138633186690574));
#44274=CARTESIAN_POINT('Ctrl Pts',(5.78390342861788E-5,-0.036027305076854,
-0.0151230886392878));
#44275=CARTESIAN_POINT('Ctrl Pts',(0.00248137045250796,-0.0361834249521,
-0.0137671877677982));
#44276=CARTESIAN_POINT('Ctrl Pts',(0.0027026847262315,-0.0363395448273461,
-0.0109989763542873));
#44277=CARTESIAN_POINT('Ctrl Pts',(0.000525365592294934,-0.036495664702592,
-0.00927524394755182));
#44278=CARTESIAN_POINT('Ctrl Pts',(-0.00211821567918175,-0.0366517845778381,
-0.0101258029520302));
#44279=CARTESIAN_POINT('Ctrl Pts',(-0.00288187993770758,-0.0368079044530841,
-0.0127957823649758));
#44280=CARTESIAN_POINT('Ctrl Pts',(-0.00108787485474889,-0.0369640243283302,
-0.0149155744116917));
#44281=CARTESIAN_POINT('Ctrl Pts',(0.00167161934314252,-0.0371201442035761,
-0.0146038633389977));
#44282=CARTESIAN_POINT('Ctrl Pts',(0.00294755115440384,-0.0372762640788222,
-0.0121372923486029));
#44283=CARTESIAN_POINT('Ctrl Pts',(0.00160752995028988,-0.0374323839540682,
-0.00970494474167266));
#44284=CARTESIAN_POINT('Ctrl Pts',(-0.00115917356836235,-0.0375885038293142,
-0.0094655281610616));
#44285=CARTESIAN_POINT('Ctrl Pts',(-0.00289711209160976,-0.0377446237045603,
-0.0116315278692769));
#44286=CARTESIAN_POINT('Ctrl Pts',(-0.0020638591878221,-0.0379007435798062,
-0.0142806128024932));
#44287=CARTESIAN_POINT('Ctrl Pts',(0.000601062435999465,-0.0380568634550523,
-0.0150617302182937));
#44288=CARTESIAN_POINT('Ctrl Pts',(0.00273255420357332,-0.0382129833302983,
-0.0132816173022125));
#44289=CARTESIAN_POINT('Ctrl Pts',(0.0024388779838377,-0.0383691032055443,
-0.0105201647771034));
#44290=CARTESIAN_POINT('Ctrl Pts',(-1.92546192460681E-5,-0.0385252230807903,
-0.00922808595817392));
#44291=CARTESIAN_POINT('Ctrl Pts',(-0.00246039170159155,-0.0386813429560364,
-0.0105522478882585));
#44292=CARTESIAN_POINT('Ctrl Pts',(-0.00271775238336546,-0.0388374628312823,
-0.0133171754567261));
#44293=CARTESIAN_POINT('Ctrl Pts',(-0.000563448104565397,-0.0389935827065284,
-0.0150695329082345));
#44294=CARTESIAN_POINT('Ctrl Pts',(0.00209157012908443,-0.0391497025817744,
-0.0142530712913992));
#44295=CARTESIAN_POINT('Ctrl Pts',(0.00288906432226327,-0.0393058224570205,
-0.0115943779139539));
#44296=CARTESIAN_POINT('Ctrl Pts',(0.00112494460107805,-0.0394619423322664,
-0.00944923592136359));
#44297=CARTESIAN_POINT('Ctrl Pts',(-0.00164299188658567,-0.0396180915523031,
-0.00972899208793168));
#44298=CARTESIAN_POINT('Ctrl Pts',(-0.00250844206789525,-0.0397222008139244,
-0.011356728213131));
#44299=CARTESIAN_POINT('Ctrl Pts',(-0.00250795369641337,-0.0397742701171305,
-0.012177240533185));
#44300=CARTESIAN_POINT('Ctrl Pts',(-0.0019834686101001,-0.0337838939496779,
-0.0109391303497317));
#44301=CARTESIAN_POINT('Ctrl Pts',(-0.00238802079301359,-0.0338359534638493,
-0.0115879146973241));
#44302=CARTESIAN_POINT('Ctrl Pts',(-0.00250544824731082,-0.0339400529364361,
-0.0133018357928247));
#44303=CARTESIAN_POINT('Ctrl Pts',(-0.000453864554152591,-0.0340961923674382,
-0.0148871568173055));
#44304=CARTESIAN_POINT('Ctrl Pts',(0.00199883496163867,-0.0342523122426843,
-0.01405964482454));
#44305=CARTESIAN_POINT('Ctrl Pts',(0.00267825522038416,-0.0344084321179303,
-0.0115634497137735));
#44306=CARTESIAN_POINT('Ctrl Pts',(0.000980371056086661,-0.0345645519931763,
-0.00960911625164863));
#44307=CARTESIAN_POINT('Ctrl Pts',(-0.0015874095971264,-0.0347206718684224,
-0.00993362075422743));
#44308=CARTESIAN_POINT('Ctrl Pts',(-0.00274645929126248,-0.0348767917436684,
-0.0122476594435127));
#44309=CARTESIAN_POINT('Ctrl Pts',(-0.0014679757071952,-0.0350329116189144,
-0.0144982039436755));
#44310=CARTESIAN_POINT('Ctrl Pts',(0.00111331071076243,-0.0351890314941604,
-0.0146875394993302));
#44311=CARTESIAN_POINT('Ctrl Pts',(0.00270654714132937,-0.0353451513694065,
-0.0126478165426109));
#44312=CARTESIAN_POINT('Ctrl Pts',(0.00189771510376056,-0.0355012712446524,
-0.0101891927860523));
#44313=CARTESIAN_POINT('Ctrl Pts',(-0.000595335933750003,-0.0356573911198985,
-0.00949374817166546));
#44314=CARTESIAN_POINT('Ctrl Pts',(-0.00256002809144039,-0.0358135109951445,
-0.0111786635536604));
#44315=CARTESIAN_POINT('Ctrl Pts',(-0.00225269356689315,-0.0359696308703904,
-0.013748589848799));
#44316=CARTESIAN_POINT('Ctrl Pts',(5.39066252202786E-5,-0.0361257507456365,
-0.0149227095153369));
#44317=CARTESIAN_POINT('Ctrl Pts',(0.0023126649444763,-0.0362818706208825,
-0.013658994776367));
#44318=CARTESIAN_POINT('Ctrl Pts',(0.00251893231661951,-0.0364379904961286,
-0.0110789908561722));
#44319=CARTESIAN_POINT('Ctrl Pts',(0.000489646593118128,-0.0365941103713746,
-0.00947245302274003));
#44320=CARTESIAN_POINT('Ctrl Pts',(-0.00197420064429818,-0.0367502302466206,
-0.0102651835039456));
#44321=CARTESIAN_POINT('Ctrl Pts',(-0.00268594425285817,-0.0369063501218667,
-0.0127536341037145));
#44322=CARTESIAN_POINT('Ctrl Pts',(-0.00101391150120779,-0.0370624699971127,
-0.0147293039401408));
#44323=CARTESIAN_POINT('Ctrl Pts',(0.00155796787677828,-0.0372185898723587,
-0.0144387857428698));
#44324=CARTESIAN_POINT('Ctrl Pts',(0.00274715055946227,-0.0373747097476047,
-0.0121399140621891));
#44325=CARTESIAN_POINT('Ctrl Pts',(0.00149823584764362,-0.0375308296228507,
-0.00987293895670145));
#44326=CARTESIAN_POINT('Ctrl Pts',(-0.00108036269772037,-0.0376869494980968,
-0.00964980003258555));
#44327=CARTESIAN_POINT('Ctrl Pts',(-0.00270014079022842,-0.0378430693733427,
-0.0116685359250327));
#44328=CARTESIAN_POINT('Ctrl Pts',(-0.00192353978793748,-0.0379991892485887,
-0.0141375126365903));
#44329=CARTESIAN_POINT('Ctrl Pts',(0.000560196895942137,-0.0381553091238348,
-0.0148655227824418));
#44330=CARTESIAN_POINT('Ctrl Pts',(0.00254677100273285,-0.0383114289990809,
-0.0132064376853053));
#44331=CARTESIAN_POINT('Ctrl Pts',(0.00227306148961988,-0.0384675488743268,
-0.0106327331245048));
#44332=CARTESIAN_POINT('Ctrl Pts',(-1.79455199462971E-5,-0.0386236687495729,
-0.00942850125053447));
#44333=CARTESIAN_POINT('Ctrl Pts',(-0.00229311251457843,-0.0387797886248189,
-0.0106626349420281));
#44334=CARTESIAN_POINT('Ctrl Pts',(-0.00253297554116661,-0.0389359085000649,
-0.0132395782820071));
#44335=CARTESIAN_POINT('Ctrl Pts',(-0.000525139919411454,-0.0390920283753109,
-0.0148727949765153));
#44336=CARTESIAN_POINT('Ctrl Pts',(0.0019493666943436,-0.039248148250557,
-0.0141118436409913));
#44337=CARTESIAN_POINT('Ctrl Pts',(0.00269264017941473,-0.0394042681258029,
-0.0116339117522181));
#44338=CARTESIAN_POINT('Ctrl Pts',(0.00104846091834516,-0.039560388001049,
-0.00963461548342703));
#44339=CARTESIAN_POINT('Ctrl Pts',(-0.00153128676789282,-0.0397165372210856,
-0.00989535135169256));
#44340=CARTESIAN_POINT('Ctrl Pts',(-0.00233789599203442,-0.039820646482707,
-0.0114124195797767));
#44341=CARTESIAN_POINT('Ctrl Pts',(-0.00233744082436491,-0.039872715785913,
-0.0121771462158908));
#44342=CARTESIAN_POINT('Ctrl Pts',(-0.00183877749073539,-0.0338823396184605,
-0.0110293474699636));
#44343=CARTESIAN_POINT('Ctrl Pts',(-0.00221381818660586,-0.0339343991326318,
-0.0116308039531261));
#44344=CARTESIAN_POINT('Ctrl Pts',(-0.00232267948073303,-0.0340384986052186,
-0.0132196970242115));
#44345=CARTESIAN_POINT('Ctrl Pts',(-0.000420755802117943,-0.0341946380362207,
-0.0146893712104127));
#44346=CARTESIAN_POINT('Ctrl Pts',(0.00185302288951808,-0.0343507579114667,
-0.0139222250010588));
#44347=CARTESIAN_POINT('Ctrl Pts',(0.00248288043915068,-0.0345068777867127,
-0.0116081236541615));
#44348=CARTESIAN_POINT('Ctrl Pts',(0.000908854428711957,-0.0346629976619587,
-0.00979635594518588));
#44349=CARTESIAN_POINT('Ctrl Pts',(-0.00147161040054275,-0.0348191175372048,
-0.0100971883213302));
#44350=CARTESIAN_POINT('Ctrl Pts',(-0.00254610912331991,-0.0349752374124508,
-0.0122424212899195));
#44351=CARTESIAN_POINT('Ctrl Pts',(-0.00136088903731159,-0.0351313572876969,
-0.014328791877145));
#44352=CARTESIAN_POINT('Ctrl Pts',(0.00103209633100332,-0.0352874771629428,
-0.014504315682342));
#44353=CARTESIAN_POINT('Ctrl Pts',(0.00250910850605269,-0.0354435970381888,
-0.0126133875168781));
#44354=CARTESIAN_POINT('Ctrl Pts',(0.00175927957662378,-0.0355997169134349,
-0.0103341167491299));
#44355=CARTESIAN_POINT('Ctrl Pts',(-0.000551907052539744,-0.0357558367886809,
-0.00968940379704389));
#44356=CARTESIAN_POINT('Ctrl Pts',(-0.00237327780546691,-0.035911956663927,
-0.0112514070787846));
#44357=CARTESIAN_POINT('Ctrl Pts',(-0.00208836288269695,-0.036068076539173,
-0.0136338610285404));
#44358=CARTESIAN_POINT('Ctrl Pts',(4.99742161543771E-5,-0.036224196414419,
-0.014722330391386));
#44359=CARTESIAN_POINT('Ctrl Pts',(0.00214395943644463,-0.036380316289665,
-0.0135508017849357));
#44360=CARTESIAN_POINT('Ctrl Pts',(0.00233517990700753,-0.036536436164911,
-0.0111590053580572));
#44361=CARTESIAN_POINT('Ctrl Pts',(0.000453927593941321,-0.036692556040157,
-0.00966966209792823));
#44362=CARTESIAN_POINT('Ctrl Pts',(-0.00183018560941461,-0.036848675915403,
-0.0104045640558609));
#44363=CARTESIAN_POINT('Ctrl Pts',(-0.00249000856800876,-0.0370047957906491,
-0.0127114858424534));
#44364=CARTESIAN_POINT('Ctrl Pts',(-0.000939948147666684,-0.0371609156658951,
-0.0145430334685901));
#44365=CARTESIAN_POINT('Ctrl Pts',(0.00144431641041405,-0.0373170355411411,
-0.0142737081467419));
#44366=CARTESIAN_POINT('Ctrl Pts',(0.00254674996452071,-0.0374731554163872,
-0.0121425357757755));
#44367=CARTESIAN_POINT('Ctrl Pts',(0.00138894174499737,-0.0376292752916331,
-0.0100409331717302));
#44368=CARTESIAN_POINT('Ctrl Pts',(-0.00100155182707838,-0.0377853951668792,
-0.00983407190410951));
#44369=CARTESIAN_POINT('Ctrl Pts',(-0.00250316948884707,-0.0379415150421252,
-0.0117055439807884));
#44370=CARTESIAN_POINT('Ctrl Pts',(-0.00178322038805286,-0.0380976349173713,
-0.0139944124706875));
#44371=CARTESIAN_POINT('Ctrl Pts',(0.000519331355884811,-0.0382537547926173,
-0.0146693153465899));
#44372=CARTESIAN_POINT('Ctrl Pts',(0.00236098780189238,-0.0384098746678633,
-0.0131312580683982));
#44373=CARTESIAN_POINT('Ctrl Pts',(0.00210724499540203,-0.0385659945431093,
-0.0107453014719063));
#44374=CARTESIAN_POINT('Ctrl Pts',(-1.66364206465234E-5,-0.0387221144183553,
-0.00962891654289501));
#44375=CARTESIAN_POINT('Ctrl Pts',(-0.00212583332756533,-0.0388782342936013,
-0.0107730219957976));
#44376=CARTESIAN_POINT('Ctrl Pts',(-0.00234819869896776,-0.0390343541688473,
-0.013161981107288));
#44377=CARTESIAN_POINT('Ctrl Pts',(-0.000486831734257513,-0.0391904740440934,
-0.0146760570447959));
#44378=CARTESIAN_POINT('Ctrl Pts',(0.00180716325960277,-0.0393465939193394,
-0.0139706159905834));
#44379=CARTESIAN_POINT('Ctrl Pts',(0.00249621603656618,-0.0395027137945854,
-0.0116734455904824));
#44380=CARTESIAN_POINT('Ctrl Pts',(0.000971977235612279,-0.0396588336698314,
-0.00981999504549048));
#44381=CARTESIAN_POINT('Ctrl Pts',(-0.00141958164919996,-0.039814982889868,
-0.0100617106154535));
#44382=CARTESIAN_POINT('Ctrl Pts',(-0.00216734991617357,-0.0399190921514895,
-0.0114681109464222));
#44383=CARTESIAN_POINT('Ctrl Pts',(-0.00216692795231646,-0.0399711614546955,
-0.0121770518985966));
#44384=CARTESIAN_POINT('Ctrl Pts',(-0.00169408637137068,-0.033980785287243,
-0.0111195645901954));
#44385=CARTESIAN_POINT('Ctrl Pts',(-0.00203961558019815,-0.0340328448014143,
-0.0116736932089283));
#44386=CARTESIAN_POINT('Ctrl Pts',(-0.00213991071415524,-0.0341369442740011,
-0.0131375582555982));
#44387=CARTESIAN_POINT('Ctrl Pts',(-0.000387647050083297,-0.0342930837050033,
-0.01449158560352));
#44388=CARTESIAN_POINT('Ctrl Pts',(0.00170721081739751,-0.0344492035802493,
-0.0137848051775777));
#44389=CARTESIAN_POINT('Ctrl Pts',(0.00228750565791722,-0.0346053234554953,
-0.0116527975945495));
#44390=CARTESIAN_POINT('Ctrl Pts',(0.000837337801337254,-0.0347614433307413,
-0.00998359563872313));
#44391=CARTESIAN_POINT('Ctrl Pts',(-0.0013558112039591,-0.0349175632059874,
-0.0102607558884331));
#44392=CARTESIAN_POINT('Ctrl Pts',(-0.00234575895537733,-0.0350736830812333,
-0.0122371831363263));
#44393=CARTESIAN_POINT('Ctrl Pts',(-0.00125380236742799,-0.0352298029564794,
-0.0141593798106144));
#44394=CARTESIAN_POINT('Ctrl Pts',(0.000950881951244222,-0.0353859228317254,
-0.0143210918653538));
#44395=CARTESIAN_POINT('Ctrl Pts',(0.00231166987077602,-0.0355420427069714,
-0.0125789584911453));
#44396=CARTESIAN_POINT('Ctrl Pts',(0.00162084404948703,-0.0356981625822174,
-0.0104790407122077));
#44397=CARTESIAN_POINT('Ctrl Pts',(-0.000508478171329484,-0.0358542824574634,
-0.00988505942242233));
#44398=CARTESIAN_POINT('Ctrl Pts',(-0.00218652751949343,-0.0360104023327094,
-0.0113241506039089));
#44399=CARTESIAN_POINT('Ctrl Pts',(-0.00192403219850073,-0.0361665222079555,
-0.013519132208282));
#44400=CARTESIAN_POINT('Ctrl Pts',(4.60418070884753E-5,-0.0363226420832015,
-0.0145219512674351));
#44401=CARTESIAN_POINT('Ctrl Pts',(0.00197525392841297,-0.0364787619584476,
-0.0134426087935045));
#44402=CARTESIAN_POINT('Ctrl Pts',(0.00215142749739555,-0.0366348818336936,
-0.0112390198599422));
#44403=CARTESIAN_POINT('Ctrl Pts',(0.000418208594764515,-0.0367910017089396,
-0.00986687117311645));
#44404=CARTESIAN_POINT('Ctrl Pts',(-0.00168617057453104,-0.0369471215841856,
-0.0105439446077764));
#44405=CARTESIAN_POINT('Ctrl Pts',(-0.00229407288315936,-0.0371032414594316,
-0.0126693375811922));
#44406=CARTESIAN_POINT('Ctrl Pts',(-0.000865984794125582,-0.0372593613346777,
-0.0143567629970394));
#44407=CARTESIAN_POINT('Ctrl Pts',(0.00133066494404982,-0.0374154812099236,
-0.014108630550614));
#44408=CARTESIAN_POINT('Ctrl Pts',(0.00234634936957914,-0.0375716010851697,
-0.0121451574893616));
#44409=CARTESIAN_POINT('Ctrl Pts',(0.00127964764235112,-0.0377277209604157,
-0.010208927386759));
#44410=CARTESIAN_POINT('Ctrl Pts',(-0.000922740956436404,-0.0378838408356617,
-0.0100183437756335));
#44411=CARTESIAN_POINT('Ctrl Pts',(-0.00230619818746574,-0.0380399607109077,
-0.0117425520365441));
#44412=CARTESIAN_POINT('Ctrl Pts',(-0.00164290098816823,-0.0381960805861538,
-0.0138513123047845));
#44413=CARTESIAN_POINT('Ctrl Pts',(0.000478465815827482,-0.0383522004613998,
-0.014473107910738));
#44414=CARTESIAN_POINT('Ctrl Pts',(0.0021752046010519,-0.0385083203366458,
-0.0130560784514912));
#44415=CARTESIAN_POINT('Ctrl Pts',(0.0019414285011842,-0.0386644402118919,
-0.0108578698193078));
#44416=CARTESIAN_POINT('Ctrl Pts',(-1.53273213467499E-5,-0.0388205600871378,
-0.00982933183525555));
#44417=CARTESIAN_POINT('Ctrl Pts',(-0.00195855414055221,-0.0389766799623838,
-0.0108834090495671));
#44418=CARTESIAN_POINT('Ctrl Pts',(-0.00216342185676891,-0.0391327998376299,
-0.0130843839325688));
#44419=CARTESIAN_POINT('Ctrl Pts',(-0.000448523549103574,-0.0392889197128759,
-0.0144793191130766));
#44420=CARTESIAN_POINT('Ctrl Pts',(0.00166495982486194,-0.0394450395881219,
-0.0138293883401754));
#44421=CARTESIAN_POINT('Ctrl Pts',(0.00229979189371764,-0.039601159463368,
-0.0117129794287466));
#44422=CARTESIAN_POINT('Ctrl Pts',(0.000895493552879401,-0.039757279338614,
-0.010005374607554));
#44423=CARTESIAN_POINT('Ctrl Pts',(-0.00130787653050712,-0.0399134285586506,
-0.0102280698792143));
#44424=CARTESIAN_POINT('Ctrl Pts',(-0.00199680384031273,-0.0400175378202719,
-0.0115238023130677));
#44425=CARTESIAN_POINT('Ctrl Pts',(-0.001996415080268,-0.040069607123478,
-0.0121769575813024));
#44426=CARTESIAN_POINT('Origin',(0.,-0.0462787743898723,-0.0121758532865581));
#44427=CARTESIAN_POINT('',(0.,0.,0.));
#44428=CARTESIAN_POINT('Ctrl Pts',(-0.0157884048591435,-0.0420671254389844,
-0.00338750223744593));
#44429=CARTESIAN_POINT('Ctrl Pts',(-0.0157173431715818,-0.0421026592929782,
-0.0033519683834522));
#44430=CARTESIAN_POINT('Ctrl Pts',(-0.0155636558736841,-0.0421616223021478,
-0.0032930053742826));
#44431=CARTESIAN_POINT('Ctrl Pts',(-0.015159650326158,-0.0422415979526153,
-0.00321302972381513));
#44432=CARTESIAN_POINT('Ctrl Pts',(-0.0148456426300394,-0.0422591074225579,
-0.00319552025387248));
#44433=CARTESIAN_POINT('Ctrl Pts',(-0.0147000397563992,-0.0422591044750182,
-0.00319552320141217));
#44434=CARTESIAN_POINT('Ctrl Pts',(-0.0157528787075658,-0.0421381807912534,
-0.00342302785458162));
#44435=CARTESIAN_POINT('Ctrl Pts',(-0.0156824358684872,-0.0421664366105109,
-0.00338793404912082));
#44436=CARTESIAN_POINT('Ctrl Pts',(-0.0155288204070857,-0.0422151679902414,
-0.00332877315343381));
#44437=CARTESIAN_POINT('Ctrl Pts',(-0.0151292237928858,-0.0422873985837832,
-0.00325294897397118));
#44438=CARTESIAN_POINT('Ctrl Pts',(-0.0148375584890053,-0.042302815988272,
-0.00323922980950275));
#44439=CARTESIAN_POINT('Ctrl Pts',(-0.0147000438396441,-0.0423053858040627,
-0.00324180453020668));
#44440=CARTESIAN_POINT('Ctrl Pts',(-0.0156744511200191,-0.0422592722231825,
-0.00350145526245708));
#44441=CARTESIAN_POINT('Ctrl Pts',(-0.0156040258414969,-0.0422778860192918,
-0.00346670011416197));
#44442=CARTESIAN_POINT('Ctrl Pts',(-0.0154465327860142,-0.0423135447464296,
-0.00340860687607781));
#44443=CARTESIAN_POINT('Ctrl Pts',(-0.015057946353037,-0.0423722576286869,
-0.00334646106679692));
#44444=CARTESIAN_POINT('Ctrl Pts',(-0.0148199479540628,-0.0423811726973118,
-0.00333924835453889));
#44445=CARTESIAN_POINT('Ctrl Pts',(-0.0147000527348183,-0.0423857572179057,
-0.00334654796809966));
#44446=CARTESIAN_POINT('Ctrl Pts',(-0.0154683605023745,-0.0424274066208669,
-0.00370754740791061));
#44447=CARTESIAN_POINT('Ctrl Pts',(-0.0153984617189363,-0.0424344514374246,
-0.00366923932138871));
#44448=CARTESIAN_POINT('Ctrl Pts',(-0.0152393099806225,-0.0424501760183733,
-0.0036057457320669));
#44449=CARTESIAN_POINT('Ctrl Pts',(-0.0149608392286012,-0.0424602418154941,
-0.00353217877322852));
#44450=CARTESIAN_POINT('Ctrl Pts',(-0.0147915700499568,-0.0424596290594207,
-0.00352111890571466));
#44451=CARTESIAN_POINT('Ctrl Pts',(-0.0147000670678934,-0.0424615469535684,
-0.00352952438408725));
#44452=CARTESIAN_POINT('Ctrl Pts',(-0.0153031604679818,-0.0424787830360679,
-0.00387274336261303));
#44453=CARTESIAN_POINT('Ctrl Pts',(-0.0152490565373728,-0.0424787818503424,
-0.00382672158200888));
#44454=CARTESIAN_POINT('Ctrl Pts',(-0.0151294062024839,-0.0424787792037381,
-0.00374633773382312));
#44455=CARTESIAN_POINT('Ctrl Pts',(-0.0149205641771022,-0.0424787775093944,
-0.00366927823060112));
#44456=CARTESIAN_POINT('Ctrl Pts',(-0.0147740219052253,-0.0424787776124787,
-0.00365678806556642));
#44457=CARTESIAN_POINT('Ctrl Pts',(-0.0147000759302474,-0.0424787772896768,
-0.00366042730492668));
#44458=CARTESIAN_POINT('Ctrl Pts',(-0.0152303498648171,-0.0424787743876894,
-0.00394555014548032));
#44459=CARTESIAN_POINT('Ctrl Pts',(-0.0151840750377049,-0.0424787743879888,
-0.0038992671324187));
#44460=CARTESIAN_POINT('Ctrl Pts',(-0.0150793499745268,-0.042478774388657,
-0.0038188996061916));
#44461=CARTESIAN_POINT('Ctrl Pts',(-0.0148964045588548,-0.0424787743890847,
-0.0037431163626244));
#44462=CARTESIAN_POINT('Ctrl Pts',(-0.014765526907758,-0.0424787743890587,
-0.00372588526759391));
#44463=CARTESIAN_POINT('Ctrl Pts',(-0.0147000802206811,-0.0424787743891402,
-0.00372588633138974));
#44464=CARTESIAN_POINT('',(-0.0157883689862958,-0.0420671433761681,-0.00338748430026228));
#44465=CARTESIAN_POINT('',(-0.0147001132585517,-0.0422591044757622,-0.0031955232006682));
#44466=CARTESIAN_POINT('Ctrl Pts',(-0.0157883689863059,-0.0420671433761781,
-0.00338748430025228));
#44467=CARTESIAN_POINT('Ctrl Pts',(-0.0157173173078478,-0.0421026692154071,
-0.00335195846102329));
#44468=CARTESIAN_POINT('Ctrl Pts',(-0.0155636332119379,-0.0421616267882068,
-0.00329300088822358));
#44469=CARTESIAN_POINT('Ctrl Pts',(-0.0151596729879242,-0.0422415934665763,
-0.00321303420985414));
#44470=CARTESIAN_POINT('Ctrl Pts',(-0.0148456954718,-0.0422591044757722,
-0.0031955232006582));
#44471=CARTESIAN_POINT('Ctrl Pts',(-0.0147001132585417,-0.0422591044757722,
-0.0031955232006582));
#44472=CARTESIAN_POINT('',(-0.0152303632585517,-0.0424787743898723,-0.00394549002800645));
#44473=CARTESIAN_POINT('Ctrl Pts',(-0.0157883689863059,-0.0420671433761781,
-0.00338748430025228));
#44474=CARTESIAN_POINT('Ctrl Pts',(-0.0157528431470768,-0.0421381950546361,
-0.00342301013948126));
#44475=CARTESIAN_POINT('Ctrl Pts',(-0.0156744155682287,-0.0422592816194792,
-0.00350143771832943));
#44476=CARTESIAN_POINT('Ctrl Pts',(-0.0154683367770566,-0.0424274007458997,
-0.00370751650950155));
#44477=CARTESIAN_POINT('Ctrl Pts',(-0.0153031609543063,-0.0424787743898823,
-0.00387269233225182));
#44478=CARTESIAN_POINT('Ctrl Pts',(-0.0152303632585616,-0.0424787743898823,
-0.00394549002799644));
#44479=CARTESIAN_POINT('',(-0.0147001132585517,-0.0424787743898723,-0.00372585328655811));
#44480=CARTESIAN_POINT('Origin',(-0.0147001132585417,-0.0424787743898823,
-0.00447574002801644));
#44481=CARTESIAN_POINT('Origin',(-0.0147001132585417,-0.0417287743898823,
-0.00372585328654811));
#44482=CARTESIAN_POINT('Ctrl Pts',(-0.0157883510491122,-0.0420671254389845,
-0.0033874484274146));
#44483=CARTESIAN_POINT('Ctrl Pts',(-0.0157528254319766,-0.0421381807912534,
-0.00342297457899241));
#44484=CARTESIAN_POINT('Ctrl Pts',(-0.0156743980241011,-0.0422592722231825,
-0.00350140216653908));
#44485=CARTESIAN_POINT('Ctrl Pts',(-0.0154683058786476,-0.0424274066208669,
-0.00370749278418372));
#44486=CARTESIAN_POINT('Ctrl Pts',(-0.0153031099239451,-0.042478783036068,
-0.00387269281857635));
#44487=CARTESIAN_POINT('Ctrl Pts',(-0.0152303031410779,-0.0424787743876895,
-0.00394550342174105));
#44488=CARTESIAN_POINT('Ctrl Pts',(-0.0158238849031059,-0.0421026592929782,
-0.00345851011497633));
#44489=CARTESIAN_POINT('Ctrl Pts',(-0.0157879192374373,-0.0421664366105109,
-0.00349341741807102));
#44490=CARTESIAN_POINT('Ctrl Pts',(-0.0157091531723962,-0.0422778860192918,
-0.00357182744506125));
#44491=CARTESIAN_POINT('Ctrl Pts',(-0.0155066139651694,-0.0424344514374246,
-0.00377739156762176));
#44492=CARTESIAN_POINT('Ctrl Pts',(-0.0153491317045492,-0.0424787818503424,
-0.00392679674918539));
#44493=CARTESIAN_POINT('Ctrl Pts',(-0.0152765861541394,-0.0424787743879888,
-0.00399177824885321));
#44494=CARTESIAN_POINT('Ctrl Pts',(-0.0158828479122755,-0.0421616223021478,
-0.00361219741287408));
#44495=CARTESIAN_POINT('Ctrl Pts',(-0.0158470801331243,-0.0422151679902414,
-0.00364703287947237));
#44496=CARTESIAN_POINT('Ctrl Pts',(-0.0157672464104804,-0.0423135447464296,
-0.00372932050054389));
#44497=CARTESIAN_POINT('Ctrl Pts',(-0.0155701075544912,-0.0424501760183733,
-0.0039365433059356));
#44498=CARTESIAN_POINT('Ctrl Pts',(-0.015429515552735,-0.0424787792037381,
-0.00404644708407416));
#44499=CARTESIAN_POINT('Ctrl Pts',(-0.0153569536803665,-0.042478774388657,
-0.00409650331203122));
#44500=CARTESIAN_POINT('Ctrl Pts',(-0.0159628235627429,-0.0422415979526153,
-0.00401620296040003));
#44501=CARTESIAN_POINT('Ctrl Pts',(-0.015922904312587,-0.0422873985837832,
-0.00404662949367233));
#44502=CARTESIAN_POINT('Ctrl Pts',(-0.0158293922197611,-0.0423722576286869,
-0.00411790693352109));
#44503=CARTESIAN_POINT('Ctrl Pts',(-0.0156436745133296,-0.0424602418154941,
-0.00421501405795683));
#44504=CARTESIAN_POINT('Ctrl Pts',(-0.0155065750559569,-0.0424787775093944,
-0.00425528910945595));
#44505=CARTESIAN_POINT('Ctrl Pts',(-0.0154327369239338,-0.0424787743890847,
-0.00427944872770332));
#44506=CARTESIAN_POINT('Ctrl Pts',(-0.0159803330326856,-0.0422591074225579,
-0.00433021065651868));
#44507=CARTESIAN_POINT('Ctrl Pts',(-0.0159366234770553,-0.042302815988272,
-0.00433829479755283));
#44508=CARTESIAN_POINT('Ctrl Pts',(-0.0158366049320192,-0.0423811726973118,
-0.00435590533249528));
#44509=CARTESIAN_POINT('Ctrl Pts',(-0.0156547343808434,-0.0424596290594207,
-0.0043842832366013));
#44510=CARTESIAN_POINT('Ctrl Pts',(-0.0155190652209917,-0.0424787776124787,
-0.00440183138133276));
#44511=CARTESIAN_POINT('Ctrl Pts',(-0.0154499680189642,-0.0424787743890587,
-0.00441032637880006));
#44512=CARTESIAN_POINT('Ctrl Pts',(-0.0159803300851459,-0.0422591044750182,
-0.00447581353015889));
#44513=CARTESIAN_POINT('Ctrl Pts',(-0.0159340487563514,-0.0423053858040627,
-0.004475809446914));
#44514=CARTESIAN_POINT('Ctrl Pts',(-0.0158293053184584,-0.0423857572179057,
-0.00447580055173977));
#44515=CARTESIAN_POINT('Ctrl Pts',(-0.0156463289024708,-0.0424615469535684,
-0.0044757862186647));
#44516=CARTESIAN_POINT('Ctrl Pts',(-0.0155154259816315,-0.0424787772896768,
-0.0044757773563107));
#44517=CARTESIAN_POINT('Ctrl Pts',(-0.0154499669551684,-0.0424787743891402,
-0.00447577306587701));
#44518=CARTESIAN_POINT('',(-0.0159803300858899,-0.0422591044757622,-0.00447574002800645));
#44519=CARTESIAN_POINT('Ctrl Pts',(-0.0157883689863059,-0.0420671433761781,
-0.00338748430025228));
#44520=CARTESIAN_POINT('Ctrl Pts',(-0.0158238948255348,-0.0421026692154071,
-0.00345853597871023));
#44521=CARTESIAN_POINT('Ctrl Pts',(-0.0158828523983345,-0.0421616267882069,
-0.00361222007462022));
#44522=CARTESIAN_POINT('Ctrl Pts',(-0.0159628190767039,-0.0422415934665763,
-0.00401618029863389));
#44523=CARTESIAN_POINT('Ctrl Pts',(-0.0159803300858999,-0.0422591044757722,
-0.00433015781475808));
#44524=CARTESIAN_POINT('Ctrl Pts',(-0.0159803300858999,-0.0422591044757722,
-0.00447574002801644));
#44525=CARTESIAN_POINT('',(-0.01545,-0.0424787743898723,-0.00447574002800645));
#44526=CARTESIAN_POINT('Origin',(-0.01545000000001,-0.0417287743898823,
-0.00447574002801644));
#44527=CARTESIAN_POINT('Origin',(-0.0147001132585417,-0.0424787743898823,
-0.00447574002801644));
#44528=CARTESIAN_POINT('Ctrl Pts',(-0.0157883510491121,-0.0420671254389844,
-0.00338744842741457));
#44529=CARTESIAN_POINT('Ctrl Pts',(-0.0158238849031059,-0.0421026592929782,
-0.00345851011497631));
#44530=CARTESIAN_POINT('Ctrl Pts',(-0.0158828479122755,-0.0421616223021478,
-0.00361219741287406));
#44531=CARTESIAN_POINT('Ctrl Pts',(-0.0159628235627429,-0.0422415979526153,
-0.00401620296040005));
#44532=CARTESIAN_POINT('Ctrl Pts',(-0.0159803330326856,-0.0422591074225579,
-0.00433021065651872));
#44533=CARTESIAN_POINT('Ctrl Pts',(-0.0159803300851459,-0.0422591044750182,
-0.00447581353015895));
#44534=CARTESIAN_POINT('Ctrl Pts',(-0.0158594064013811,-0.0420315998218488,
-0.00342297457899238));
#44535=CARTESIAN_POINT('Ctrl Pts',(-0.0158876622206386,-0.0420666936273096,
-0.003493417418071));
#44536=CARTESIAN_POINT('Ctrl Pts',(-0.0159363936003691,-0.0421258545229966,
-0.00364703287947235));
#44537=CARTESIAN_POINT('Ctrl Pts',(-0.0160086241939108,-0.0422016787024593,
-0.00404662949367235));
#44538=CARTESIAN_POINT('Ctrl Pts',(-0.0160240415983997,-0.0422153978669277,
-0.00433829479755287));
#44539=CARTESIAN_POINT('Ctrl Pts',(-0.0160266114141903,-0.0422128231462237,
-0.00447580944691406));
#44540=CARTESIAN_POINT('Ctrl Pts',(-0.0159804978333101,-0.0419531724139733,
-0.00350140216653905));
#44541=CARTESIAN_POINT('Ctrl Pts',(-0.0159991116294195,-0.0419879275622684,
-0.00357182744506123));
#44542=CARTESIAN_POINT('Ctrl Pts',(-0.0160347703565572,-0.0420460208003526,
-0.00372932050054387));
#44543=CARTESIAN_POINT('Ctrl Pts',(-0.0160934832388146,-0.0421081666096335,
-0.00411790693352111));
#44544=CARTESIAN_POINT('Ctrl Pts',(-0.0161023983074396,-0.0421153793218916,
-0.00435590533249531));
#44545=CARTESIAN_POINT('Ctrl Pts',(-0.0161069828280333,-0.0421080797083308,
-0.00447580055173983));
#44546=CARTESIAN_POINT('Ctrl Pts',(-0.0161486322309946,-0.0417470802685198,
-0.00370749278418369));
#44547=CARTESIAN_POINT('Ctrl Pts',(-0.0161556770475524,-0.0417853883550417,
-0.00377739156762175));
#44548=CARTESIAN_POINT('Ctrl Pts',(-0.0161714016285009,-0.0418488819443635,
-0.00393654330593559));
#44549=CARTESIAN_POINT('Ctrl Pts',(-0.0161814674256218,-0.0419224489032019,
-0.00421501405795684));
#44550=CARTESIAN_POINT('Ctrl Pts',(-0.0161808546695484,-0.0419335087707158,
-0.00438428323660133));
#44551=CARTESIAN_POINT('Ctrl Pts',(-0.0161827725636961,-0.0419251032923432,
-0.00447578621866474));
#44552=CARTESIAN_POINT('Ctrl Pts',(-0.0162000086461957,-0.0415818843138174,
-0.00387269281857635));
#44553=CARTESIAN_POINT('Ctrl Pts',(-0.0162000074604701,-0.0416279060944215,
-0.00392679674918539));
#44554=CARTESIAN_POINT('Ctrl Pts',(-0.0162000048138658,-0.0417082899426073,
-0.00404644708407417));
#44555=CARTESIAN_POINT('Ctrl Pts',(-0.0162000031195221,-0.0417853494458292,
-0.00425528910945597));
#44556=CARTESIAN_POINT('Ctrl Pts',(-0.0162000032226064,-0.041797839610864,
-0.00440183138133279));
#44557=CARTESIAN_POINT('Ctrl Pts',(-0.0162000028998045,-0.0417942003715037,
-0.00447577735631073));
#44558=CARTESIAN_POINT('Ctrl Pts',(-0.0161999999978171,-0.0415090775309501,
-0.00394550342174106));
#44559=CARTESIAN_POINT('Ctrl Pts',(-0.0161999999981165,-0.0415553605440118,
-0.00399177824885322));
#44560=CARTESIAN_POINT('Ctrl Pts',(-0.0161999999987847,-0.0416357280702388,
-0.00409650331203123));
#44561=CARTESIAN_POINT('Ctrl Pts',(-0.0161999999992124,-0.0417115113138059,
-0.00427944872770334));
#44562=CARTESIAN_POINT('Ctrl Pts',(-0.0161999999991864,-0.0417287424088365,
-0.00441032637880008));
#44563=CARTESIAN_POINT('Ctrl Pts',(-0.0161999999992679,-0.0417287413450407,
-0.00447577306587704));
#44564=CARTESIAN_POINT('',(-0.0162,-0.041509137648424,-0.00394549002800645));
#44565=CARTESIAN_POINT('Ctrl Pts',(-0.0157883689863059,-0.0420671433761781,
-0.00338748430025228));
#44566=CARTESIAN_POINT('Ctrl Pts',(-0.0158594206647638,-0.0420316175369492,
-0.00342301013948126));
#44567=CARTESIAN_POINT('Ctrl Pts',(-0.0159805072296069,-0.041953189958101,
-0.00350143771832943));
#44568=CARTESIAN_POINT('Ctrl Pts',(-0.0161486263560273,-0.0417471111669288,
-0.00370751650950155));
#44569=CARTESIAN_POINT('Ctrl Pts',(-0.01620000000001,-0.0415819353441786,
-0.00387269233225182));
#44570=CARTESIAN_POINT('Ctrl Pts',(-0.01620000000001,-0.041509137648434,
-0.00394549002799644));
#44571=CARTESIAN_POINT('',(-0.0162,-0.0417287743898723,-0.00447574002800645));
#44572=CARTESIAN_POINT('Origin',(-0.01620000000001,-0.040978887648414,-0.00447574002801644));
#44573=CARTESIAN_POINT('Origin',(-0.01545000000001,-0.0417287743898823,
-0.00447574002801644));
#44574=CARTESIAN_POINT('Ctrl Pts',(-0.0157883510491121,-0.0420671792490158,
-0.00338750223744593));
#44575=CARTESIAN_POINT('Ctrl Pts',(-0.0158594064013811,-0.0420316530974381,
-0.00342302785458162));
#44576=CARTESIAN_POINT('Ctrl Pts',(-0.0159804978333101,-0.0419532255098914,
-0.00350145526245708));
#44577=CARTESIAN_POINT('Ctrl Pts',(-0.0161486322309946,-0.0417471348922468,
-0.00370754740791061));
#44578=CARTESIAN_POINT('Ctrl Pts',(-0.0162000086461957,-0.0415819348578541,
-0.00387274336261302));
#44579=CARTESIAN_POINT('Ctrl Pts',(-0.0161999999978171,-0.0415091242546894,
-0.00394555014548031));
#44580=CARTESIAN_POINT('Ctrl Pts',(-0.0158238849031059,-0.0419961175614541,
-0.0033519683834522));
#44581=CARTESIAN_POINT('Ctrl Pts',(-0.0158876622206386,-0.0419612102583594,
-0.00338793404912082));
#44582=CARTESIAN_POINT('Ctrl Pts',(-0.0159991116294195,-0.0418828002313692,
-0.00346670011416197));
#44583=CARTESIAN_POINT('Ctrl Pts',(-0.0161556770475524,-0.0416772361088086,
-0.0036692393213887));
#44584=CARTESIAN_POINT('Ctrl Pts',(-0.0162000074604701,-0.041527830927245,
-0.00382672158200888));
#44585=CARTESIAN_POINT('Ctrl Pts',(-0.0161999999981165,-0.0414628494275772,
-0.0038992671324187));
#44586=CARTESIAN_POINT('Ctrl Pts',(-0.0158828479122755,-0.0418424302635564,
-0.0032930053742826));
#44587=CARTESIAN_POINT('Ctrl Pts',(-0.0159363936003691,-0.041807594796958,
-0.00332877315343381));
#44588=CARTESIAN_POINT('Ctrl Pts',(-0.0160347703565572,-0.0417253071758865,
-0.00340860687607781));
#44589=CARTESIAN_POINT('Ctrl Pts',(-0.0161714016285009,-0.0415180843704948,
-0.0036057457320669));
#44590=CARTESIAN_POINT('Ctrl Pts',(-0.0162000048138658,-0.0414081805923563,
-0.00374633773382311));
#44591=CARTESIAN_POINT('Ctrl Pts',(-0.0161999999987847,-0.0413581243643992,
-0.00381889960619159));
#44592=CARTESIAN_POINT('Ctrl Pts',(-0.0159628235627429,-0.0414384247160303,
-0.00321302972381512));
#44593=CARTESIAN_POINT('Ctrl Pts',(-0.0160086241939108,-0.0414079981827581,
-0.00325294897397118));
#44594=CARTESIAN_POINT('Ctrl Pts',(-0.0160934832388146,-0.0413367207429093,
-0.00334646106679692));
#44595=CARTESIAN_POINT('Ctrl Pts',(-0.0161814674256218,-0.0412396136184735,
-0.00353217877322852));
#44596=CARTESIAN_POINT('Ctrl Pts',(-0.0162000031195221,-0.0411993385669745,
-0.00366927823060111));
#44597=CARTESIAN_POINT('Ctrl Pts',(-0.0161999999992124,-0.041175178948727,
-0.00374311636262439));
#44598=CARTESIAN_POINT('Ctrl Pts',(-0.0159803330326856,-0.0411244170199117,
-0.00319552025387248));
#44599=CARTESIAN_POINT('Ctrl Pts',(-0.0160240415983997,-0.0411163328788775,
-0.00323922980950275));
#44600=CARTESIAN_POINT('Ctrl Pts',(-0.0161023983074396,-0.0410987223439351,
-0.00333924835453889));
#44601=CARTESIAN_POINT('Ctrl Pts',(-0.0161808546695484,-0.0410703444398291,
-0.00352111890571466));
#44602=CARTESIAN_POINT('Ctrl Pts',(-0.0162000032226064,-0.0410527962950976,
-0.0036567880655664));
#44603=CARTESIAN_POINT('Ctrl Pts',(-0.0161999999991864,-0.0410443012976303,
-0.0037258852675939));
#44604=CARTESIAN_POINT('Ctrl Pts',(-0.0159803300851459,-0.0409788141462715,
-0.00319552320141217));
#44605=CARTESIAN_POINT('Ctrl Pts',(-0.0160266114141903,-0.0409788182295164,
-0.00324180453020668));
#44606=CARTESIAN_POINT('Ctrl Pts',(-0.0161069828280333,-0.0409788271246906,
-0.00334654796809965));
#44607=CARTESIAN_POINT('Ctrl Pts',(-0.0161827725636961,-0.0409788414577657,
-0.00352952438408725));
#44608=CARTESIAN_POINT('Ctrl Pts',(-0.0162000028998045,-0.0409788503201197,
-0.00366042730492668));
#44609=CARTESIAN_POINT('Ctrl Pts',(-0.0161999999992679,-0.0409788546105534,
-0.00372588633138973));
#44610=CARTESIAN_POINT('',(-0.0159803300858899,-0.040978887648424,-0.0031955232006682));
#44611=CARTESIAN_POINT('Ctrl Pts',(-0.0157883689863059,-0.0420671433761781,
-0.00338748430025228));
#44612=CARTESIAN_POINT('Ctrl Pts',(-0.0158238948255348,-0.0419960916977202,
-0.00335195846102329));
#44613=CARTESIAN_POINT('Ctrl Pts',(-0.0158828523983345,-0.0418424076018102,
-0.00329300088822358));
#44614=CARTESIAN_POINT('Ctrl Pts',(-0.0159628190767039,-0.0414384473777965,
-0.00321303420985414));
#44615=CARTESIAN_POINT('Ctrl Pts',(-0.0159803300858999,-0.0411244698616723,
-0.0031955232006582));
#44616=CARTESIAN_POINT('Ctrl Pts',(-0.0159803300858999,-0.040978887648414,
-0.0031955232006582));
#44617=CARTESIAN_POINT('',(-0.0162,-0.040978887648424,-0.00372585328655811));
#44618=CARTESIAN_POINT('Origin',(-0.01545000000001,-0.040978887648414,-0.00372585328654811));
#44619=CARTESIAN_POINT('Origin',(-0.01620000000001,-0.040978887648414,-0.00447574002801644));
#44620=CARTESIAN_POINT('Ctrl Pts',(-0.0157883510491122,-0.0420671792490158,
-0.00338750223744593));
#44621=CARTESIAN_POINT('Ctrl Pts',(-0.0158238849031059,-0.0419961175614541,
-0.0033519683834522));
#44622=CARTESIAN_POINT('Ctrl Pts',(-0.0158828479122755,-0.0418424302635563,
-0.00329300537428259));
#44623=CARTESIAN_POINT('Ctrl Pts',(-0.0159628235627429,-0.0414384247160304,
-0.00321302972381513));
#44624=CARTESIAN_POINT('Ctrl Pts',(-0.0159803330326856,-0.0411244170199117,
-0.00319552025387248));
#44625=CARTESIAN_POINT('Ctrl Pts',(-0.0159803300851459,-0.0409788141462716,
-0.00319552320141217));
#44626=CARTESIAN_POINT('Ctrl Pts',(-0.0157528254319766,-0.0420316530974381,
-0.00331644688517704));
#44627=CARTESIAN_POINT('Ctrl Pts',(-0.0157879192374373,-0.0419612102583594,
-0.00328819106591946));
#44628=CARTESIAN_POINT('Ctrl Pts',(-0.0158470801331243,-0.041807594796958,
-0.00323945968618903));
#44629=CARTESIAN_POINT('Ctrl Pts',(-0.015922904312587,-0.0414079981827581,
-0.00316722909264728));
#44630=CARTESIAN_POINT('Ctrl Pts',(-0.0159366234770553,-0.0411163328788775,
-0.00315181168815843));
#44631=CARTESIAN_POINT('Ctrl Pts',(-0.0159340487563514,-0.0409788182295164,
-0.00314924187236774));
#44632=CARTESIAN_POINT('Ctrl Pts',(-0.0156743980241011,-0.0419532255098914,
-0.00319535545324794));
#44633=CARTESIAN_POINT('Ctrl Pts',(-0.0157091531723962,-0.0418828002313692,
-0.00317674165713853));
#44634=CARTESIAN_POINT('Ctrl Pts',(-0.0157672464104804,-0.0417253071758865,
-0.0031410829300009));
#44635=CARTESIAN_POINT('Ctrl Pts',(-0.0158293922197611,-0.0413367207429093,
-0.00308237004774348));
#44636=CARTESIAN_POINT('Ctrl Pts',(-0.0158366049320192,-0.0410987223439351,
-0.00307345497911859));
#44637=CARTESIAN_POINT('Ctrl Pts',(-0.0158293053184584,-0.0409788271246907,
-0.00306887045852474));
#44638=CARTESIAN_POINT('Ctrl Pts',(-0.0154683058786476,-0.0417471348922467,
-0.00302722105556352));
#44639=CARTESIAN_POINT('Ctrl Pts',(-0.0155066139651694,-0.0416772361088086,
-0.00302017623900574));
#44640=CARTESIAN_POINT('Ctrl Pts',(-0.0155701075544912,-0.0415180843704948,
-0.00300445165805715));
#44641=CARTESIAN_POINT('Ctrl Pts',(-0.0156436745133296,-0.0412396136184735,
-0.00299438586093631));
#44642=CARTESIAN_POINT('Ctrl Pts',(-0.0156547343808434,-0.0410703444398291,
-0.00299499861700969));
#44643=CARTESIAN_POINT('Ctrl Pts',(-0.0156463289024708,-0.0409788414577657,
-0.002993080722862));
#44644=CARTESIAN_POINT('Ctrl Pts',(-0.0153031099239451,-0.0415819348578541,
-0.00297584464036246));
#44645=CARTESIAN_POINT('Ctrl Pts',(-0.0153491317045492,-0.041527830927245,
-0.00297584582608801));
#44646=CARTESIAN_POINT('Ctrl Pts',(-0.015429515552735,-0.0414081805923563,
-0.00297584847269227));
#44647=CARTESIAN_POINT('Ctrl Pts',(-0.0155065750559569,-0.0411993385669745,
-0.00297585016703602));
#44648=CARTESIAN_POINT('Ctrl Pts',(-0.0155190652209917,-0.0410527962950977,
-0.00297585006395169));
#44649=CARTESIAN_POINT('Ctrl Pts',(-0.0155154259816315,-0.0409788503201198,
-0.00297585038675357));
#44650=CARTESIAN_POINT('Ctrl Pts',(-0.0152303031410779,-0.0415091242546894,
-0.00297585328874096));
#44651=CARTESIAN_POINT('Ctrl Pts',(-0.0152765861541394,-0.0414628494275772,
-0.00297585328844161));
#44652=CARTESIAN_POINT('Ctrl Pts',(-0.0153569536803665,-0.0413581243643992,
-0.00297585328777345));
#44653=CARTESIAN_POINT('Ctrl Pts',(-0.0154327369239338,-0.041175178948727,
-0.00297585328734569));
#44654=CARTESIAN_POINT('Ctrl Pts',(-0.0154499680189642,-0.0410443012976304,
-0.00297585328737171));
#44655=CARTESIAN_POINT('Ctrl Pts',(-0.0154499669551684,-0.0409788546105535,
-0.00297585328729021));
#44656=CARTESIAN_POINT('',(-0.0152303632585517,-0.041509137648424,-0.00297585328655811));
#44657=CARTESIAN_POINT('Ctrl Pts',(-0.0157883689863059,-0.0420671433761781,
-0.00338748430025228));
#44658=CARTESIAN_POINT('Ctrl Pts',(-0.0157528431470768,-0.0420316175369492,
-0.00331643262179432));
#44659=CARTESIAN_POINT('Ctrl Pts',(-0.0156744155682287,-0.041953189958101,
-0.00319534605695119));
#44660=CARTESIAN_POINT('Ctrl Pts',(-0.0154683367770566,-0.0417471111669288,
-0.00302722693053075));
#44661=CARTESIAN_POINT('Ctrl Pts',(-0.0153031609543063,-0.0415819353441786,
-0.00297585328654811));
#44662=CARTESIAN_POINT('Ctrl Pts',(-0.0152303632585616,-0.041509137648434,
-0.00297585328654811));
#44663=CARTESIAN_POINT('',(-0.01545,-0.040978887648424,-0.00297585328655811));
#44664=CARTESIAN_POINT('Origin',(-0.0147001132585417,-0.040978887648414,
-0.00297585328654811));
#44665=CARTESIAN_POINT('Origin',(-0.01545000000001,-0.040978887648414,-0.00372585328654811));
#44666=CARTESIAN_POINT('Ctrl Pts',(0.00878840485914476,-0.0420671254389838,
-0.00338750223744656));
#44667=CARTESIAN_POINT('Ctrl Pts',(0.00871734317158273,-0.0421026592929779,
-0.00335196838345255));
#44668=CARTESIAN_POINT('Ctrl Pts',(0.00856365587368485,-0.0421616223021476,
-0.00329300537428275));
#44669=CARTESIAN_POINT('Ctrl Pts',(0.00815965032615725,-0.0422415979526155,
-0.00321302972381497));
#44670=CARTESIAN_POINT('Ctrl Pts',(0.00784564263003751,-0.042259107422558,
-0.00319552025387238));
#44671=CARTESIAN_POINT('Ctrl Pts',(0.00770003975639664,-0.0422591044750182,
-0.00319552320141217));
#44672=CARTESIAN_POINT('Ctrl Pts',(0.00875287870756702,-0.0420315998218482,
-0.00331644688517755));
#44673=CARTESIAN_POINT('Ctrl Pts',(0.00868243586848799,-0.0420666936273092,
-0.00328819106591975));
#44674=CARTESIAN_POINT('Ctrl Pts',(0.00852882040708653,-0.0421258545229965,
-0.00323945968618918));
#44675=CARTESIAN_POINT('Ctrl Pts',(0.00812922379288497,-0.0422016787024594,
-0.00316722909264713));
#44676=CARTESIAN_POINT('Ctrl Pts',(0.00783755848900357,-0.0422153978669278,
-0.00315181168815834));
#44677=CARTESIAN_POINT('Ctrl Pts',(0.00770004383964167,-0.0422128231462237,
-0.0031492418723677));
#44678=CARTESIAN_POINT('Ctrl Pts',(0.00867445112002032,-0.0419531724139727,
-0.00319535545324827));
#44679=CARTESIAN_POINT('Ctrl Pts',(0.00860402584149779,-0.041987927562268,
-0.00317674165713874));
#44680=CARTESIAN_POINT('Ctrl Pts',(0.00844653278601498,-0.0420460208003524,
-0.00314108293000102));
#44681=CARTESIAN_POINT('Ctrl Pts',(0.00805794635303622,-0.0421081666096336,
-0.00308237004774336));
#44682=CARTESIAN_POINT('Ctrl Pts',(0.00781994795406137,-0.0421153793218916,
-0.00307345497911853));
#44683=CARTESIAN_POINT('Ctrl Pts',(0.00770005273481621,-0.0421080797083306,
-0.00306887045852466));
#44684=CARTESIAN_POINT('Ctrl Pts',(0.00846836050237675,-0.0417470802685202,
-0.0030272210555645));
#44685=CARTESIAN_POINT('Ctrl Pts',(0.0083984617189383,-0.0417853883550424,
-0.00302017623900663));
#44686=CARTESIAN_POINT('Ctrl Pts',(0.00823930998062413,-0.0418488819443643,
-0.00300445165805787));
#44687=CARTESIAN_POINT('Ctrl Pts',(0.00796083922860127,-0.041922448903203,
-0.00299438586093674));
#44688=CARTESIAN_POINT('Ctrl Pts',(0.00779157004995592,-0.0419335087707168,
-0.00299499861701009));
#44689=CARTESIAN_POINT('Ctrl Pts',(0.0077000670678918,-0.041925103292344,
-0.00299308072286236));
#44690=CARTESIAN_POINT('Ctrl Pts',(0.00830316046798526,-0.0415818843138191,
-0.00297584464036324));
#44691=CARTESIAN_POINT('Ctrl Pts',(0.00824905653737577,-0.0416279060944235,
-0.00297584582608869));
#44692=CARTESIAN_POINT('Ctrl Pts',(0.008129406202486,-0.0417082899426093,
-0.00297584847269271));
#44693=CARTESIAN_POINT('Ctrl Pts',(0.00792056417710238,-0.0417853494458315,
-0.00297585016703631));
#44694=CARTESIAN_POINT('Ctrl Pts',(0.00777402190522474,-0.0417978396108661,
-0.00297585006395198));
#44695=CARTESIAN_POINT('Ctrl Pts',(0.00770007593024611,-0.0417942003715057,
-0.00297585038675383));
#44696=CARTESIAN_POINT('Ctrl Pts',(0.00823034986482126,-0.0415090775309527,
-0.00297585328874096));
#44697=CARTESIAN_POINT('Ctrl Pts',(0.00818407503770855,-0.0415553605440146,
-0.00297585328844161));
#44698=CARTESIAN_POINT('Ctrl Pts',(0.0080793499745296,-0.041635728070242,
-0.00297585328777345));
#44699=CARTESIAN_POINT('Ctrl Pts',(0.00789640455885557,-0.0417115113138095,
-0.00297585328734569));
#44700=CARTESIAN_POINT('Ctrl Pts',(0.00776552690775766,-0.0417287424088398,
-0.00297585328737171));
#44701=CARTESIAN_POINT('Ctrl Pts',(0.00770008022067996,-0.0417287413450437,
-0.00297585328729021));
#44702=CARTESIAN_POINT('',(0.0087883689862958,-0.0420671433761681,-0.00338748430026228));
#44703=CARTESIAN_POINT('',(0.0077001132585517,-0.0422591044757622,-0.0031955232006682));
#44704=CARTESIAN_POINT('Ctrl Pts',(0.0087883689863058,-0.0420671433761781,
-0.00338748430025228));
#44705=CARTESIAN_POINT('Ctrl Pts',(0.0087173173078479,-0.0421026692154071,
-0.00335195846102329));
#44706=CARTESIAN_POINT('Ctrl Pts',(0.0085636332119379,-0.0421616267882068,
-0.00329300088822358));
#44707=CARTESIAN_POINT('Ctrl Pts',(0.0081596729879242,-0.0422415934665763,
-0.00321303420985414));
#44708=CARTESIAN_POINT('Ctrl Pts',(0.00784569547182,-0.0422591044757722,
-0.0031955232006582));
#44709=CARTESIAN_POINT('Ctrl Pts',(0.0077001132585617,-0.0422591044757722,
-0.0031955232006582));
#44710=CARTESIAN_POINT('',(0.0082303632585517,-0.041509137648424,-0.00297585328655811));
#44711=CARTESIAN_POINT('Ctrl Pts',(0.0087883689863058,-0.0420671433761781,
-0.00338748430025228));
#44712=CARTESIAN_POINT('Ctrl Pts',(0.0087528431470769,-0.0420316175369492,
-0.00331643262179432));
#44713=CARTESIAN_POINT('Ctrl Pts',(0.0086744155682287,-0.041953189958101,
-0.00319534605695119));
#44714=CARTESIAN_POINT('Ctrl Pts',(0.0084683367770566,-0.0417471111669288,
-0.00302722693053075));
#44715=CARTESIAN_POINT('Ctrl Pts',(0.0083031609543063,-0.0415819353441786,
-0.00297585328654811));
#44716=CARTESIAN_POINT('Ctrl Pts',(0.0082303632585617,-0.041509137648434,
-0.00297585328654811));
#44717=CARTESIAN_POINT('',(0.0077001132585517,-0.0417287743898723,-0.00297585328655811));
#44718=CARTESIAN_POINT('Origin',(0.0077001132585617,-0.040978887648414,
-0.00297585328654811));
#44719=CARTESIAN_POINT('Origin',(0.0077001132585617,-0.0417287743898823,
-0.00372585328654811));
#44720=CARTESIAN_POINT('Ctrl Pts',(0.00878835104911207,-0.042067179249016,
-0.00338750223744602));
#44721=CARTESIAN_POINT('Ctrl Pts',(0.00875282543197647,-0.0420316530974382,
-0.00331644688517711));
#44722=CARTESIAN_POINT('Ctrl Pts',(0.00867439802410098,-0.0419532255098915,
-0.00319535545324799));
#44723=CARTESIAN_POINT('Ctrl Pts',(0.00846830587865056,-0.04174713489225,
-0.00302722105556606));
#44724=CARTESIAN_POINT('Ctrl Pts',(0.00830310992395243,-0.0415819348578616,
-0.00297584464036477));
#44725=CARTESIAN_POINT('Ctrl Pts',(0.00823030314108757,-0.0415091242546993,
-0.00297585328874096));
#44726=CARTESIAN_POINT('Ctrl Pts',(0.00882388490310585,-0.0419961175614542,
-0.00335196838345225));
#44727=CARTESIAN_POINT('Ctrl Pts',(0.00878791923743725,-0.0419612102583595,
-0.0032881910659195));
#44728=CARTESIAN_POINT('Ctrl Pts',(0.00870915317239613,-0.0418828002313693,
-0.00317674165713856));
#44729=CARTESIAN_POINT('Ctrl Pts',(0.0085066139651724,-0.0416772361088118,
-0.0030201762390081));
#44730=CARTESIAN_POINT('Ctrl Pts',(0.00834913170455625,-0.0415278309272518,
-0.00297584582609));
#44731=CARTESIAN_POINT('Ctrl Pts',(0.00827658615414919,-0.0414628494275861,
-0.00297585328844161));
#44732=CARTESIAN_POINT('Ctrl Pts',(0.00888284791227546,-0.0418424302635565,
-0.00329300537428262));
#44733=CARTESIAN_POINT('Ctrl Pts',(0.00884708013312432,-0.0418075947969581,
-0.00323945968618904));
#44734=CARTESIAN_POINT('Ctrl Pts',(0.00876724641048024,-0.0417253071758866,
-0.00314108293000092));
#44735=CARTESIAN_POINT('Ctrl Pts',(0.00857010755449411,-0.041518084370498,
-0.0030044516580592));
#44736=CARTESIAN_POINT('Ctrl Pts',(0.00842951555274125,-0.0414081805923613,
-0.00297584847269355));
#44737=CARTESIAN_POINT('Ctrl Pts',(0.0083569536803763,-0.041358124364406,
-0.00297585328777345));
#44738=CARTESIAN_POINT('Ctrl Pts',(0.00896282356274304,-0.0414384247160302,
-0.0032130297238151));
#44739=CARTESIAN_POINT('Ctrl Pts',(0.00892290431258698,-0.041407998182758,
-0.00316722909264726));
#44740=CARTESIAN_POINT('Ctrl Pts',(0.00882939221976126,-0.0413367207429092,
-0.00308237004774346));
#44741=CARTESIAN_POINT('Ctrl Pts',(0.00864367451333237,-0.0412396136184749,
-0.00299438586093763));
#44742=CARTESIAN_POINT('Ctrl Pts',(0.00850657505596322,-0.0411993385669762,
-0.00297585016703686));
#44743=CARTESIAN_POINT('Ctrl Pts',(0.00843273692394366,-0.0411751789487302,
-0.00297585328734569));
#44744=CARTESIAN_POINT('Ctrl Pts',(0.00898033303268563,-0.0411244170199114,
-0.00319552025387247));
#44745=CARTESIAN_POINT('Ctrl Pts',(0.00893662347705534,-0.0411163328788773,
-0.00315181168815842));
#44746=CARTESIAN_POINT('Ctrl Pts',(0.00883660493201919,-0.0410987223439349,
-0.00307345497911858));
#44747=CARTESIAN_POINT('Ctrl Pts',(0.00865473438084623,-0.0410703444398294,
-0.00299499861701086));
#44748=CARTESIAN_POINT('Ctrl Pts',(0.00851906522099781,-0.0410527962950983,
-0.00297585006395255));
#44749=CARTESIAN_POINT('Ctrl Pts',(0.00844996801897355,-0.0410443012976314,
-0.00297585328737171));
#44750=CARTESIAN_POINT('Ctrl Pts',(0.00898033008514593,-0.0409788141462712,
-0.00319552320141217));
#44751=CARTESIAN_POINT('Ctrl Pts',(0.00893404875635143,-0.0409788182295161,
-0.00314924187236774));
#44752=CARTESIAN_POINT('Ctrl Pts',(0.00882930531845842,-0.0409788271246904,
-0.00306887045852473));
#44753=CARTESIAN_POINT('Ctrl Pts',(0.00864632890247355,-0.0409788414577655,
-0.00299308072286314));
#44754=CARTESIAN_POINT('Ctrl Pts',(0.00851542598163733,-0.0409788503201196,
-0.00297585038675435));
#44755=CARTESIAN_POINT('Ctrl Pts',(0.00844996695517721,-0.0409788546105533,
-0.00297585328729021));
#44756=CARTESIAN_POINT('',(0.0089803300858899,-0.040978887648424,-0.0031955232006682));
#44757=CARTESIAN_POINT('Ctrl Pts',(0.0087883689863058,-0.0420671433761781,
-0.00338748430025228));
#44758=CARTESIAN_POINT('Ctrl Pts',(0.0088238948255348,-0.0419960916977202,
-0.00335195846102329));
#44759=CARTESIAN_POINT('Ctrl Pts',(0.0088828523983345,-0.0418424076018102,
-0.00329300088822358));
#44760=CARTESIAN_POINT('Ctrl Pts',(0.008962819076704,-0.0414384473777965,
-0.00321303420985414));
#44761=CARTESIAN_POINT('Ctrl Pts',(0.0089803300858999,-0.0411244698616723,
-0.0031955232006582));
#44762=CARTESIAN_POINT('Ctrl Pts',(0.0089803300858999,-0.040978887648414,
-0.0031955232006582));
#44763=CARTESIAN_POINT('',(0.00845,-0.040978887648424,-0.00297585328655811));
#44764=CARTESIAN_POINT('Origin',(0.00845000000001,-0.040978887648414,-0.00372585328654811));
#44765=CARTESIAN_POINT('Origin',(0.0077001132585617,-0.040978887648414,
-0.00297585328654811));
#44766=CARTESIAN_POINT('Ctrl Pts',(0.00878835104911214,-0.0420671792490158,
-0.00338750223744593));
#44767=CARTESIAN_POINT('Ctrl Pts',(0.00882388490310589,-0.0419961175614541,
-0.0033519683834522));
#44768=CARTESIAN_POINT('Ctrl Pts',(0.00888284791227549,-0.0418424302635564,
-0.0032930053742826));
#44769=CARTESIAN_POINT('Ctrl Pts',(0.00896282356274302,-0.0414384247160304,
-0.00321302972381512));
#44770=CARTESIAN_POINT('Ctrl Pts',(0.00898033303268562,-0.0411244170199117,
-0.00319552025387248));
#44771=CARTESIAN_POINT('Ctrl Pts',(0.00898033008514593,-0.0409788141462715,
-0.00319552320141217));
#44772=CARTESIAN_POINT('Ctrl Pts',(0.00885940640138106,-0.0420316530974381,
-0.00342302785458162));
#44773=CARTESIAN_POINT('Ctrl Pts',(0.00888766222063862,-0.0419612102583594,
-0.00338793404912082));
#44774=CARTESIAN_POINT('Ctrl Pts',(0.00893639360036903,-0.041807594796958,
-0.00332877315343381));
#44775=CARTESIAN_POINT('Ctrl Pts',(0.00900862419391088,-0.0414079981827581,
-0.00325294897397118));
#44776=CARTESIAN_POINT('Ctrl Pts',(0.00902404159839969,-0.0411163328788775,
-0.00323922980950275));
#44777=CARTESIAN_POINT('Ctrl Pts',(0.00902661141419034,-0.0409788182295164,
-0.00324180453020668));
#44778=CARTESIAN_POINT('Ctrl Pts',(0.00898049783331014,-0.0419532255098914,
-0.00350145526245707));
#44779=CARTESIAN_POINT('Ctrl Pts',(0.00899911162941954,-0.0418828002313692,
-0.00346670011416197));
#44780=CARTESIAN_POINT('Ctrl Pts',(0.00903477035655726,-0.0417253071758865,
-0.0034086068760778));
#44781=CARTESIAN_POINT('Ctrl Pts',(0.00909348323881464,-0.0413367207429093,
-0.00334646106679692));
#44782=CARTESIAN_POINT('Ctrl Pts',(0.00910239830743949,-0.0410987223439351,
-0.00333924835453889));
#44783=CARTESIAN_POINT('Ctrl Pts',(0.00910698282803342,-0.0409788271246906,
-0.00334654796809965));
#44784=CARTESIAN_POINT('Ctrl Pts',(0.00914863223099463,-0.0417471348922468,
-0.00370754740791059));
#44785=CARTESIAN_POINT('Ctrl Pts',(0.00915567704755241,-0.0416772361088086,
-0.0036692393213887));
#44786=CARTESIAN_POINT('Ctrl Pts',(0.00917140162850093,-0.0415180843704948,
-0.0036057457320669));
#44787=CARTESIAN_POINT('Ctrl Pts',(0.00918146742562174,-0.0412396136184735,
-0.00353217877322852));
#44788=CARTESIAN_POINT('Ctrl Pts',(0.00918085466954842,-0.0410703444398291,
-0.00352111890571465));
#44789=CARTESIAN_POINT('Ctrl Pts',(0.00918277256369609,-0.0409788414577657,
-0.00352952438408724));
#44790=CARTESIAN_POINT('Ctrl Pts',(0.00920000864619565,-0.0415819348578541,
-0.00387274336261302));
#44791=CARTESIAN_POINT('Ctrl Pts',(0.0092000074604701,-0.041527830927245,
-0.00382672158200887));
#44792=CARTESIAN_POINT('Ctrl Pts',(0.00920000481386584,-0.0414081805923563,
-0.00374633773382311));
#44793=CARTESIAN_POINT('Ctrl Pts',(0.00920000311952209,-0.0411993385669745,
-0.00366927823060111));
#44794=CARTESIAN_POINT('Ctrl Pts',(0.00920000322260642,-0.0410527962950976,
-0.0036567880655664));
#44795=CARTESIAN_POINT('Ctrl Pts',(0.00920000289980454,-0.0409788503201197,
-0.00366042730492667));
#44796=CARTESIAN_POINT('Ctrl Pts',(0.00919999999781715,-0.0415091242546894,
-0.00394555014548031));
#44797=CARTESIAN_POINT('Ctrl Pts',(0.0091999999981165,-0.0414628494275772,
-0.00389926713241869));
#44798=CARTESIAN_POINT('Ctrl Pts',(0.00919999999878466,-0.0413581243643992,
-0.00381889960619159));
#44799=CARTESIAN_POINT('Ctrl Pts',(0.00919999999921242,-0.041175178948727,
-0.00374311636262439));
#44800=CARTESIAN_POINT('Ctrl Pts',(0.0091999999991864,-0.0410443012976303,
-0.0037258852675939));
#44801=CARTESIAN_POINT('Ctrl Pts',(0.0091999999992679,-0.0409788546105534,
-0.00372588633138973));
#44802=CARTESIAN_POINT('',(0.0092,-0.041509137648424,-0.00394549002800645));
#44803=CARTESIAN_POINT('Ctrl Pts',(0.0087883689863058,-0.0420671433761781,
-0.00338748430025228));
#44804=CARTESIAN_POINT('Ctrl Pts',(0.0088594206647638,-0.0420316175369492,
-0.00342301013948126));
#44805=CARTESIAN_POINT('Ctrl Pts',(0.0089805072296069,-0.041953189958101,
-0.00350143771832943));
#44806=CARTESIAN_POINT('Ctrl Pts',(0.0091486263560274,-0.0417471111669288,
-0.00370751650950155));
#44807=CARTESIAN_POINT('Ctrl Pts',(0.00920000000001,-0.0415819353441786,
-0.00387269233225182));
#44808=CARTESIAN_POINT('Ctrl Pts',(0.00920000000001,-0.041509137648434,
-0.00394549002799644));
#44809=CARTESIAN_POINT('',(0.0092,-0.040978887648424,-0.00372585328655811));
#44810=CARTESIAN_POINT('Origin',(0.00920000000001,-0.040978887648414,-0.00447574002801644));
#44811=CARTESIAN_POINT('Origin',(0.00845000000001,-0.040978887648414,-0.00372585328654811));
#44812=CARTESIAN_POINT('Ctrl Pts',(0.00878835104911214,-0.0420671254389844,
-0.00338744842741457));
#44813=CARTESIAN_POINT('Ctrl Pts',(0.00885940640138106,-0.0420315998218488,
-0.00342297457899238));
#44814=CARTESIAN_POINT('Ctrl Pts',(0.00898049783331015,-0.0419531724139734,
-0.00350140216653905));
#44815=CARTESIAN_POINT('Ctrl Pts',(0.00914863223099464,-0.0417470802685199,
-0.00370749278418369));
#44816=CARTESIAN_POINT('Ctrl Pts',(0.00920000864619566,-0.0415818843138174,
-0.00387269281857635));
#44817=CARTESIAN_POINT('Ctrl Pts',(0.00919999999781715,-0.0415090775309502,
-0.00394550342174106));
#44818=CARTESIAN_POINT('Ctrl Pts',(0.00882388490310589,-0.0421026592929782,
-0.00345851011497631));
#44819=CARTESIAN_POINT('Ctrl Pts',(0.00888766222063861,-0.0420666936273096,
-0.003493417418071));
#44820=CARTESIAN_POINT('Ctrl Pts',(0.00899911162941954,-0.0419879275622684,
-0.00357182744506123));
#44821=CARTESIAN_POINT('Ctrl Pts',(0.00915567704755241,-0.0417853883550417,
-0.00377739156762174));
#44822=CARTESIAN_POINT('Ctrl Pts',(0.0092000074604701,-0.0416279060944215,
-0.00392679674918539));
#44823=CARTESIAN_POINT('Ctrl Pts',(0.0091999999981165,-0.0415553605440118,
-0.00399177824885322));
#44824=CARTESIAN_POINT('Ctrl Pts',(0.00888284791227548,-0.0421616223021478,
-0.00361219741287406));
#44825=CARTESIAN_POINT('Ctrl Pts',(0.00893639360036912,-0.0421258545229966,
-0.00364703287947235));
#44826=CARTESIAN_POINT('Ctrl Pts',(0.00903477035655715,-0.0420460208003526,
-0.00372932050054387));
#44827=CARTESIAN_POINT('Ctrl Pts',(0.00917140162850093,-0.0418488819443635,
-0.00393654330593559));
#44828=CARTESIAN_POINT('Ctrl Pts',(0.00920000481386584,-0.0417082899426073,
-0.00404644708407417));
#44829=CARTESIAN_POINT('Ctrl Pts',(0.00919999999878465,-0.0416357280702388,
-0.00409650331203123));
#44830=CARTESIAN_POINT('Ctrl Pts',(0.00896282356274302,-0.0422415979526153,
-0.00401620296040005));
#44831=CARTESIAN_POINT('Ctrl Pts',(0.00900862419391088,-0.0422016787024593,
-0.00404662949367235));
#44832=CARTESIAN_POINT('Ctrl Pts',(0.00909348323881464,-0.0421081666096335,
-0.00411790693352111));
#44833=CARTESIAN_POINT('Ctrl Pts',(0.00918146742562184,-0.0419224489032019,
-0.00421501405795684));
#44834=CARTESIAN_POINT('Ctrl Pts',(0.00920000311952209,-0.0417853494458292,
-0.00425528910945596));
#44835=CARTESIAN_POINT('Ctrl Pts',(0.00919999999921242,-0.041711511313806,
-0.00427944872770334));
#44836=CARTESIAN_POINT('Ctrl Pts',(0.00898033303268561,-0.0422591074225579,
-0.00433021065651873));
#44837=CARTESIAN_POINT('Ctrl Pts',(0.00902404159839969,-0.0422153978669277,
-0.00433829479755288));
#44838=CARTESIAN_POINT('Ctrl Pts',(0.00910239830743949,-0.0421153793218916,
-0.00435590533249531));
#44839=CARTESIAN_POINT('Ctrl Pts',(0.00918085466954842,-0.0419335087707158,
-0.00438428323660133));
#44840=CARTESIAN_POINT('Ctrl Pts',(0.00920000322260641,-0.041797839610864,
-0.00440183138133278));
#44841=CARTESIAN_POINT('Ctrl Pts',(0.0091999999991864,-0.0417287424088365,
-0.00441032637880008));
#44842=CARTESIAN_POINT('Ctrl Pts',(0.00898033008514593,-0.0422591044750182,
-0.00447581353015895));
#44843=CARTESIAN_POINT('Ctrl Pts',(0.00902661141419034,-0.0422128231462237,
-0.00447580944691406));
#44844=CARTESIAN_POINT('Ctrl Pts',(0.00910698282803332,-0.0421080797083307,
-0.00447580055173983));
#44845=CARTESIAN_POINT('Ctrl Pts',(0.00918277256369609,-0.0419251032923432,
-0.00447578621866474));
#44846=CARTESIAN_POINT('Ctrl Pts',(0.00920000289980454,-0.0417942003715037,
-0.00447577735631073));
#44847=CARTESIAN_POINT('Ctrl Pts',(0.0091999999992679,-0.0417287413450407,
-0.00447577306587704));
#44848=CARTESIAN_POINT('',(0.0089803300858899,-0.0422591044757622,-0.00447574002800645));
#44849=CARTESIAN_POINT('Ctrl Pts',(0.0087883689863058,-0.0420671433761781,
-0.00338748430025228));
#44850=CARTESIAN_POINT('Ctrl Pts',(0.0088238948255348,-0.0421026692154071,
-0.00345853597871023));
#44851=CARTESIAN_POINT('Ctrl Pts',(0.0088828523983345,-0.0421616267882069,
-0.00361222007462022));
#44852=CARTESIAN_POINT('Ctrl Pts',(0.008962819076704,-0.0422415934665763,
-0.00401618029863389));
#44853=CARTESIAN_POINT('Ctrl Pts',(0.0089803300858999,-0.0422591044757722,
-0.00433015781475808));
#44854=CARTESIAN_POINT('Ctrl Pts',(0.0089803300858999,-0.0422591044757722,
-0.00447574002801644));
#44855=CARTESIAN_POINT('',(0.0092,-0.0417287743898723,-0.00447574002800645));
#44856=CARTESIAN_POINT('Origin',(0.00845000000001,-0.0417287743898823,-0.00447574002801644));
#44857=CARTESIAN_POINT('Origin',(0.00920000000001,-0.040978887648414,-0.00447574002801644));
#44858=CARTESIAN_POINT('Ctrl Pts',(0.00878835104911207,-0.0420671254389844,
-0.00338744842741442));
#44859=CARTESIAN_POINT('Ctrl Pts',(0.00882388490310585,-0.0421026592929781,
-0.00345851011497621));
#44860=CARTESIAN_POINT('Ctrl Pts',(0.00888284791227546,-0.0421616223021478,
-0.00361219741287397));
#44861=CARTESIAN_POINT('Ctrl Pts',(0.00896282356274304,-0.0422415979526153,
-0.00401620296040014));
#44862=CARTESIAN_POINT('Ctrl Pts',(0.00898033303268563,-0.0422591074225579,
-0.00433021065651894));
#44863=CARTESIAN_POINT('Ctrl Pts',(0.00898033008514593,-0.0422591044750182,
-0.00447581353015925));
#44864=CARTESIAN_POINT('Ctrl Pts',(0.00875282543197647,-0.0421381807912533,
-0.00342297457899223));
#44865=CARTESIAN_POINT('Ctrl Pts',(0.00878791923743725,-0.0421664366105109,
-0.00349341741807089));
#44866=CARTESIAN_POINT('Ctrl Pts',(0.00884708013312432,-0.0422151679902414,
-0.00364703287947226));
#44867=CARTESIAN_POINT('Ctrl Pts',(0.00892290431258698,-0.0422873985837832,
-0.00404662949367244));
#44868=CARTESIAN_POINT('Ctrl Pts',(0.00893662347705534,-0.042302815988272,
-0.00433829479755307));
#44869=CARTESIAN_POINT('Ctrl Pts',(0.00893404875635143,-0.0423053858040627,
-0.00447580944691434));
#44870=CARTESIAN_POINT('Ctrl Pts',(0.00867439802410098,-0.0422592722231824,
-0.00350140216653891));
#44871=CARTESIAN_POINT('Ctrl Pts',(0.00870915317239614,-0.0422778860192918,
-0.00357182744506112));
#44872=CARTESIAN_POINT('Ctrl Pts',(0.00876724641048024,-0.0423135447464296,
-0.00372932050054379));
#44873=CARTESIAN_POINT('Ctrl Pts',(0.00882939221976126,-0.042372257628687,
-0.00411790693352119));
#44874=CARTESIAN_POINT('Ctrl Pts',(0.00883660493201919,-0.0423811726973118,
-0.00435590533249547));
#44875=CARTESIAN_POINT('Ctrl Pts',(0.00882930531845843,-0.0423857572179057,
-0.00447580055174007));
#44876=CARTESIAN_POINT('Ctrl Pts',(0.00846830587865057,-0.0424274066208644,
-0.00370749278418045));
#44877=CARTESIAN_POINT('Ctrl Pts',(0.00850661396517241,-0.0424344514374222,
-0.00377739156761855));
#44878=CARTESIAN_POINT('Ctrl Pts',(0.00857010755449421,-0.0424501760183713,
-0.00393654330593241));
#44879=CARTESIAN_POINT('Ctrl Pts',(0.00864367451333238,-0.0424602418154928,
-0.00421501405795545));
#44880=CARTESIAN_POINT('Ctrl Pts',(0.00865473438084623,-0.0424596290594195,
-0.00438428323660103));
#44881=CARTESIAN_POINT('Ctrl Pts',(0.00864632890247365,-0.0424615469535673,
-0.00447578621866493));
#44882=CARTESIAN_POINT('Ctrl Pts',(0.00830310992395244,-0.0424787830360656,
-0.00387269281856879));
#44883=CARTESIAN_POINT('Ctrl Pts',(0.00834913170455626,-0.0424787818503404,
-0.00392679674917857));
#44884=CARTESIAN_POINT('Ctrl Pts',(0.00842951555274136,-0.0424787792037368,
-0.00404644708406916));
#44885=CARTESIAN_POINT('Ctrl Pts',(0.00850657505596322,-0.0424787775093936,
-0.0042552891094542));
#44886=CARTESIAN_POINT('Ctrl Pts',(0.00851906522099781,-0.0424787776124778,
-0.00440183138133209));
#44887=CARTESIAN_POINT('Ctrl Pts',(0.00851542598163734,-0.0424787772896761,
-0.00447577735631089));
#44888=CARTESIAN_POINT('Ctrl Pts',(0.00823030314108758,-0.0424787743876895,
-0.00394550342173112));
#44889=CARTESIAN_POINT('Ctrl Pts',(0.0082765861541492,-0.0424787743879888,
-0.00399177824884436));
#44890=CARTESIAN_POINT('Ctrl Pts',(0.00835695368037631,-0.042478774388657,
-0.00409650331202441));
#44891=CARTESIAN_POINT('Ctrl Pts',(0.00843273692394367,-0.0424787743890847,
-0.00427944872770011));
#44892=CARTESIAN_POINT('Ctrl Pts',(0.00844996801897356,-0.0424787743890587,
-0.00441032637879902));
#44893=CARTESIAN_POINT('Ctrl Pts',(0.00844996695517722,-0.0424787743891402,
-0.00447577306587717));
#44894=CARTESIAN_POINT('',(0.0082303632585517,-0.0424787743898723,-0.00394549002800645));
#44895=CARTESIAN_POINT('Ctrl Pts',(0.0087883689863058,-0.0420671433761781,
-0.00338748430025228));
#44896=CARTESIAN_POINT('Ctrl Pts',(0.0087528431470769,-0.0421381950546361,
-0.00342301013948126));
#44897=CARTESIAN_POINT('Ctrl Pts',(0.0086744155682287,-0.0422592816194792,
-0.00350143771832943));
#44898=CARTESIAN_POINT('Ctrl Pts',(0.0084683367770566,-0.0424274007458997,
-0.00370751650950155));
#44899=CARTESIAN_POINT('Ctrl Pts',(0.0083031609543063,-0.0424787743898823,
-0.00387269233225182));
#44900=CARTESIAN_POINT('Ctrl Pts',(0.0082303632585617,-0.0424787743898823,
-0.00394549002799644));
#44901=CARTESIAN_POINT('',(0.00845,-0.0424787743898723,-0.00447574002800645));
#44902=CARTESIAN_POINT('Origin',(0.0077001132585617,-0.0424787743898823,
-0.00447574002801644));
#44903=CARTESIAN_POINT('Origin',(0.00845000000001,-0.0417287743898823,-0.00447574002801644));
#44904=CARTESIAN_POINT('Ctrl Pts',(-0.0157883510491121,-0.042067179249016,
-0.0209642043356702));
#44905=CARTESIAN_POINT('Ctrl Pts',(-0.0158238849031058,-0.0419961175614543,
-0.0209997381896639));
#44906=CARTESIAN_POINT('Ctrl Pts',(-0.0158828479122755,-0.0418424302635564,
-0.0210587011988336));
#44907=CARTESIAN_POINT('Ctrl Pts',(-0.0159628235627429,-0.0414384247160302,
-0.0211386768493011));
#44908=CARTESIAN_POINT('Ctrl Pts',(-0.0159803330326856,-0.0411244170199114,
-0.0211561863192437));
#44909=CARTESIAN_POINT('Ctrl Pts',(-0.0159803300851459,-0.0409788141462712,
-0.021156183371704));
#44910=CARTESIAN_POINT('Ctrl Pts',(-0.015859406401381,-0.0420316530974383,
-0.0209286787185346));
#44911=CARTESIAN_POINT('Ctrl Pts',(-0.0158876622206386,-0.0419612102583595,
-0.0209637725239953));
#44912=CARTESIAN_POINT('Ctrl Pts',(-0.0159363936003691,-0.0418075947969582,
-0.0210229334196824));
#44913=CARTESIAN_POINT('Ctrl Pts',(-0.0160086241939108,-0.041407998182758,
-0.0210987575991451));
#44914=CARTESIAN_POINT('Ctrl Pts',(-0.0160240415983997,-0.0411163328788773,
-0.0211124767636134));
#44915=CARTESIAN_POINT('Ctrl Pts',(-0.0160266114141903,-0.0409788182295161,
-0.0211099020429095));
#44916=CARTESIAN_POINT('Ctrl Pts',(-0.0159804978333101,-0.0419532255098915,
-0.0208502513106591));
#44917=CARTESIAN_POINT('Ctrl Pts',(-0.0159991116294195,-0.0418828002313693,
-0.0208850064589542));
#44918=CARTESIAN_POINT('Ctrl Pts',(-0.0160347703565571,-0.0417253071758866,
-0.0209430996970383));
#44919=CARTESIAN_POINT('Ctrl Pts',(-0.0160934832388147,-0.0413367207429092,
-0.0210052455063193));
#44920=CARTESIAN_POINT('Ctrl Pts',(-0.0161023983074396,-0.0410987223439349,
-0.0210124582185773));
#44921=CARTESIAN_POINT('Ctrl Pts',(-0.0161069828280333,-0.0409788271246903,
-0.0210051586050165));
#44922=CARTESIAN_POINT('Ctrl Pts',(-0.0161486322309921,-0.04174713489225,
-0.0206441591652087));
#44923=CARTESIAN_POINT('Ctrl Pts',(-0.0161556770475501,-0.0416772361088118,
-0.0206824672517305));
#44924=CARTESIAN_POINT('Ctrl Pts',(-0.0161714016284989,-0.041518084370498,
-0.0207459608410522));
#44925=CARTESIAN_POINT('Ctrl Pts',(-0.0161814674256205,-0.0412396136184749,
-0.0208195277998905));
#44926=CARTESIAN_POINT('Ctrl Pts',(-0.0161808546695472,-0.0410703444398294,
-0.0208305876674043));
#44927=CARTESIAN_POINT('Ctrl Pts',(-0.016182772563695,-0.0409788414577655,
-0.0208221821890317));
#44928=CARTESIAN_POINT('Ctrl Pts',(-0.0162000086461933,-0.0415819348578615,
-0.0204789632105105));
#44929=CARTESIAN_POINT('Ctrl Pts',(-0.0162000074604681,-0.0415278309272518,
-0.0205249849911143));
#44930=CARTESIAN_POINT('Ctrl Pts',(-0.0162000048138646,-0.0414081805923612,
-0.0206053688392993));
#44931=CARTESIAN_POINT('Ctrl Pts',(-0.0162000031195212,-0.0411993385669761,
-0.0206824283425213));
#44932=CARTESIAN_POINT('Ctrl Pts',(-0.0162000032226055,-0.0410527962950982,
-0.0206949185075559));
#44933=CARTESIAN_POINT('Ctrl Pts',(-0.0162000028998038,-0.0409788503201196,
-0.0206912792681954));
#44934=CARTESIAN_POINT('Ctrl Pts',(-0.0161999999978171,-0.0415091242546993,
-0.0204061564276456));
#44935=CARTESIAN_POINT('Ctrl Pts',(-0.0161999999981165,-0.0414628494275861,
-0.0204524394407073));
#44936=CARTESIAN_POINT('Ctrl Pts',(-0.0161999999987847,-0.041358124364406,
-0.0205328069669344));
#44937=CARTESIAN_POINT('Ctrl Pts',(-0.0161999999992124,-0.0411751789487302,
-0.0206085902105018));
#44938=CARTESIAN_POINT('Ctrl Pts',(-0.0161999999991864,-0.0410443012976313,
-0.0206258213055316));
#44939=CARTESIAN_POINT('Ctrl Pts',(-0.0161999999992679,-0.0409788546105533,
-0.0206258202417353));
#44940=CARTESIAN_POINT('',(-0.0157883689862958,-0.0420671433761681,-0.0209642222728539));
#44941=CARTESIAN_POINT('',(-0.0159803300858899,-0.040978887648424,-0.021156183372448));
#44942=CARTESIAN_POINT('Ctrl Pts',(-0.0157883689863059,-0.0420671433761781,
-0.0209642222728639));
#44943=CARTESIAN_POINT('Ctrl Pts',(-0.0158238948255348,-0.0419960916977202,
-0.0209997481120929));
#44944=CARTESIAN_POINT('Ctrl Pts',(-0.0158828523983345,-0.0418424076018101,
-0.0210587056848926));
#44945=CARTESIAN_POINT('Ctrl Pts',(-0.0159628190767039,-0.0414384473777965,
-0.0211386723632621));
#44946=CARTESIAN_POINT('Ctrl Pts',(-0.0159803300858999,-0.0411244698616723,
-0.021156183372458));
#44947=CARTESIAN_POINT('Ctrl Pts',(-0.0159803300858999,-0.040978887648414,
-0.021156183372458));
#44948=CARTESIAN_POINT('',(-0.0162,-0.041509137648424,-0.0204062165451098));
#44949=CARTESIAN_POINT('Ctrl Pts',(-0.0157883689863059,-0.0420671433761781,
-0.0209642222728639));
#44950=CARTESIAN_POINT('Ctrl Pts',(-0.0158594206647638,-0.0420316175369492,
-0.020928696433635));
#44951=CARTESIAN_POINT('Ctrl Pts',(-0.0159805072296069,-0.0419531899581009,
-0.0208502688547868));
#44952=CARTESIAN_POINT('Ctrl Pts',(-0.0161486263560273,-0.0417471111669288,
-0.0206441900636147));
#44953=CARTESIAN_POINT('Ctrl Pts',(-0.01620000000001,-0.0415819353441786,
-0.0204790142408644));
#44954=CARTESIAN_POINT('Ctrl Pts',(-0.01620000000001,-0.041509137648434,
-0.0204062165451198));
#44955=CARTESIAN_POINT('',(-0.0162,-0.040978887648424,-0.0206258532865581));
#44956=CARTESIAN_POINT('Origin',(-0.01620000000001,-0.040978887648414,-0.0198759665451198));
#44957=CARTESIAN_POINT('Origin',(-0.01545000000001,-0.040978887648414,-0.0206258532865681));
#44958=CARTESIAN_POINT('Ctrl Pts',(-0.0157883510491115,-0.0420671254389838,
-0.0209642581457029));
#44959=CARTESIAN_POINT('Ctrl Pts',(-0.0158594064013806,-0.0420315998218482,
-0.0209287319941251));
#44960=CARTESIAN_POINT('Ctrl Pts',(-0.0159804978333098,-0.0419531724139726,
-0.0208503044065784));
#44961=CARTESIAN_POINT('Ctrl Pts',(-0.0161486322309936,-0.0417470802685202,
-0.0206442137889348));
#44962=CARTESIAN_POINT('Ctrl Pts',(-0.0162000086461949,-0.041581884313819,
-0.0204790137545434));
#44963=CARTESIAN_POINT('Ctrl Pts',(-0.0161999999978171,-0.0415090775309527,
-0.0204062031513794));
#44964=CARTESIAN_POINT('Ctrl Pts',(-0.0158238849031055,-0.0421026592929779,
-0.0208931964581408));
#44965=CARTESIAN_POINT('Ctrl Pts',(-0.0158876622206383,-0.0420666936273093,
-0.0208582891550461));
#44966=CARTESIAN_POINT('Ctrl Pts',(-0.0159991116294193,-0.041987927562268,
-0.0207798791280559));
#44967=CARTESIAN_POINT('Ctrl Pts',(-0.0161556770475515,-0.0417853883550424,
-0.0205743150054964));
#44968=CARTESIAN_POINT('Ctrl Pts',(-0.0162000074604694,-0.0416279060944235,
-0.0204249098239339));
#44969=CARTESIAN_POINT('Ctrl Pts',(-0.0161999999981165,-0.0415553605440146,
-0.0203599283242667));
#44970=CARTESIAN_POINT('Ctrl Pts',(-0.0158828479122753,-0.0421616223021476,
-0.020739509160243));
#44971=CARTESIAN_POINT('Ctrl Pts',(-0.015936393600369,-0.0421258545229965,
-0.0207046736936446));
#44972=CARTESIAN_POINT('Ctrl Pts',(-0.016034770356557,-0.0420460208003524,
-0.0206223860725731));
#44973=CARTESIAN_POINT('Ctrl Pts',(-0.0161714016285002,-0.0418488819443643,
-0.0204151632671822));
#44974=CARTESIAN_POINT('Ctrl Pts',(-0.0162000048138654,-0.0417082899426093,
-0.0203052594890441));
#44975=CARTESIAN_POINT('Ctrl Pts',(-0.0161999999987847,-0.041635728070242,
-0.0202552032610877));
#44976=CARTESIAN_POINT('Ctrl Pts',(-0.0159628235627431,-0.0422415979526155,
-0.0203355036127153));
#44977=CARTESIAN_POINT('Ctrl Pts',(-0.0160086241939109,-0.0422016787024594,
-0.0203050770794431));
#44978=CARTESIAN_POINT('Ctrl Pts',(-0.0160934832388148,-0.0421081666096336,
-0.0202337996395943));
#44979=CARTESIAN_POINT('Ctrl Pts',(-0.0161814674256214,-0.041922448903203,
-0.0201366925151593));
#44980=CARTESIAN_POINT('Ctrl Pts',(-0.0162000031195218,-0.0417853494458315,
-0.0200964174636605));
#44981=CARTESIAN_POINT('Ctrl Pts',(-0.0161999999992124,-0.0417115113138095,
-0.0200722578454137));
#44982=CARTESIAN_POINT('Ctrl Pts',(-0.0159803330326857,-0.042259107422558,
-0.0200214959165956));
#44983=CARTESIAN_POINT('Ctrl Pts',(-0.0160240415983998,-0.0422153978669277,
-0.0200134117755617));
#44984=CARTESIAN_POINT('Ctrl Pts',(-0.0161023983074396,-0.0421153793218915,
-0.0199958012406195));
#44985=CARTESIAN_POINT('Ctrl Pts',(-0.016180854669548,-0.0419335087707168,
-0.019967423336514));
#44986=CARTESIAN_POINT('Ctrl Pts',(-0.0162000032226061,-0.0417978396108662,
-0.0199498751917828));
#44987=CARTESIAN_POINT('Ctrl Pts',(-0.0161999999991864,-0.0417287424088398,
-0.0199413801943158));
#44988=CARTESIAN_POINT('Ctrl Pts',(-0.0159803300851459,-0.0422591044750182,
-0.0198758930429547));
#44989=CARTESIAN_POINT('Ctrl Pts',(-0.0160266114141904,-0.0422128231462237,
-0.0198758971261998));
#44990=CARTESIAN_POINT('Ctrl Pts',(-0.0161069828280334,-0.0421080797083306,
-0.0198759060213743));
#44991=CARTESIAN_POINT('Ctrl Pts',(-0.0161827725636957,-0.041925103292344,
-0.0198759203544499));
#44992=CARTESIAN_POINT('Ctrl Pts',(-0.0162000028998043,-0.0417942003715057,
-0.0198759292168042));
#44993=CARTESIAN_POINT('Ctrl Pts',(-0.0161999999992679,-0.0417287413450437,
-0.0198759335072381));
#44994=CARTESIAN_POINT('',(-0.0159803300858899,-0.0422591044757622,-0.0198759665451098));
#44995=CARTESIAN_POINT('Ctrl Pts',(-0.0157883689863059,-0.0420671433761781,
-0.0209642222728639));
#44996=CARTESIAN_POINT('Ctrl Pts',(-0.0158238948255348,-0.0421026692154071,
-0.020893170594406));
#44997=CARTESIAN_POINT('Ctrl Pts',(-0.0158828523983345,-0.0421616267882068,
-0.020739486498496));
#44998=CARTESIAN_POINT('Ctrl Pts',(-0.0159628190767039,-0.0422415934665763,
-0.0203355262744823));
#44999=CARTESIAN_POINT('Ctrl Pts',(-0.0159803300858999,-0.0422591044757722,
-0.0200215487583781));
#45000=CARTESIAN_POINT('Ctrl Pts',(-0.0159803300858999,-0.0422591044757722,
-0.0198759665451198));
#45001=CARTESIAN_POINT('',(-0.0162,-0.0417287743898723,-0.0198759665451098));
#45002=CARTESIAN_POINT('Origin',(-0.01545000000001,-0.0417287743898823,
-0.0198759665451198));
#45003=CARTESIAN_POINT('Origin',(-0.01620000000001,-0.040978887648414,-0.0198759665451198));
#45004=CARTESIAN_POINT('Ctrl Pts',(-0.0157883510491115,-0.0420671254389838,
-0.0209642581457028));
#45005=CARTESIAN_POINT('Ctrl Pts',(-0.0158238849031055,-0.0421026592929779,
-0.0208931964581408));
#45006=CARTESIAN_POINT('Ctrl Pts',(-0.0158828479122753,-0.0421616223021476,
-0.0207395091602429));
#45007=CARTESIAN_POINT('Ctrl Pts',(-0.0159628235627431,-0.0422415979526155,
-0.0203355036127154));
#45008=CARTESIAN_POINT('Ctrl Pts',(-0.0159803330326857,-0.042259107422558,
-0.0200214959165957));
#45009=CARTESIAN_POINT('Ctrl Pts',(-0.0159803300851459,-0.0422591044750182,
-0.0198758930429548));
#45010=CARTESIAN_POINT('Ctrl Pts',(-0.0157528254319759,-0.0421381807912529,
-0.0209287319941251));
#45011=CARTESIAN_POINT('Ctrl Pts',(-0.0157879192374369,-0.0421664366105106,
-0.0208582891550461));
#45012=CARTESIAN_POINT('Ctrl Pts',(-0.0158470801331242,-0.0422151679902413,
-0.0207046736936446));
#45013=CARTESIAN_POINT('Ctrl Pts',(-0.0159229043125871,-0.0422873985837833,
-0.0203050770794431));
#45014=CARTESIAN_POINT('Ctrl Pts',(-0.0159366234770554,-0.0423028159882721,
-0.0200134117755617));
#45015=CARTESIAN_POINT('Ctrl Pts',(-0.0159340487563514,-0.0423053858040627,
-0.0198758971261998));
#45016=CARTESIAN_POINT('Ctrl Pts',(-0.0156743980241005,-0.0422592722231821,
-0.0208503044065784));
#45017=CARTESIAN_POINT('Ctrl Pts',(-0.0157091531723958,-0.0422778860192916,
-0.0207798791280559));
#45018=CARTESIAN_POINT('Ctrl Pts',(-0.0157672464104802,-0.0423135447464294,
-0.0206223860725731));
#45019=CARTESIAN_POINT('Ctrl Pts',(-0.0158293922197613,-0.042372257628687,
-0.0202337996395943));
#45020=CARTESIAN_POINT('Ctrl Pts',(-0.0158366049320192,-0.0423811726973118,
-0.0199958012406195));
#45021=CARTESIAN_POINT('Ctrl Pts',(-0.0158293053184583,-0.0423857572179058,
-0.0198759060213744));
#45022=CARTESIAN_POINT('Ctrl Pts',(-0.015468305878648,-0.042427406620866,
-0.0206442137889348));
#45023=CARTESIAN_POINT('Ctrl Pts',(-0.0155066139651701,-0.0424344514374237,
-0.0205743150054965));
#45024=CARTESIAN_POINT('Ctrl Pts',(-0.0155701075544921,-0.0424501760183725,
-0.0204151632671822));
#45025=CARTESIAN_POINT('Ctrl Pts',(-0.0156436745133307,-0.0424602418154937,
-0.0201366925151594));
#45026=CARTESIAN_POINT('Ctrl Pts',(-0.0156547343808444,-0.0424596290594203,
-0.019967423336514));
#45027=CARTESIAN_POINT('Ctrl Pts',(-0.0156463289024716,-0.042461546953568,
-0.0198759203544499));
#45028=CARTESIAN_POINT('Ctrl Pts',(-0.0153031099239469,-0.0424787830360672,
-0.0204790137545434));
#45029=CARTESIAN_POINT('Ctrl Pts',(-0.0153491317045512,-0.0424787818503417,
-0.0204249098239339));
#45030=CARTESIAN_POINT('Ctrl Pts',(-0.015429515552737,-0.0424787792037377,
-0.0203052594890441));
#45031=CARTESIAN_POINT('Ctrl Pts',(-0.0155065750559592,-0.0424787775093941,
-0.0200964174636605));
#45032=CARTESIAN_POINT('Ctrl Pts',(-0.0155190652209939,-0.0424787776124784,
-0.0199498751917829));
#45033=CARTESIAN_POINT('Ctrl Pts',(-0.0155154259816334,-0.0424787772896766,
-0.0198759292168042));
#45034=CARTESIAN_POINT('Ctrl Pts',(-0.0152303031410804,-0.0424787743876895,
-0.0204062031513794));
#45035=CARTESIAN_POINT('Ctrl Pts',(-0.0152765861541423,-0.0424787743879888,
-0.0203599283242667));
#45036=CARTESIAN_POINT('Ctrl Pts',(-0.0153569536803697,-0.042478774388657,
-0.0202552032610877));
#45037=CARTESIAN_POINT('Ctrl Pts',(-0.0154327369239373,-0.0424787743890847,
-0.0200722578454137));
#45038=CARTESIAN_POINT('Ctrl Pts',(-0.0154499680189675,-0.0424787743890587,
-0.0199413801943158));
#45039=CARTESIAN_POINT('Ctrl Pts',(-0.0154499669551714,-0.0424787743891402,
-0.0198759335072381));
#45040=CARTESIAN_POINT('',(-0.0152303632585517,-0.0424787743898723,-0.0204062165451098));
#45041=CARTESIAN_POINT('Ctrl Pts',(-0.0157883689863059,-0.0420671433761781,
-0.0209642222728639));
#45042=CARTESIAN_POINT('Ctrl Pts',(-0.0157528431470768,-0.0421381950546361,
-0.020928696433635));
#45043=CARTESIAN_POINT('Ctrl Pts',(-0.0156744155682287,-0.0422592816194792,
-0.0208502688547868));
#45044=CARTESIAN_POINT('Ctrl Pts',(-0.0154683367770566,-0.0424274007458997,
-0.0206441900636147));
#45045=CARTESIAN_POINT('Ctrl Pts',(-0.0153031609543063,-0.0424787743898823,
-0.0204790142408644));
#45046=CARTESIAN_POINT('Ctrl Pts',(-0.0152303632585616,-0.0424787743898823,
-0.0204062165451198));
#45047=CARTESIAN_POINT('',(-0.01545,-0.0424787743898723,-0.0198759665451098));
#45048=CARTESIAN_POINT('Origin',(-0.0147001132585417,-0.0424787743898823,
-0.0198759665451198));
#45049=CARTESIAN_POINT('Origin',(-0.01545000000001,-0.0417287743898823,
-0.0198759665451198));
#45050=CARTESIAN_POINT('Ctrl Pts',(-0.0157884048591437,-0.0420671254389844,
-0.0209642043356702));
#45051=CARTESIAN_POINT('Ctrl Pts',(-0.0157528787075659,-0.0421381807912533,
-0.0209286787185346));
#45052=CARTESIAN_POINT('Ctrl Pts',(-0.0156744511200192,-0.0422592722231824,
-0.0208502513106591));
#45053=CARTESIAN_POINT('Ctrl Pts',(-0.0154683605023777,-0.0424274066208644,
-0.0206441591652087));
#45054=CARTESIAN_POINT('Ctrl Pts',(-0.0153031604679893,-0.0424787830360656,
-0.0204789632105105));
#45055=CARTESIAN_POINT('Ctrl Pts',(-0.015230349864827,-0.0424787743876894,
-0.0204061564276457));
#45056=CARTESIAN_POINT('Ctrl Pts',(-0.0157173431715819,-0.0421026592929782,
-0.0209997381896639));
#45057=CARTESIAN_POINT('Ctrl Pts',(-0.0156824358684873,-0.0421664366105109,
-0.0209637725239953));
#45058=CARTESIAN_POINT('Ctrl Pts',(-0.015604025841497,-0.0422778860192918,
-0.0208850064589542));
#45059=CARTESIAN_POINT('Ctrl Pts',(-0.0153984617189395,-0.0424344514374223,
-0.0206824672517305));
#45060=CARTESIAN_POINT('Ctrl Pts',(-0.0152490565373796,-0.0424787818503404,
-0.0205249849911143));
#45061=CARTESIAN_POINT('Ctrl Pts',(-0.0151840750377138,-0.0424787743879888,
-0.0204524394407073));
#45062=CARTESIAN_POINT('Ctrl Pts',(-0.0155636558736842,-0.0421616223021478,
-0.0210587011988336));
#45063=CARTESIAN_POINT('Ctrl Pts',(-0.0155288204070858,-0.0422151679902414,
-0.0210229334196824));
#45064=CARTESIAN_POINT('Ctrl Pts',(-0.0154465327860143,-0.0423135447464295,
-0.0209430996970383));
#45065=CARTESIAN_POINT('Ctrl Pts',(-0.0152393099806257,-0.0424501760183712,
-0.0207459608410522));
#45066=CARTESIAN_POINT('Ctrl Pts',(-0.0151294062024889,-0.0424787792037368,
-0.0206053688392994));
#45067=CARTESIAN_POINT('Ctrl Pts',(-0.0150793499745336,-0.042478774388657,
-0.0205328069669344));
#45068=CARTESIAN_POINT('Ctrl Pts',(-0.0151596503261579,-0.0422415979526153,
-0.0211386768493011));
#45069=CARTESIAN_POINT('Ctrl Pts',(-0.0151292237928857,-0.0422873985837832,
-0.0210987575991451));
#45070=CARTESIAN_POINT('Ctrl Pts',(-0.0150579463530369,-0.0423722576286868,
-0.0210052455063194));
#45071=CARTESIAN_POINT('Ctrl Pts',(-0.0149608392286026,-0.0424602418154928,
-0.0208195277998905));
#45072=CARTESIAN_POINT('Ctrl Pts',(-0.0149205641771039,-0.0424787775093935,
-0.0206824283425213));
#45073=CARTESIAN_POINT('Ctrl Pts',(-0.014896404558858,-0.0424787743890847,
-0.0206085902105018));
#45074=CARTESIAN_POINT('Ctrl Pts',(-0.0148456426300391,-0.0422591074225579,
-0.0211561863192437));
#45075=CARTESIAN_POINT('Ctrl Pts',(-0.0148375584890051,-0.042302815988272,
-0.0211124767636134));
#45076=CARTESIAN_POINT('Ctrl Pts',(-0.0148199479540626,-0.0423811726973118,
-0.0210124582185773));
#45077=CARTESIAN_POINT('Ctrl Pts',(-0.0147915700499571,-0.0424596290594196,
-0.0208305876674042));
#45078=CARTESIAN_POINT('Ctrl Pts',(-0.014774021905226,-0.0424787776124778,
-0.0206949185075559));
#45079=CARTESIAN_POINT('Ctrl Pts',(-0.0147655269077591,-0.0424787743890587,
-0.0206258213055317));
#45080=CARTESIAN_POINT('Ctrl Pts',(-0.0147000397563989,-0.0422591044750182,
-0.021156183371704));
#45081=CARTESIAN_POINT('Ctrl Pts',(-0.0147000438396438,-0.0423053858040627,
-0.0211099020429095));
#45082=CARTESIAN_POINT('Ctrl Pts',(-0.0147000527348181,-0.0423857572179057,
-0.0210051586050165));
#45083=CARTESIAN_POINT('Ctrl Pts',(-0.0147000670678932,-0.0424615469535673,
-0.0208221821890316));
#45084=CARTESIAN_POINT('Ctrl Pts',(-0.0147000759302473,-0.0424787772896761,
-0.0206912792681954));
#45085=CARTESIAN_POINT('Ctrl Pts',(-0.014700080220681,-0.0424787743891402,
-0.0206258202417353));
#45086=CARTESIAN_POINT('',(-0.0147001132585517,-0.0422591044757622,-0.021156183372448));
#45087=CARTESIAN_POINT('Ctrl Pts',(-0.0157883689863059,-0.0420671433761781,
-0.0209642222728639));
#45088=CARTESIAN_POINT('Ctrl Pts',(-0.0157173173078478,-0.0421026692154071,
-0.0209997481120929));
#45089=CARTESIAN_POINT('Ctrl Pts',(-0.0155636332119379,-0.0421616267882068,
-0.0210587056848926));
#45090=CARTESIAN_POINT('Ctrl Pts',(-0.0151596729879242,-0.0422415934665763,
-0.0211386723632621));
#45091=CARTESIAN_POINT('Ctrl Pts',(-0.0148456954718,-0.0422591044757722,
-0.021156183372458));
#45092=CARTESIAN_POINT('Ctrl Pts',(-0.0147001132585417,-0.0422591044757722,
-0.021156183372458));
#45093=CARTESIAN_POINT('',(-0.0147001132585517,-0.0424787743898723,-0.0206258532865581));
#45094=CARTESIAN_POINT('Origin',(-0.0147001132585417,-0.0417287743898823,
-0.0206258532865681));
#45095=CARTESIAN_POINT('Origin',(-0.0147001132585417,-0.0424787743898823,
-0.0198759665451198));
#45096=CARTESIAN_POINT('Ctrl Pts',(-0.0157884048591435,-0.0420671254389844,
-0.0209642043356702));
#45097=CARTESIAN_POINT('Ctrl Pts',(-0.0157173431715818,-0.0421026592929782,
-0.020999738189664));
#45098=CARTESIAN_POINT('Ctrl Pts',(-0.0155636558736841,-0.0421616223021478,
-0.0210587011988336));
#45099=CARTESIAN_POINT('Ctrl Pts',(-0.015159650326158,-0.0422415979526153,
-0.0211386768493011));
#45100=CARTESIAN_POINT('Ctrl Pts',(-0.0148456426300393,-0.0422591074225579,
-0.0211561863192437));
#45101=CARTESIAN_POINT('Ctrl Pts',(-0.0147000397563992,-0.0422591044750182,
-0.021156183371704));
#45102=CARTESIAN_POINT('Ctrl Pts',(-0.0157528787075658,-0.0420315998218488,
-0.0210352596879392));
#45103=CARTESIAN_POINT('Ctrl Pts',(-0.0156824358684872,-0.0420666936273096,
-0.0210635155071967));
#45104=CARTESIAN_POINT('Ctrl Pts',(-0.0155288204070858,-0.0421258545229966,
-0.0211122468869272));
#45105=CARTESIAN_POINT('Ctrl Pts',(-0.0151292237928857,-0.0422016787024593,
-0.021184477480469));
#45106=CARTESIAN_POINT('Ctrl Pts',(-0.0148375584890053,-0.0422153978669276,
-0.0211998948849578));
#45107=CARTESIAN_POINT('Ctrl Pts',(-0.0147000438396441,-0.0422128231462237,
-0.0212024647007484));
#45108=CARTESIAN_POINT('Ctrl Pts',(-0.0156744511200191,-0.0419531724139732,
-0.0211563511198682));
#45109=CARTESIAN_POINT('Ctrl Pts',(-0.0156040258414969,-0.0419879275622684,
-0.0211749649159776));
#45110=CARTESIAN_POINT('Ctrl Pts',(-0.0154465327860142,-0.0420460208003526,
-0.0212106236431153));
#45111=CARTESIAN_POINT('Ctrl Pts',(-0.015057946353037,-0.0421081666096335,
-0.0212693365253727));
#45112=CARTESIAN_POINT('Ctrl Pts',(-0.0148199479540628,-0.0421153793218915,
-0.0212782515939976));
#45113=CARTESIAN_POINT('Ctrl Pts',(-0.0147000527348183,-0.0421080797083307,
-0.0212828361145914));
#45114=CARTESIAN_POINT('Ctrl Pts',(-0.0154683605023745,-0.0417470802685199,
-0.0213244855175527));
#45115=CARTESIAN_POINT('Ctrl Pts',(-0.0153984617189363,-0.0417853883550417,
-0.0213315303341105));
#45116=CARTESIAN_POINT('Ctrl Pts',(-0.0152393099806225,-0.0418488819443635,
-0.021347254915059));
#45117=CARTESIAN_POINT('Ctrl Pts',(-0.0149608392286012,-0.0419224489032019,
-0.0213573207121799));
#45118=CARTESIAN_POINT('Ctrl Pts',(-0.0147915700499568,-0.0419335087707158,
-0.0213567079561065));
#45119=CARTESIAN_POINT('Ctrl Pts',(-0.0147000670678934,-0.0419251032923431,
-0.0213586258502542));
#45120=CARTESIAN_POINT('Ctrl Pts',(-0.0153031604679818,-0.0415818843138173,
-0.0213758619327538));
#45121=CARTESIAN_POINT('Ctrl Pts',(-0.0152490565373728,-0.0416279060944215,
-0.0213758607470282));
#45122=CARTESIAN_POINT('Ctrl Pts',(-0.0151294062024839,-0.0417082899426073,
-0.021375858100424));
#45123=CARTESIAN_POINT('Ctrl Pts',(-0.0149205641771022,-0.0417853494458292,
-0.0213758564060802));
#45124=CARTESIAN_POINT('Ctrl Pts',(-0.0147740219052253,-0.041797839610864,
-0.0213758565091645));
#45125=CARTESIAN_POINT('Ctrl Pts',(-0.0147000759302474,-0.0417942003715037,
-0.0213758561863626));
#45126=CARTESIAN_POINT('Ctrl Pts',(-0.0152303498648171,-0.0415090775309501,
-0.0213758532843752));
#45127=CARTESIAN_POINT('Ctrl Pts',(-0.0151840750377049,-0.0415553605440118,
-0.0213758532846746));
#45128=CARTESIAN_POINT('Ctrl Pts',(-0.0150793499745268,-0.0416357280702388,
-0.0213758532853428));
#45129=CARTESIAN_POINT('Ctrl Pts',(-0.0148964045588548,-0.041711511313806,
-0.0213758532857705));
#45130=CARTESIAN_POINT('Ctrl Pts',(-0.014765526907758,-0.0417287424088365,
-0.0213758532857445));
#45131=CARTESIAN_POINT('Ctrl Pts',(-0.0147000802206811,-0.0417287413450406,
-0.021375853285826));
#45132=CARTESIAN_POINT('',(-0.0152303632585517,-0.041509137648424,-0.0213758532865581));
#45133=CARTESIAN_POINT('Ctrl Pts',(-0.0157883689863059,-0.0420671433761781,
-0.0209642222728639));
#45134=CARTESIAN_POINT('Ctrl Pts',(-0.0157528431470768,-0.0420316175369492,
-0.0210352739513219));
#45135=CARTESIAN_POINT('Ctrl Pts',(-0.0156744155682287,-0.0419531899581009,
-0.021156360516165));
#45136=CARTESIAN_POINT('Ctrl Pts',(-0.0154683367770566,-0.0417471111669288,
-0.0213244796425855));
#45137=CARTESIAN_POINT('Ctrl Pts',(-0.0153031609543063,-0.0415819353441785,
-0.0213758532865681));
#45138=CARTESIAN_POINT('Ctrl Pts',(-0.0152303632585616,-0.041509137648434,
-0.0213758532865681));
#45139=CARTESIAN_POINT('',(-0.0147001132585517,-0.0417287743898723,-0.0213758532865581));
#45140=CARTESIAN_POINT('Origin',(-0.0147001132585417,-0.040978887648414,
-0.0213758532865681));
#45141=CARTESIAN_POINT('Origin',(-0.0147001132585417,-0.0417287743898823,
-0.0206258532865681));
#45142=CARTESIAN_POINT('Ctrl Pts',(0.00878835104911206,-0.042067179249016,
-0.0209642043356701));
#45143=CARTESIAN_POINT('Ctrl Pts',(0.00882388490310584,-0.0419961175614543,
-0.0209997381896639));
#45144=CARTESIAN_POINT('Ctrl Pts',(0.00888284791227546,-0.0418424302635564,
-0.0210587011988336));
#45145=CARTESIAN_POINT('Ctrl Pts',(0.00896282356274304,-0.0414384247160302,
-0.0211386768493011));
#45146=CARTESIAN_POINT('Ctrl Pts',(0.00898033303268563,-0.0411244170199114,
-0.0211561863192437));
#45147=CARTESIAN_POINT('Ctrl Pts',(0.00898033008514593,-0.0409788141462712,
-0.021156183371704));
#45148=CARTESIAN_POINT('Ctrl Pts',(0.00875282543197645,-0.0420316530974382,
-0.0210352596879391));
#45149=CARTESIAN_POINT('Ctrl Pts',(0.00878791923743724,-0.0419612102583595,
-0.0210635155071967));
#45150=CARTESIAN_POINT('Ctrl Pts',(0.00884708013312432,-0.0418075947969582,
-0.0211122468869272));
#45151=CARTESIAN_POINT('Ctrl Pts',(0.00892290431258698,-0.0414079981827579,
-0.021184477480469));
#45152=CARTESIAN_POINT('Ctrl Pts',(0.00893662347705534,-0.0411163328788773,
-0.0211998948849578));
#45153=CARTESIAN_POINT('Ctrl Pts',(0.00893404875635143,-0.0409788182295161,
-0.0212024647007484));
#45154=CARTESIAN_POINT('Ctrl Pts',(0.00867439802410097,-0.0419532255098914,
-0.0211563511198682));
#45155=CARTESIAN_POINT('Ctrl Pts',(0.00870915317239613,-0.0418828002313693,
-0.0211749649159776));
#45156=CARTESIAN_POINT('Ctrl Pts',(0.00876724641048034,-0.0417253071758866,
-0.0212106236431153));
#45157=CARTESIAN_POINT('Ctrl Pts',(0.00882939221976116,-0.0413367207429092,
-0.0212693365253728));
#45158=CARTESIAN_POINT('Ctrl Pts',(0.0088366049320192,-0.0410987223439349,
-0.0212782515939976));
#45159=CARTESIAN_POINT('Ctrl Pts',(0.00882930531845842,-0.0409788271246903,
-0.0212828361145914));
#45160=CARTESIAN_POINT('Ctrl Pts',(0.00846830587865044,-0.04174713489225,
-0.0213244855175502));
#45161=CARTESIAN_POINT('Ctrl Pts',(0.00850661396517239,-0.0416772361088118,
-0.0213315303341082));
#45162=CARTESIAN_POINT('Ctrl Pts',(0.0085701075544941,-0.041518084370498,
-0.021347254915057));
#45163=CARTESIAN_POINT('Ctrl Pts',(0.00864367451333237,-0.0412396136184749,
-0.0213573207121786));
#45164=CARTESIAN_POINT('Ctrl Pts',(0.00865473438084613,-0.0410703444398294,
-0.0213567079561054));
#45165=CARTESIAN_POINT('Ctrl Pts',(0.00864632890247354,-0.0409788414577655,
-0.0213586258502531));
#45166=CARTESIAN_POINT('Ctrl Pts',(0.0083031099239524,-0.0415819348578615,
-0.0213758619327514));
#45167=CARTESIAN_POINT('Ctrl Pts',(0.00834913170455623,-0.0415278309272518,
-0.0213758607470262));
#45168=CARTESIAN_POINT('Ctrl Pts',(0.00842951555274124,-0.0414081805923612,
-0.0213758581004227));
#45169=CARTESIAN_POINT('Ctrl Pts',(0.00850657505596321,-0.0411993385669761,
-0.0213758564060794));
#45170=CARTESIAN_POINT('Ctrl Pts',(0.0085190652209978,-0.0410527962950982,
-0.0213758565091637));
#45171=CARTESIAN_POINT('Ctrl Pts',(0.00851542598163732,-0.0409788503201196,
-0.0213758561863619));
#45172=CARTESIAN_POINT('Ctrl Pts',(0.00823030314108753,-0.0415091242546993,
-0.0213758532843753));
#45173=CARTESIAN_POINT('Ctrl Pts',(0.00827658615414917,-0.0414628494275861,
-0.0213758532846746));
#45174=CARTESIAN_POINT('Ctrl Pts',(0.00835695368037628,-0.041358124364406,
-0.0213758532853428));
#45175=CARTESIAN_POINT('Ctrl Pts',(0.00843273692394364,-0.0411751789487302,
-0.0213758532857705));
#45176=CARTESIAN_POINT('Ctrl Pts',(0.00844996801897354,-0.0410443012976313,
-0.0213758532857445));
#45177=CARTESIAN_POINT('Ctrl Pts',(0.0084499669551772,-0.0409788546105533,
-0.021375853285826));
#45178=CARTESIAN_POINT('',(0.0087883689862958,-0.0420671433761681,-0.0209642222728539));
#45179=CARTESIAN_POINT('',(0.0089803300858899,-0.040978887648424,-0.021156183372448));
#45180=CARTESIAN_POINT('Ctrl Pts',(0.0087883689863058,-0.0420671433761781,
-0.0209642222728639));
#45181=CARTESIAN_POINT('Ctrl Pts',(0.0088238948255348,-0.0419960916977202,
-0.0209997481120929));
#45182=CARTESIAN_POINT('Ctrl Pts',(0.0088828523983345,-0.0418424076018101,
-0.0210587056848926));
#45183=CARTESIAN_POINT('Ctrl Pts',(0.008962819076704,-0.0414384473777965,
-0.0211386723632621));
#45184=CARTESIAN_POINT('Ctrl Pts',(0.0089803300858999,-0.0411244698616723,
-0.021156183372458));
#45185=CARTESIAN_POINT('Ctrl Pts',(0.0089803300858999,-0.040978887648414,
-0.021156183372458));
#45186=CARTESIAN_POINT('',(0.0082303632585517,-0.041509137648424,-0.0213758532865581));
#45187=CARTESIAN_POINT('Ctrl Pts',(0.0087883689863058,-0.0420671433761781,
-0.0209642222728639));
#45188=CARTESIAN_POINT('Ctrl Pts',(0.0087528431470769,-0.0420316175369492,
-0.0210352739513219));
#45189=CARTESIAN_POINT('Ctrl Pts',(0.0086744155682287,-0.0419531899581009,
-0.021156360516165));
#45190=CARTESIAN_POINT('Ctrl Pts',(0.0084683367770565,-0.0417471111669288,
-0.0213244796425855));
#45191=CARTESIAN_POINT('Ctrl Pts',(0.0083031609543063,-0.0415819353441785,
-0.0213758532865681));
#45192=CARTESIAN_POINT('Ctrl Pts',(0.0082303632585617,-0.041509137648434,
-0.0213758532865681));
#45193=CARTESIAN_POINT('',(0.00845,-0.040978887648424,-0.0213758532865581));
#45194=CARTESIAN_POINT('Origin',(0.0077001132585617,-0.040978887648414,
-0.0213758532865681));
#45195=CARTESIAN_POINT('Origin',(0.00845000000001,-0.040978887648414,-0.0206258532865681));
#45196=CARTESIAN_POINT('Ctrl Pts',(0.00878840485914476,-0.0420671254389838,
-0.0209642043356696));
#45197=CARTESIAN_POINT('Ctrl Pts',(0.00875287870756702,-0.0420315998218482,
-0.0210352596879387));
#45198=CARTESIAN_POINT('Ctrl Pts',(0.00867445112002032,-0.0419531724139726,
-0.0211563511198679));
#45199=CARTESIAN_POINT('Ctrl Pts',(0.00846836050237665,-0.0417470802685202,
-0.0213244855175518));
#45200=CARTESIAN_POINT('Ctrl Pts',(0.00830316046798527,-0.041581884313819,
-0.021375861932753));
#45201=CARTESIAN_POINT('Ctrl Pts',(0.00823034986482127,-0.0415090775309527,
-0.0213758532843752));
#45202=CARTESIAN_POINT('Ctrl Pts',(0.00871734317158273,-0.0421026592929779,
-0.0209997381896636));
#45203=CARTESIAN_POINT('Ctrl Pts',(0.00868243586848799,-0.0420666936273092,
-0.0210635155071964));
#45204=CARTESIAN_POINT('Ctrl Pts',(0.00860402584149779,-0.041987927562268,
-0.0211749649159774));
#45205=CARTESIAN_POINT('Ctrl Pts',(0.0083984617189383,-0.0417853883550424,
-0.0213315303341096));
#45206=CARTESIAN_POINT('Ctrl Pts',(0.00824905653737567,-0.0416279060944235,
-0.0213758607470275));
#45207=CARTESIAN_POINT('Ctrl Pts',(0.00818407503770855,-0.0415553605440146,
-0.0213758532846746));
#45208=CARTESIAN_POINT('Ctrl Pts',(0.00856365587368485,-0.0421616223021476,
-0.0210587011988334));
#45209=CARTESIAN_POINT('Ctrl Pts',(0.00852882040708653,-0.0421258545229965,
-0.0211122468869271));
#45210=CARTESIAN_POINT('Ctrl Pts',(0.00844653278601498,-0.0420460208003524,
-0.0212106236431152));
#45211=CARTESIAN_POINT('Ctrl Pts',(0.00823930998062413,-0.0418488819443643,
-0.0213472549150583));
#45212=CARTESIAN_POINT('Ctrl Pts',(0.008129406202486,-0.0417082899426094,
-0.0213758581004235));
#45213=CARTESIAN_POINT('Ctrl Pts',(0.0080793499745296,-0.041635728070242,
-0.0213758532853428));
#45214=CARTESIAN_POINT('Ctrl Pts',(0.00815965032615725,-0.0422415979526155,
-0.0211386768493013));
#45215=CARTESIAN_POINT('Ctrl Pts',(0.00812922379288497,-0.0422016787024594,
-0.0211844774804691));
#45216=CARTESIAN_POINT('Ctrl Pts',(0.00805794635303622,-0.0421081666096336,
-0.0212693365253729));
#45217=CARTESIAN_POINT('Ctrl Pts',(0.00796083922860117,-0.041922448903203,
-0.0213573207121794));
#45218=CARTESIAN_POINT('Ctrl Pts',(0.00792056417710239,-0.0417853494458315,
-0.0213758564060799));
#45219=CARTESIAN_POINT('Ctrl Pts',(0.00789640455885557,-0.0417115113138095,
-0.0213758532857705));
#45220=CARTESIAN_POINT('Ctrl Pts',(0.00784564263003751,-0.042259107422558,
-0.0211561863192438));
#45221=CARTESIAN_POINT('Ctrl Pts',(0.00783755848900357,-0.0422153978669277,
-0.0211998948849579));
#45222=CARTESIAN_POINT('Ctrl Pts',(0.00781994795406137,-0.0421153793218915,
-0.0212782515939977));
#45223=CARTESIAN_POINT('Ctrl Pts',(0.00779157004995592,-0.0419335087707168,
-0.0213567079561061));
#45224=CARTESIAN_POINT('Ctrl Pts',(0.00777402190522474,-0.0417978396108662,
-0.0213758565091642));
#45225=CARTESIAN_POINT('Ctrl Pts',(0.00776552690775767,-0.0417287424088398,
-0.0213758532857445));
#45226=CARTESIAN_POINT('Ctrl Pts',(0.00770003975639664,-0.0422591044750182,
-0.021156183371704));
#45227=CARTESIAN_POINT('Ctrl Pts',(0.00770004383964167,-0.0422128231462237,
-0.0212024647007485));
#45228=CARTESIAN_POINT('Ctrl Pts',(0.00770005273481621,-0.0421080797083306,
-0.0212828361145915));
#45229=CARTESIAN_POINT('Ctrl Pts',(0.0077000670678918,-0.0419251032923439,
-0.0213586258502538));
#45230=CARTESIAN_POINT('Ctrl Pts',(0.00770007593024611,-0.0417942003715057,
-0.0213758561863624));
#45231=CARTESIAN_POINT('Ctrl Pts',(0.00770008022067996,-0.0417287413450437,
-0.021375853285826));
#45232=CARTESIAN_POINT('',(0.0077001132585517,-0.0422591044757622,-0.021156183372448));
#45233=CARTESIAN_POINT('Ctrl Pts',(0.0087883689863058,-0.0420671433761781,
-0.0209642222728639));
#45234=CARTESIAN_POINT('Ctrl Pts',(0.0087173173078479,-0.0421026692154071,
-0.0209997481120929));
#45235=CARTESIAN_POINT('Ctrl Pts',(0.0085636332119379,-0.0421616267882068,
-0.0210587056848926));
#45236=CARTESIAN_POINT('Ctrl Pts',(0.0081596729879242,-0.0422415934665763,
-0.0211386723632621));
#45237=CARTESIAN_POINT('Ctrl Pts',(0.00784569547182,-0.0422591044757722,
-0.021156183372458));
#45238=CARTESIAN_POINT('Ctrl Pts',(0.0077001132585617,-0.0422591044757722,
-0.021156183372458));
#45239=CARTESIAN_POINT('',(0.0077001132585517,-0.0417287743898723,-0.0213758532865581));
#45240=CARTESIAN_POINT('Origin',(0.0077001132585617,-0.0417287743898823,
-0.0206258532865681));
#45241=CARTESIAN_POINT('Origin',(0.0077001132585617,-0.040978887648414,
-0.0213758532865681));
#45242=CARTESIAN_POINT('Ctrl Pts',(0.00878840485914491,-0.0420671254389837,
-0.0209642043356696));
#45243=CARTESIAN_POINT('Ctrl Pts',(0.00871734317158283,-0.0421026592929778,
-0.0209997381896636));
#45244=CARTESIAN_POINT('Ctrl Pts',(0.00856365587368494,-0.0421616223021476,
-0.0210587011988334));
#45245=CARTESIAN_POINT('Ctrl Pts',(0.00815965032615716,-0.0422415979526155,
-0.0211386768493013));
#45246=CARTESIAN_POINT('Ctrl Pts',(0.0078456426300373,-0.042259107422558,
-0.0211561863192438));
#45247=CARTESIAN_POINT('Ctrl Pts',(0.00770003975639635,-0.0422591044750182,
-0.021156183371704));
#45248=CARTESIAN_POINT('Ctrl Pts',(0.00875287870756717,-0.0421381807912528,
-0.0209286787185338));
#45249=CARTESIAN_POINT('Ctrl Pts',(0.00868243586848809,-0.0421664366105106,
-0.020963772523995));
#45250=CARTESIAN_POINT('Ctrl Pts',(0.00852882040708662,-0.0422151679902413,
-0.0210229334196823));
#45251=CARTESIAN_POINT('Ctrl Pts',(0.00812922379288488,-0.0422873985837833,
-0.0210987575991452));
#45252=CARTESIAN_POINT('Ctrl Pts',(0.00783755848900338,-0.0423028159882721,
-0.0211124767636135));
#45253=CARTESIAN_POINT('Ctrl Pts',(0.00770004383964139,-0.0423053858040627,
-0.0211099020429095));
#45254=CARTESIAN_POINT('Ctrl Pts',(0.00867445112002046,-0.0422592722231821,
-0.0208502513106585));
#45255=CARTESIAN_POINT('Ctrl Pts',(0.00860402584149789,-0.0422778860192916,
-0.0208850064589539));
#45256=CARTESIAN_POINT('Ctrl Pts',(0.00844653278601506,-0.0423135447464294,
-0.0209430996970382));
#45257=CARTESIAN_POINT('Ctrl Pts',(0.00805794635303614,-0.042372257628687,
-0.0210052455063195));
#45258=CARTESIAN_POINT('Ctrl Pts',(0.00781994795406121,-0.0423811726973118,
-0.0210124582185773));
#45259=CARTESIAN_POINT('Ctrl Pts',(0.00770005273481597,-0.0423857572179058,
-0.0210051586050164));
#45260=CARTESIAN_POINT('Ctrl Pts',(0.00846836050238168,-0.042427406620862,
-0.0206441591652107));
#45261=CARTESIAN_POINT('Ctrl Pts',(0.00839846171894318,-0.0424344514374201,
-0.0206824672517328));
#45262=CARTESIAN_POINT('Ctrl Pts',(0.008239309980629,-0.0424501760183693,
-0.0207459608410547));
#45263=CARTESIAN_POINT('Ctrl Pts',(0.00796083922860346,-0.0424602418154917,
-0.0208195277998931));
#45264=CARTESIAN_POINT('Ctrl Pts',(0.00779157004995647,-0.0424596290594185,
-0.0208305876674068));
#45265=CARTESIAN_POINT('Ctrl Pts',(0.00770006706789161,-0.0424615469535663,
-0.0208221821890339));
#45266=CARTESIAN_POINT('Ctrl Pts',(0.00830316046799688,-0.0424787830360636,
-0.0204789632105163));
#45267=CARTESIAN_POINT('Ctrl Pts',(0.00824905653738625,-0.0424787818503386,
-0.0205249849911202));
#45268=CARTESIAN_POINT('Ctrl Pts',(0.0081294062024937,-0.0424787792037357,
-0.0206053688393048));
#45269=CARTESIAN_POINT('Ctrl Pts',(0.00792056417710514,-0.0424787775093928,
-0.0206824283425269));
#45270=CARTESIAN_POINT('Ctrl Pts',(0.00777402190522587,-0.0424787776124771,
-0.0206949185075614));
#45271=CARTESIAN_POINT('Ctrl Pts',(0.00770007593024596,-0.0424787772896754,
-0.0206912792682006));
#45272=CARTESIAN_POINT('Ctrl Pts',(0.00823034986483657,-0.0424787743876894,
-0.0204061564276536));
#45273=CARTESIAN_POINT('Ctrl Pts',(0.00818407503772218,-0.0424787743879888,
-0.0204524394407155));
#45274=CARTESIAN_POINT('Ctrl Pts',(0.00807934997454009,-0.042478774388657,
-0.0205328069669429));
#45275=CARTESIAN_POINT('Ctrl Pts',(0.00789640455886057,-0.0424787743890847,
-0.0206085902105108));
#45276=CARTESIAN_POINT('Ctrl Pts',(0.00776552690775935,-0.0424787743890587,
-0.02062582130554));
#45277=CARTESIAN_POINT('Ctrl Pts',(0.00770008022067983,-0.0424787743891402,
-0.0206258202417431));
#45278=CARTESIAN_POINT('',(0.0082303632585517,-0.0424787743898723,-0.0204062165451098));
#45279=CARTESIAN_POINT('Ctrl Pts',(0.0087883689863058,-0.0420671433761781,
-0.0209642222728639));
#45280=CARTESIAN_POINT('Ctrl Pts',(0.0087528431470769,-0.0421381950546361,
-0.0209286964336349));
#45281=CARTESIAN_POINT('Ctrl Pts',(0.0086744155682287,-0.0422592816194792,
-0.0208502688547868));
#45282=CARTESIAN_POINT('Ctrl Pts',(0.0084683367770566,-0.0424274007458997,
-0.0206441900636147));
#45283=CARTESIAN_POINT('Ctrl Pts',(0.0083031609543063,-0.0424787743898823,
-0.0204790142408644));
#45284=CARTESIAN_POINT('Ctrl Pts',(0.0082303632585617,-0.0424787743898823,
-0.0204062165451198));
#45285=CARTESIAN_POINT('',(0.0077001132585517,-0.0424787743898723,-0.0206258532865581));
#45286=CARTESIAN_POINT('Origin',(0.0077001132585617,-0.0424787743898823,
-0.0198759665451198));
#45287=CARTESIAN_POINT('Origin',(0.0077001132585617,-0.0417287743898823,
-0.0206258532865681));
#45288=CARTESIAN_POINT('Ctrl Pts',(0.00878835104911144,-0.0420671254389837,
-0.020964258145703));
#45289=CARTESIAN_POINT('Ctrl Pts',(0.00875282543197585,-0.0421381807912528,
-0.0209287319941252));
#45290=CARTESIAN_POINT('Ctrl Pts',(0.00867439802410037,-0.0422592722231821,
-0.0208503044065786));
#45291=CARTESIAN_POINT('Ctrl Pts',(0.00846830587865264,-0.042427406620862,
-0.0206442137889398));
#45292=CARTESIAN_POINT('Ctrl Pts',(0.00830310992395822,-0.0424787830360636,
-0.020479013754555));
#45293=CARTESIAN_POINT('Ctrl Pts',(0.00823030314109548,-0.0424787743876894,
-0.0204062031513947));
#45294=CARTESIAN_POINT('Ctrl Pts',(0.0088238849031055,-0.0421026592929778,
-0.0208931964581409));
#45295=CARTESIAN_POINT('Ctrl Pts',(0.00878791923743691,-0.0421664366105106,
-0.0208582891550462));
#45296=CARTESIAN_POINT('Ctrl Pts',(0.00870915317239579,-0.0422778860192916,
-0.020779879128056));
#45297=CARTESIAN_POINT('Ctrl Pts',(0.00850661396517473,-0.0424344514374201,
-0.0205743150055014));
#45298=CARTESIAN_POINT('Ctrl Pts',(0.00834913170456207,-0.0424787818503386,
-0.0204249098239443));
#45299=CARTESIAN_POINT('Ctrl Pts',(0.00827658615415742,-0.0424787743879888,
-0.0203599283242803));
#45300=CARTESIAN_POINT('Ctrl Pts',(0.00888284791227531,-0.0421616223021476,
-0.020739509160243));
#45301=CARTESIAN_POINT('Ctrl Pts',(0.00884708013312418,-0.0422151679902413,
-0.0207046736936447));
#45302=CARTESIAN_POINT('Ctrl Pts',(0.00876724641048012,-0.0423135447464294,
-0.0206223860725732));
#45303=CARTESIAN_POINT('Ctrl Pts',(0.00857010755449659,-0.0424501760183693,
-0.0204151632671871));
#45304=CARTESIAN_POINT('Ctrl Pts',(0.00842951555274672,-0.0424787792037357,
-0.0203052594890518));
#45305=CARTESIAN_POINT('Ctrl Pts',(0.00835695368038484,-0.042478774388657,
-0.0202552032610982));
#45306=CARTESIAN_POINT('Ctrl Pts',(0.00896282356274319,-0.0422415979526155,
-0.0203355036127153));
#45307=CARTESIAN_POINT('Ctrl Pts',(0.00892290431258713,-0.0422873985837833,
-0.020305077079443));
#45308=CARTESIAN_POINT('Ctrl Pts',(0.00882939221976138,-0.042372257628687,
-0.0202337996395942));
#45309=CARTESIAN_POINT('Ctrl Pts',(0.00864367451333499,-0.0424602418154917,
-0.0201366925151615));
#45310=CARTESIAN_POINT('Ctrl Pts',(0.00850657505596884,-0.0424787775093928,
-0.0200964174636632));
#45311=CARTESIAN_POINT('Ctrl Pts',(0.00843273692395266,-0.0424787743890847,
-0.0200722578454187));
#45312=CARTESIAN_POINT('Ctrl Pts',(0.00898033303268573,-0.042259107422558,
-0.0200214959165954));
#45313=CARTESIAN_POINT('Ctrl Pts',(0.00893662347705542,-0.0423028159882721,
-0.0200134117755615));
#45314=CARTESIAN_POINT('Ctrl Pts',(0.00883660493201924,-0.0423811726973119,
-0.0199958012406193));
#45315=CARTESIAN_POINT('Ctrl Pts',(0.00865473438084872,-0.0424596290594185,
-0.0199674233365146));
#45316=CARTESIAN_POINT('Ctrl Pts',(0.0085190652210033,-0.0424787776124771,
-0.019949875191784));
#45317=CARTESIAN_POINT('Ctrl Pts',(0.00844996801898193,-0.0424787743890587,
-0.0199413801943175));
#45318=CARTESIAN_POINT('Ctrl Pts',(0.00898033008514593,-0.0422591044750182,
-0.0198758930429544));
#45319=CARTESIAN_POINT('Ctrl Pts',(0.00893404875635139,-0.0423053858040627,
-0.0198758971261995));
#45320=CARTESIAN_POINT('Ctrl Pts',(0.0088293053184583,-0.0423857572179058,
-0.0198759060213741));
#45321=CARTESIAN_POINT('Ctrl Pts',(0.00864632890247584,-0.0424615469535663,
-0.0198759203544497));
#45322=CARTESIAN_POINT('Ctrl Pts',(0.0085154259816425,-0.0424787772896754,
-0.0198759292168041));
#45323=CARTESIAN_POINT('Ctrl Pts',(0.00844996695518506,-0.0424787743891402,
-0.0198759335072379));
#45324=CARTESIAN_POINT('',(0.0089803300858899,-0.0422591044757622,-0.0198759665451098));
#45325=CARTESIAN_POINT('Ctrl Pts',(0.0087883689863058,-0.0420671433761781,
-0.0209642222728639));
#45326=CARTESIAN_POINT('Ctrl Pts',(0.0088238948255348,-0.0421026692154071,
-0.020893170594406));
#45327=CARTESIAN_POINT('Ctrl Pts',(0.0088828523983345,-0.0421616267882068,
-0.020739486498496));
#45328=CARTESIAN_POINT('Ctrl Pts',(0.008962819076704,-0.0422415934665763,
-0.0203355262744823));
#45329=CARTESIAN_POINT('Ctrl Pts',(0.0089803300858999,-0.0422591044757722,
-0.0200215487583781));
#45330=CARTESIAN_POINT('Ctrl Pts',(0.0089803300858999,-0.0422591044757722,
-0.0198759665451198));
#45331=CARTESIAN_POINT('',(0.00845,-0.0424787743898723,-0.0198759665451098));
#45332=CARTESIAN_POINT('Origin',(0.00845000000001,-0.0417287743898823,-0.0198759665451198));
#45333=CARTESIAN_POINT('Origin',(0.0077001132585617,-0.0424787743898823,
-0.0198759665451198));
#45334=CARTESIAN_POINT('Ctrl Pts',(0.00878835104911152,-0.0420671254389838,
-0.0209642581457029));
#45335=CARTESIAN_POINT('Ctrl Pts',(0.00882388490310554,-0.0421026592929778,
-0.0208931964581408));
#45336=CARTESIAN_POINT('Ctrl Pts',(0.00888284791227533,-0.0421616223021476,
-0.020739509160243));
#45337=CARTESIAN_POINT('Ctrl Pts',(0.00896282356274317,-0.0422415979526155,
-0.0203355036127153));
#45338=CARTESIAN_POINT('Ctrl Pts',(0.00898033303268572,-0.042259107422558,
-0.0200214959165956));
#45339=CARTESIAN_POINT('Ctrl Pts',(0.00898033008514593,-0.0422591044750182,
-0.0198758930429547));
#45340=CARTESIAN_POINT('Ctrl Pts',(0.00885940640138057,-0.0420315998218482,
-0.020928731994125));
#45341=CARTESIAN_POINT('Ctrl Pts',(0.00888766222063833,-0.0420666936273092,
-0.0208582891550461));
#45342=CARTESIAN_POINT('Ctrl Pts',(0.00893639360036898,-0.0421258545229965,
-0.0207046736936446));
#45343=CARTESIAN_POINT('Ctrl Pts',(0.00900862419391102,-0.0422016787024594,
-0.0203050770794431));
#45344=CARTESIAN_POINT('Ctrl Pts',(0.00902404159839978,-0.0422153978669277,
-0.0200134117755617));
#45345=CARTESIAN_POINT('Ctrl Pts',(0.00902661141419038,-0.0422128231462237,
-0.0198758971261998));
#45346=CARTESIAN_POINT('Ctrl Pts',(0.00898049783330982,-0.0419531724139727,
-0.0208503044065784));
#45347=CARTESIAN_POINT('Ctrl Pts',(0.00899911162941933,-0.041987927562268,
-0.0207798791280559));
#45348=CARTESIAN_POINT('Ctrl Pts',(0.00903477035655714,-0.0420460208003524,
-0.0206223860725731));
#45349=CARTESIAN_POINT('Ctrl Pts',(0.00909348323881476,-0.0421081666096336,
-0.0202337996395943));
#45350=CARTESIAN_POINT('Ctrl Pts',(0.00910239830743954,-0.0421153793218915,
-0.0199958012406195));
#45351=CARTESIAN_POINT('Ctrl Pts',(0.0091069828280335,-0.0421080797083306,
-0.0198759060213743));
#45352=CARTESIAN_POINT('Ctrl Pts',(0.00914863223099365,-0.0417470802685202,
-0.0206442137889348));
#45353=CARTESIAN_POINT('Ctrl Pts',(0.00915567704755152,-0.0417853883550424,
-0.0205743150054964));
#45354=CARTESIAN_POINT('Ctrl Pts',(0.00917140162850022,-0.0418488819443643,
-0.0204151632671822));
#45355=CARTESIAN_POINT('Ctrl Pts',(0.00918146742562141,-0.041922448903203,
-0.0201366925151594));
#45356=CARTESIAN_POINT('Ctrl Pts',(0.00918085466954802,-0.0419335087707168,
-0.019967423336514));
#45357=CARTESIAN_POINT('Ctrl Pts',(0.00918277256369573,-0.0419251032923439,
-0.0198759203544499));
#45358=CARTESIAN_POINT('Ctrl Pts',(0.00920000864619486,-0.041581884313819,
-0.0204790137545434));
#45359=CARTESIAN_POINT('Ctrl Pts',(0.00920000746046942,-0.0416279060944234,
-0.0204249098239339));
#45360=CARTESIAN_POINT('Ctrl Pts',(0.0092000048138654,-0.0417082899426094,
-0.0203052594890441));
#45361=CARTESIAN_POINT('Ctrl Pts',(0.0092000031195218,-0.0417853494458315,
-0.0200964174636605));
#45362=CARTESIAN_POINT('Ctrl Pts',(0.00920000322260612,-0.0417978396108662,
-0.0199498751917828));
#45363=CARTESIAN_POINT('Ctrl Pts',(0.00920000289980427,-0.0417942003715057,
-0.0198759292168042));
#45364=CARTESIAN_POINT('Ctrl Pts',(0.00919999999781715,-0.0415090775309527,
-0.0204062031513794));
#45365=CARTESIAN_POINT('Ctrl Pts',(0.0091999999981165,-0.0415553605440146,
-0.0203599283242666));
#45366=CARTESIAN_POINT('Ctrl Pts',(0.00919999999878466,-0.041635728070242,
-0.0202552032610877));
#45367=CARTESIAN_POINT('Ctrl Pts',(0.00919999999921242,-0.0417115113138095,
-0.0200722578454137));
#45368=CARTESIAN_POINT('Ctrl Pts',(0.0091999999991864,-0.0417287424088398,
-0.0199413801943158));
#45369=CARTESIAN_POINT('Ctrl Pts',(0.00919999999926789,-0.0417287413450437,
-0.0198759335072381));
#45370=CARTESIAN_POINT('',(0.0092,-0.041509137648424,-0.0204062165451098));
#45371=CARTESIAN_POINT('Ctrl Pts',(0.0087883689863058,-0.0420671433761781,
-0.0209642222728639));
#45372=CARTESIAN_POINT('Ctrl Pts',(0.0088594206647638,-0.0420316175369492,
-0.0209286964336349));
#45373=CARTESIAN_POINT('Ctrl Pts',(0.0089805072296069,-0.0419531899581009,
-0.0208502688547868));
#45374=CARTESIAN_POINT('Ctrl Pts',(0.0091486263560274,-0.0417471111669288,
-0.0206441900636146));
#45375=CARTESIAN_POINT('Ctrl Pts',(0.00920000000001,-0.0415819353441785,
-0.0204790142408644));
#45376=CARTESIAN_POINT('Ctrl Pts',(0.00920000000001,-0.041509137648434,
-0.0204062165451198));
#45377=CARTESIAN_POINT('',(0.0092,-0.0417287743898723,-0.0198759665451098));
#45378=CARTESIAN_POINT('Origin',(0.00920000000001,-0.040978887648414,-0.0198759665451198));
#45379=CARTESIAN_POINT('Origin',(0.00845000000001,-0.0417287743898823,-0.0198759665451198));
#45380=CARTESIAN_POINT('Ctrl Pts',(0.00878835104911206,-0.042067179249016,
-0.0209642043356702));
#45381=CARTESIAN_POINT('Ctrl Pts',(0.00885940640138099,-0.0420316530974383,
-0.0209286787185344));
#45382=CARTESIAN_POINT('Ctrl Pts',(0.0089804978333101,-0.0419532255098915,
-0.0208502513106591));
#45383=CARTESIAN_POINT('Ctrl Pts',(0.00914863223099209,-0.04174713489225,
-0.0206441591652086));
#45384=CARTESIAN_POINT('Ctrl Pts',(0.00920000864619334,-0.0415819348578615,
-0.0204789632105105));
#45385=CARTESIAN_POINT('Ctrl Pts',(0.00919999999781715,-0.0415091242546993,
-0.0204061564276456));
#45386=CARTESIAN_POINT('Ctrl Pts',(0.00882388490310584,-0.0419961175614543,
-0.0209997381896639));
#45387=CARTESIAN_POINT('Ctrl Pts',(0.00888766222063857,-0.0419612102583595,
-0.0209637725239953));
#45388=CARTESIAN_POINT('Ctrl Pts',(0.00899911162941951,-0.0418828002313693,
-0.0208850064589542));
#45389=CARTESIAN_POINT('Ctrl Pts',(0.00915567704755005,-0.0416772361088118,
-0.0206824672517305));
#45390=CARTESIAN_POINT('Ctrl Pts',(0.00920000746046811,-0.0415278309272518,
-0.0205249849911143));
#45391=CARTESIAN_POINT('Ctrl Pts',(0.0091999999981165,-0.0414628494275861,
-0.0204524394407073));
#45392=CARTESIAN_POINT('Ctrl Pts',(0.00888284791227546,-0.0418424302635564,
-0.0210587011988336));
#45393=CARTESIAN_POINT('Ctrl Pts',(0.00893639360036911,-0.0418075947969582,
-0.0210229334196824));
#45394=CARTESIAN_POINT('Ctrl Pts',(0.00903477035655724,-0.0417253071758866,
-0.0209430996970383));
#45395=CARTESIAN_POINT('Ctrl Pts',(0.00917140162849889,-0.041518084370498,
-0.0207459608410522));
#45396=CARTESIAN_POINT('Ctrl Pts',(0.00920000481386456,-0.0414081805923612,
-0.0206053688392993));
#45397=CARTESIAN_POINT('Ctrl Pts',(0.00919999999878466,-0.041358124364406,
-0.0205328069669344));
#45398=CARTESIAN_POINT('Ctrl Pts',(0.00896282356274304,-0.0414384247160302,
-0.0211386768493011));
#45399=CARTESIAN_POINT('Ctrl Pts',(0.0090086241939109,-0.0414079981827579,
-0.0210987575991451));
#45400=CARTESIAN_POINT('Ctrl Pts',(0.00909348323881466,-0.0413367207429092,
-0.0210052455063194));
#45401=CARTESIAN_POINT('Ctrl Pts',(0.00918146742562052,-0.0412396136184749,
-0.0208195277998905));
#45402=CARTESIAN_POINT('Ctrl Pts',(0.00920000311952126,-0.0411993385669761,
-0.0206824283425213));
#45403=CARTESIAN_POINT('Ctrl Pts',(0.00919999999921242,-0.0411751789487302,
-0.0206085902105018));
#45404=CARTESIAN_POINT('Ctrl Pts',(0.00898033303268563,-0.0411244170199114,
-0.0211561863192437));
#45405=CARTESIAN_POINT('Ctrl Pts',(0.0090240415983997,-0.0411163328788772,
-0.0211124767636134));
#45406=CARTESIAN_POINT('Ctrl Pts',(0.0091023983074395,-0.0410987223439349,
-0.0210124582185773));
#45407=CARTESIAN_POINT('Ctrl Pts',(0.00918085466954725,-0.0410703444398294,
-0.0208305876674043));
#45408=CARTESIAN_POINT('Ctrl Pts',(0.00920000322260556,-0.0410527962950982,
-0.0206949185075559));
#45409=CARTESIAN_POINT('Ctrl Pts',(0.0091999999991864,-0.0410443012976313,
-0.0206258213055316));
#45410=CARTESIAN_POINT('Ctrl Pts',(0.00898033008514593,-0.0409788141462712,
-0.021156183371704));
#45411=CARTESIAN_POINT('Ctrl Pts',(0.00902661141419035,-0.0409788182295161,
-0.0211099020429095));
#45412=CARTESIAN_POINT('Ctrl Pts',(0.00910698282803333,-0.0409788271246903,
-0.0210051586050165));
#45413=CARTESIAN_POINT('Ctrl Pts',(0.00918277256369496,-0.0409788414577655,
-0.0208221821890316));
#45414=CARTESIAN_POINT('Ctrl Pts',(0.00920000289980377,-0.0409788503201195,
-0.0206912792681954));
#45415=CARTESIAN_POINT('Ctrl Pts',(0.00919999999926789,-0.0409788546105533,
-0.0206258202417353));
#45416=CARTESIAN_POINT('',(0.0092,-0.040978887648424,-0.0206258532865581));
#45417=CARTESIAN_POINT('Origin',(0.00845000000001,-0.040978887648414,-0.0206258532865681));
#45418=CARTESIAN_POINT('Origin',(0.00920000000001,-0.040978887648414,-0.0198759665451198));
#45419=CARTESIAN_POINT('Origin',(0.00845,-0.0326537743898723,-0.0206258532865581));
#45420=CARTESIAN_POINT('',(0.00845,-0.0297787743898723,-0.0213758532865581));
#45421=CARTESIAN_POINT('',(0.0092,-0.0297787743898723,-0.0206258532865581));
#45422=CARTESIAN_POINT('Origin',(0.00845000000001,-0.0297787743898623,-0.0206258532865681));
#45423=CARTESIAN_POINT('',(0.00920000000001,-0.0326537743898623,-0.0206258532865681));
#45424=CARTESIAN_POINT('',(0.00845000000001,-0.0326537743898623,-0.0213758532865681));
#45425=CARTESIAN_POINT('Ctrl Pts',(-0.0157883510491121,-0.0420671792490158,
-0.0209642043356702));
#45426=CARTESIAN_POINT('Ctrl Pts',(-0.0157528254319765,-0.0420316530974381,
-0.0210352596879392));
#45427=CARTESIAN_POINT('Ctrl Pts',(-0.0156743980241011,-0.0419532255098913,
-0.0211563511198682));
#45428=CARTESIAN_POINT('Ctrl Pts',(-0.0154683058786475,-0.0417471348922467,
-0.0213244855175527));
#45429=CARTESIAN_POINT('Ctrl Pts',(-0.0153031099239451,-0.041581934857854,
-0.0213758619327538));
#45430=CARTESIAN_POINT('Ctrl Pts',(-0.0152303031410778,-0.0415091242546894,
-0.0213758532843753));
#45431=CARTESIAN_POINT('Ctrl Pts',(-0.0158238849031059,-0.0419961175614541,
-0.020999738189664));
#45432=CARTESIAN_POINT('Ctrl Pts',(-0.0157879192374373,-0.0419612102583594,
-0.0210635155071967));
#45433=CARTESIAN_POINT('Ctrl Pts',(-0.0157091531723962,-0.0418828002313692,
-0.0211749649159776));
#45434=CARTESIAN_POINT('Ctrl Pts',(-0.0155066139651694,-0.0416772361088086,
-0.0213315303341105));
#45435=CARTESIAN_POINT('Ctrl Pts',(-0.0153491317045492,-0.0415278309272449,
-0.0213758607470282));
#45436=CARTESIAN_POINT('Ctrl Pts',(-0.0152765861541394,-0.0414628494275772,
-0.0213758532846746));
#45437=CARTESIAN_POINT('Ctrl Pts',(-0.0158828479122755,-0.0418424302635563,
-0.0210587011988336));
#45438=CARTESIAN_POINT('Ctrl Pts',(-0.0158470801331243,-0.0418075947969581,
-0.0211122468869272));
#45439=CARTESIAN_POINT('Ctrl Pts',(-0.0157672464104804,-0.0417253071758865,
-0.0212106236431154));
#45440=CARTESIAN_POINT('Ctrl Pts',(-0.0155701075544912,-0.0415180843704948,
-0.021347254915059));
#45441=CARTESIAN_POINT('Ctrl Pts',(-0.0154295155527349,-0.0414081805923562,
-0.0213758581004239));
#45442=CARTESIAN_POINT('Ctrl Pts',(-0.0153569536803665,-0.0413581243643992,
-0.0213758532853428));
#45443=CARTESIAN_POINT('Ctrl Pts',(-0.0159628235627429,-0.0414384247160303,
-0.0211386768493011));
#45444=CARTESIAN_POINT('Ctrl Pts',(-0.015922904312587,-0.0414079981827581,
-0.021184477480469));
#45445=CARTESIAN_POINT('Ctrl Pts',(-0.0158293922197611,-0.0413367207429093,
-0.0212693365253728));
#45446=CARTESIAN_POINT('Ctrl Pts',(-0.0156436745133296,-0.0412396136184735,
-0.0213573207121799));
#45447=CARTESIAN_POINT('Ctrl Pts',(-0.0155065750559569,-0.0411993385669744,
-0.0213758564060802));
#45448=CARTESIAN_POINT('Ctrl Pts',(-0.0154327369239338,-0.041175178948727,
-0.0213758532857705));
#45449=CARTESIAN_POINT('Ctrl Pts',(-0.0159803330326856,-0.0411244170199117,
-0.0211561863192437));
#45450=CARTESIAN_POINT('Ctrl Pts',(-0.0159366234770553,-0.0411163328788775,
-0.0211998948849578));
#45451=CARTESIAN_POINT('Ctrl Pts',(-0.0158366049320192,-0.0410987223439351,
-0.0212782515939976));
#45452=CARTESIAN_POINT('Ctrl Pts',(-0.0156547343808434,-0.0410703444398291,
-0.0213567079561065));
#45453=CARTESIAN_POINT('Ctrl Pts',(-0.0155190652209917,-0.0410527962950975,
-0.0213758565091645));
#45454=CARTESIAN_POINT('Ctrl Pts',(-0.0154499680189642,-0.0410443012976302,
-0.0213758532857445));
#45455=CARTESIAN_POINT('Ctrl Pts',(-0.0159803300851459,-0.0409788141462715,
-0.021156183371704));
#45456=CARTESIAN_POINT('Ctrl Pts',(-0.0159340487563514,-0.0409788182295164,
-0.0212024647007484));
#45457=CARTESIAN_POINT('Ctrl Pts',(-0.0158293053184584,-0.0409788271246906,
-0.0212828361145914));
#45458=CARTESIAN_POINT('Ctrl Pts',(-0.0156463289024708,-0.0409788414577657,
-0.0213586258502542));
#45459=CARTESIAN_POINT('Ctrl Pts',(-0.0155154259816314,-0.0409788503201197,
-0.0213758561863626));
#45460=CARTESIAN_POINT('Ctrl Pts',(-0.0154499669551684,-0.0409788546105534,
-0.021375853285826));
#45461=CARTESIAN_POINT('',(-0.01545,-0.040978887648424,-0.0213758532865581));
#45462=CARTESIAN_POINT('Origin',(-0.01545000000001,-0.040978887648414,-0.0206258532865681));
#45463=CARTESIAN_POINT('Origin',(-0.0147001132585417,-0.040978887648414,
-0.0213758532865681));
#45464=CARTESIAN_POINT('Origin',(-0.01545,-0.0326537743898723,-0.0206258532865581));
#45465=CARTESIAN_POINT('',(-0.0162,-0.0297787743898723,-0.0206258532865581));
#45466=CARTESIAN_POINT('',(-0.01545,-0.0297787743898723,-0.0213758532865581));
#45467=CARTESIAN_POINT('Origin',(-0.01545000000001,-0.0297787743898623,
-0.0206258532865681));
#45468=CARTESIAN_POINT('',(-0.01545000000001,-0.0326537743898623,-0.0213758532865681));
#45469=CARTESIAN_POINT('',(-0.01620000000001,-0.0326537743898623,-0.0206258532865681));
#45470=CARTESIAN_POINT('Origin',(-0.00925,-0.0417287743898723,-0.0206258532865581));
#45471=CARTESIAN_POINT('',(-0.00924999999999,-0.0424787743898823,-0.0206258532865681));
#45472=CARTESIAN_POINT('',(-0.00924999999999,-0.0417287743898823,-0.0213758532865681));
#45473=CARTESIAN_POINT('Ctrl Pts',(0.00878840485914475,-0.0420671254389838,
-0.00338750223744656));
#45474=CARTESIAN_POINT('Ctrl Pts',(0.00875287870756701,-0.0421381807912529,
-0.00342302785458223));
#45475=CARTESIAN_POINT('Ctrl Pts',(0.00867445112002031,-0.0422592722231821,
-0.00350145526245769));
#45476=CARTESIAN_POINT('Ctrl Pts',(0.00846836050237674,-0.042427406620866,
-0.00370754740791023));
#45477=CARTESIAN_POINT('Ctrl Pts',(0.00830316046798524,-0.0424787830360672,
-0.00387274336261131));
#45478=CARTESIAN_POINT('Ctrl Pts',(0.00823034986482124,-0.0424787743876894,
-0.0039455501454778));
#45479=CARTESIAN_POINT('Ctrl Pts',(0.00871734317158272,-0.0421026592929779,
-0.00335196838345255));
#45480=CARTESIAN_POINT('Ctrl Pts',(0.00868243586848798,-0.0421664366105106,
-0.00338793404912117));
#45481=CARTESIAN_POINT('Ctrl Pts',(0.00860402584149778,-0.0422778860192916,
-0.00346670011416231));
#45482=CARTESIAN_POINT('Ctrl Pts',(0.00839846171893839,-0.0424344514374237,
-0.00366923932138805));
#45483=CARTESIAN_POINT('Ctrl Pts',(0.00824905653737574,-0.0424787818503417,
-0.00382672158200695));
#45484=CARTESIAN_POINT('Ctrl Pts',(0.00818407503770852,-0.0424787743879888,
-0.00389926713241585));
#45485=CARTESIAN_POINT('Ctrl Pts',(0.00856365587368484,-0.0421616223021476,
-0.00329300537428275));
#45486=CARTESIAN_POINT('Ctrl Pts',(0.00852882040708652,-0.0422151679902413,
-0.00332877315343396));
#45487=CARTESIAN_POINT('Ctrl Pts',(0.00844653278601497,-0.0423135447464294,
-0.00340860687607793));
#45488=CARTESIAN_POINT('Ctrl Pts',(0.00823930998062411,-0.0424501760183726,
-0.00360574573206604));
#45489=CARTESIAN_POINT('Ctrl Pts',(0.00812940620248598,-0.0424787792037377,
-0.00374633773382112));
#45490=CARTESIAN_POINT('Ctrl Pts',(0.00807934997452958,-0.042478774388657,
-0.00381889960618842));
#45491=CARTESIAN_POINT('Ctrl Pts',(0.00815965032615726,-0.0422415979526155,
-0.00321302972381497));
#45492=CARTESIAN_POINT('Ctrl Pts',(0.00812922379288498,-0.0422873985837833,
-0.00325294897397103));
#45493=CARTESIAN_POINT('Ctrl Pts',(0.00805794635303623,-0.0423722576286871,
-0.0033464610667968));
#45494=CARTESIAN_POINT('Ctrl Pts',(0.00796083922860117,-0.0424602418154937,
-0.00353217877322744));
#45495=CARTESIAN_POINT('Ctrl Pts',(0.00792056417710238,-0.0424787775093941,
-0.00366927823059887));
#45496=CARTESIAN_POINT('Ctrl Pts',(0.00789640455885557,-0.0424787743890847,
-0.00374311636262087));
#45497=CARTESIAN_POINT('Ctrl Pts',(0.00784564263003753,-0.042259107422558,
-0.00319552025387238));
#45498=CARTESIAN_POINT('Ctrl Pts',(0.00783755848900359,-0.0423028159882721,
-0.00323922980950267));
#45499=CARTESIAN_POINT('Ctrl Pts',(0.00781994795406138,-0.0423811726973118,
-0.00333924835453885));
#45500=CARTESIAN_POINT('Ctrl Pts',(0.00779157004995593,-0.0424596290594203,
-0.00352111890571367));
#45501=CARTESIAN_POINT('Ctrl Pts',(0.00777402190522475,-0.0424787776124784,
-0.00365678806556426));
#45502=CARTESIAN_POINT('Ctrl Pts',(0.00776552690775767,-0.0424787743890587,
-0.00372588526759064));
#45503=CARTESIAN_POINT('Ctrl Pts',(0.00770003975639667,-0.0422591044750182,
-0.00319552320141217));
#45504=CARTESIAN_POINT('Ctrl Pts',(0.00770004383964169,-0.0423053858040628,
-0.00324180453020672));
#45505=CARTESIAN_POINT('Ctrl Pts',(0.00770005273481624,-0.0423857572179058,
-0.00334654796809979));
#45506=CARTESIAN_POINT('Ctrl Pts',(0.00770006706789182,-0.042461546953568,
-0.00352952438408646));
#45507=CARTESIAN_POINT('Ctrl Pts',(0.00770007593024613,-0.0424787772896766,
-0.00366042730492475));
#45508=CARTESIAN_POINT('Ctrl Pts',(0.00770008022067997,-0.0424787743891402,
-0.00372588633138674));
#45509=CARTESIAN_POINT('',(0.0077001132585517,-0.0424787743898723,-0.00372585328655811));
#45510=CARTESIAN_POINT('Origin',(0.0077001132585617,-0.0417287743898823,
-0.00372585328654811));
#45511=CARTESIAN_POINT('Origin',(0.0077001132585617,-0.0424787743898823,
-0.00447574002801644));
#45512=CARTESIAN_POINT('Origin',(0.00845,-0.0355287743470315,-0.00372585328655811));
#45513=CARTESIAN_POINT('',(0.0092,-0.0297787743898723,-0.0037258532865581));
#45514=CARTESIAN_POINT('',(0.00845,-0.0297787743898723,-0.0029758532865581));
#45515=CARTESIAN_POINT('Origin',(0.00845000000001,-0.0297787743898623,-0.0037258532865481));
#45516=CARTESIAN_POINT('',(0.00845000000001,-0.0355287743470215,-0.0029758532865481));
#45517=CARTESIAN_POINT('',(0.00920000000001,-0.0355287743470215,-0.00372585328654811));
#45518=CARTESIAN_POINT('Ctrl Pts',(-0.0157884048591435,-0.0420671254389844,
-0.00338750223744594));
#45519=CARTESIAN_POINT('Ctrl Pts',(-0.0157528787075658,-0.0420315998218488,
-0.00331644688517705));
#45520=CARTESIAN_POINT('Ctrl Pts',(-0.0156744511200191,-0.0419531724139733,
-0.00319535545324795));
#45521=CARTESIAN_POINT('Ctrl Pts',(-0.0154683605023745,-0.0417470802685198,
-0.00302722105556351));
#45522=CARTESIAN_POINT('Ctrl Pts',(-0.0153031604679818,-0.0415818843138174,
-0.00297584464036245));
#45523=CARTESIAN_POINT('Ctrl Pts',(-0.0152303498648171,-0.0415090775309501,
-0.00297585328874096));
#45524=CARTESIAN_POINT('Ctrl Pts',(-0.0157173431715818,-0.0421026592929782,
-0.00335196838345221));
#45525=CARTESIAN_POINT('Ctrl Pts',(-0.0156824358684872,-0.0420666936273096,
-0.00328819106591947));
#45526=CARTESIAN_POINT('Ctrl Pts',(-0.0156040258414969,-0.0419879275622684,
-0.00317674165713853));
#45527=CARTESIAN_POINT('Ctrl Pts',(-0.0153984617189363,-0.0417853883550417,
-0.00302017623900573));
#45528=CARTESIAN_POINT('Ctrl Pts',(-0.0152490565373728,-0.0416279060944215,
-0.002975845826088));
#45529=CARTESIAN_POINT('Ctrl Pts',(-0.0151840750377049,-0.0415553605440117,
-0.00297585328844161));
#45530=CARTESIAN_POINT('Ctrl Pts',(-0.0155636558736841,-0.0421616223021478,
-0.0032930053742826));
#45531=CARTESIAN_POINT('Ctrl Pts',(-0.0155288204070858,-0.0421258545229966,
-0.00323945968618904));
#45532=CARTESIAN_POINT('Ctrl Pts',(-0.0154465327860142,-0.0420460208003526,
-0.00314108293000091));
#45533=CARTESIAN_POINT('Ctrl Pts',(-0.0152393099806225,-0.0418488819443635,
-0.00300445165805714));
#45534=CARTESIAN_POINT('Ctrl Pts',(-0.0151294062024839,-0.0417082899426073,
-0.00297584847269226));
#45535=CARTESIAN_POINT('Ctrl Pts',(-0.0150793499745268,-0.0416357280702388,
-0.00297585328777345));
#45536=CARTESIAN_POINT('Ctrl Pts',(-0.015159650326158,-0.0422415979526153,
-0.00321302972381513));
#45537=CARTESIAN_POINT('Ctrl Pts',(-0.0151292237928857,-0.0422016787024593,
-0.00316722909264727));
#45538=CARTESIAN_POINT('Ctrl Pts',(-0.015057946353037,-0.0421081666096335,
-0.00308237004774347));
#45539=CARTESIAN_POINT('Ctrl Pts',(-0.0149608392286012,-0.0419224489032019,
-0.00299438586093631));
#45540=CARTESIAN_POINT('Ctrl Pts',(-0.0149205641771022,-0.0417853494458292,
-0.00297585016703602));
#45541=CARTESIAN_POINT('Ctrl Pts',(-0.0148964045588548,-0.041711511313806,
-0.00297585328734569));
#45542=CARTESIAN_POINT('Ctrl Pts',(-0.0148456426300393,-0.0422591074225579,
-0.00319552025387248));
#45543=CARTESIAN_POINT('Ctrl Pts',(-0.0148375584890053,-0.0422153978669277,
-0.00315181168815843));
#45544=CARTESIAN_POINT('Ctrl Pts',(-0.0148199479540628,-0.0421153793218916,
-0.00307345497911859));
#45545=CARTESIAN_POINT('Ctrl Pts',(-0.0147915700499568,-0.0419335087707158,
-0.00299499861700968));
#45546=CARTESIAN_POINT('Ctrl Pts',(-0.0147740219052253,-0.041797839610864,
-0.00297585006395169));
#45547=CARTESIAN_POINT('Ctrl Pts',(-0.014765526907758,-0.0417287424088365,
-0.00297585328737171));
#45548=CARTESIAN_POINT('Ctrl Pts',(-0.0147000397563992,-0.0422591044750182,
-0.00319552320141217));
#45549=CARTESIAN_POINT('Ctrl Pts',(-0.0147000438396441,-0.0422128231462237,
-0.00314924187236774));
#45550=CARTESIAN_POINT('Ctrl Pts',(-0.0147000527348183,-0.0421080797083307,
-0.00306887045852474));
#45551=CARTESIAN_POINT('Ctrl Pts',(-0.0147000670678934,-0.0419251032923432,
-0.002993080722862));
#45552=CARTESIAN_POINT('Ctrl Pts',(-0.0147000759302474,-0.0417942003715037,
-0.00297585038675357));
#45553=CARTESIAN_POINT('Ctrl Pts',(-0.0147000802206811,-0.0417287413450406,
-0.00297585328729021));
#45554=CARTESIAN_POINT('',(-0.0147001132585517,-0.0417287743898723,-0.00297585328655811));
#45555=CARTESIAN_POINT('Origin',(-0.0147001132585417,-0.0417287743898823,
-0.00372585328654811));
#45556=CARTESIAN_POINT('Origin',(-0.0147001132585417,-0.040978887648414,
-0.00297585328654811));
#45557=CARTESIAN_POINT('Origin',(-0.01545,-0.0355287743470315,-0.00372585328655811));
#45558=CARTESIAN_POINT('',(-0.01545,-0.0297787743898723,-0.0029758532865581));
#45559=CARTESIAN_POINT('',(-0.0162,-0.0297787743898723,-0.0037258532865581));
#45560=CARTESIAN_POINT('Origin',(-0.01545000000001,-0.0297787743898623,
-0.0037258532865481));
#45561=CARTESIAN_POINT('',(-0.01620000000001,-0.0355287743470215,-0.00372585328654811));
#45562=CARTESIAN_POINT('',(-0.01545000000001,-0.0355287743470215,-0.0029758532865481));
#45563=CARTESIAN_POINT('Origin',(-0.01545,-0.0417287743898723,-0.0121758532865581));
#45564=CARTESIAN_POINT('',(-0.01545000000001,-0.0424787743898823,-0.0121758532865681));
#45565=CARTESIAN_POINT('',(-0.01620000000001,-0.0417287743898823,-0.0121758532865681));
#45566=CARTESIAN_POINT('Origin',(-0.0035,-0.0417287743898723,-0.00372585328655811));
#45567=CARTESIAN_POINT('',(-0.00349999999999,-0.0424787743898823,-0.00372585328654811));
#45568=CARTESIAN_POINT('',(-0.00349999999999,-0.0417287743898823,-0.00297585328654811));
#45569=CARTESIAN_POINT('Origin',(0.00845,-0.0417287743898723,-0.0121758532865581));
#45570=CARTESIAN_POINT('',(0.00845000000001,-0.0424787743898823,-0.0121758532865681));
#45571=CARTESIAN_POINT('',(0.00920000000001,-0.0417287743898823,-0.0121758532865681));
#45572=CARTESIAN_POINT('Origin',(-0.015,-0.0297787743898723,-0.0213758532865581));
#45573=CARTESIAN_POINT('',(-0.0095,-0.0297787743898723,-0.0213758532865581));
#45574=CARTESIAN_POINT('',(-0.015,-0.0297787743898623,-0.0213758532865681));
#45575=CARTESIAN_POINT('',(-0.0095,-0.0372787743898723,-0.0213758532865581));
#45576=CARTESIAN_POINT('',(-0.00949999999999,-0.0372787743898623,-0.0213758532865681));
#45577=CARTESIAN_POINT('',(-0.0035,-0.0372787743898723,-0.0213758532865581));
#45578=CARTESIAN_POINT('Origin',(-0.00649999999999,-0.0372787743898623,
-0.0213758532865681));
#45579=CARTESIAN_POINT('',(-0.0035,-0.0285787743898723,-0.0213758532865581));
#45580=CARTESIAN_POINT('',(-0.00349999999999,-0.0372787743898623,-0.0213758532865681));
#45581=CARTESIAN_POINT('',(0.0045,-0.0285787743898723,-0.0213758532865581));
#45582=CARTESIAN_POINT('',(0.00450000000001,-0.0285787743898623,-0.0213758532865681));
#45583=CARTESIAN_POINT('',(0.0045,-0.035138261906077,-0.0213758532865581));
#45584=CARTESIAN_POINT('',(0.00450000000001,-0.0297787743898623,-0.0213758532865681));
#45585=CARTESIAN_POINT('',(0.0075,-0.035138261906077,-0.0213758532865581));
#45586=CARTESIAN_POINT('Origin',(0.00600000000001,-0.0355287743898623,-0.0213758532865681));
#45587=CARTESIAN_POINT('',(0.0075,-0.0297787743898723,-0.0213758532865581));
#45588=CARTESIAN_POINT('',(0.00750000000001,-0.0355287743898623,-0.0213758532865681));
#45589=CARTESIAN_POINT('',(-0.015,-0.0297787743898623,-0.0213758532865681));
#45590=CARTESIAN_POINT('Origin',(-0.0095,-0.0297787743898723,-0.0041758532865581));
#45591=CARTESIAN_POINT('',(-0.0162,-0.0297787743898723,-0.0189258532865581));
#45592=CARTESIAN_POINT('',(-0.01620000000001,-0.0297787743898623,-0.0213758532865681));
#45593=CARTESIAN_POINT('',(-0.015,-0.0297787743898723,-0.0189258532865581));
#45594=CARTESIAN_POINT('',(-0.01119999999999,-0.0297787743898623,-0.0189258532865681));
#45595=CARTESIAN_POINT('',(-0.015,-0.0297787743898723,-0.0201758532865581));
#45596=CARTESIAN_POINT('',(-0.015,-0.0297787743898623,-0.0213758532865681));
#45597=CARTESIAN_POINT('',(-0.0095,-0.0297787743898723,-0.0201758532865581));
#45598=CARTESIAN_POINT('',(-0.00924999999999,-0.0297787743898623,-0.0201758532865681));
#45599=CARTESIAN_POINT('',(-0.00949999999999,-0.0297787743898623,-0.0029758532865481));
#45600=CARTESIAN_POINT('Origin',(-0.0162,-0.0355287743898723,-0.0121758532865581));
#45601=CARTESIAN_POINT('',(-0.0162,-0.0297787743898723,-0.0054258532865581));
#45602=CARTESIAN_POINT('',(-0.01620000000001,-0.0297787743898623,-0.0213758532865681));
#45603=CARTESIAN_POINT('',(-0.0162,-0.0285787743898723,-0.0054258532865581));
#45604=CARTESIAN_POINT('',(-0.01620000000001,-0.0297787743898623,-0.0054258532865681));
#45605=CARTESIAN_POINT('',(-0.0162,-0.0285787743898723,-0.0104258532865581));
#45606=CARTESIAN_POINT('',(-0.01620000000001,-0.0285787743898623,-0.0104258532865681));
#45607=CARTESIAN_POINT('',(-0.0162,-0.0297787743898723,-0.0104258532865581));
#45608=CARTESIAN_POINT('',(-0.01620000000001,-0.0297787743898623,-0.0104258532865681));
#45609=CARTESIAN_POINT('',(-0.0162,-0.0297787743898723,-0.0139258532865581));
#45610=CARTESIAN_POINT('',(-0.01620000000001,-0.0297787743898623,-0.0213758532865681));
#45611=CARTESIAN_POINT('',(-0.0162,-0.0285787743898723,-0.0139258532865581));
#45612=CARTESIAN_POINT('',(-0.01620000000001,-0.0297787743898623,-0.0139258532865681));
#45613=CARTESIAN_POINT('',(-0.0162,-0.0285787743898723,-0.0189258532865581));
#45614=CARTESIAN_POINT('',(-0.01620000000001,-0.0285787743898623,-0.0139258532865681));
#45615=CARTESIAN_POINT('',(-0.01620000000001,-0.0297787743898623,-0.0189258532865681));
#45616=CARTESIAN_POINT('Origin',(-0.0095,-0.0297787743898723,-0.0041758532865581));
#45617=CARTESIAN_POINT('',(-0.0095,-0.0297787743898723,-0.0029758532865581));
#45618=CARTESIAN_POINT('',(-0.015,-0.0297787743898623,-0.0029758532865481));
#45619=CARTESIAN_POINT('',(-0.0095,-0.0297787743898723,-0.0041758532865581));
#45620=CARTESIAN_POINT('',(-0.00949999999999,-0.0297787743898623,-0.0041758532865581));
#45621=CARTESIAN_POINT('',(-0.015,-0.0297787743898723,-0.0041758532865581));
#45622=CARTESIAN_POINT('',(-0.015,-0.0297787743898623,-0.0041758532865581));
#45623=CARTESIAN_POINT('',(-0.015,-0.0297787743898723,-0.0054258532865581));
#45624=CARTESIAN_POINT('',(-0.015,-0.0297787743898623,-0.0213758532865681));
#45625=CARTESIAN_POINT('',(-0.01284999999999,-0.0297787743898623,-0.0054258532865681));
#45626=CARTESIAN_POINT('Origin',(-0.0035,-0.0424787743898723,-0.0121758532865581));
#45627=CARTESIAN_POINT('',(-0.00685,-0.0424787743898823,-0.0121758532865581));
#45628=CARTESIAN_POINT('Origin',(1.00006808390063E-14,-0.0424787743898823,
-0.0121758532865681));
#45629=CARTESIAN_POINT('',(-0.015,-0.0424787743898823,-0.0121758532865581));
#45630=CARTESIAN_POINT('Origin',(-0.01249999999999,-0.0424787743898823,
-0.0121758532865681));
#45631=CARTESIAN_POINT('Origin',(-0.0139,-0.0295787743898723,-0.0066758532865581));
#45632=CARTESIAN_POINT('',(-0.0129,-0.0295787743898723,-0.0104258532865581));
#45633=CARTESIAN_POINT('',(-0.0139,-0.0285787743898723,-0.0104258532865581));
#45634=CARTESIAN_POINT('Origin',(-0.01389999999999,-0.0295787743898623,
-0.0104258532865681));
#45635=CARTESIAN_POINT('',(-0.0139,-0.0285787743898723,-0.0054258532865581));
#45636=CARTESIAN_POINT('',(-0.01389999999999,-0.0285787743898623,-0.0066758532865681));
#45637=CARTESIAN_POINT('',(-0.0129,-0.0295787743898723,-0.0054258532865581));
#45638=CARTESIAN_POINT('Origin',(-0.01389999999999,-0.0295787743898623,
-0.0054258532865681));
#45639=CARTESIAN_POINT('',(-0.01289999999999,-0.0295787743898623,-0.0066758532865681));
#45640=CARTESIAN_POINT('Origin',(-0.01455,-0.0285787743898723,-0.0079258532865581));
#45641=CARTESIAN_POINT('',(-0.01289999999999,-0.0285787743898623,-0.0104258532865681));
#45642=CARTESIAN_POINT('',(-0.01620000000001,-0.0285787743898623,-0.0054258532865681));
#45643=CARTESIAN_POINT('Origin',(-0.0129,-0.0297787743898723,-0.0104258532865581));
#45644=CARTESIAN_POINT('',(-0.0129,-0.0297787743898723,-0.0104258532865581));
#45645=CARTESIAN_POINT('',(-0.01289999999999,-0.0297787743898623,-0.0104258532865681));
#45646=CARTESIAN_POINT('',(-0.015,-0.0297787743898723,-0.0104258532865581));
#45647=CARTESIAN_POINT('',(-0.01289999999999,-0.0297787743898623,-0.0104258532865681));
#45648=CARTESIAN_POINT('',(-0.01119999999999,-0.0297787743898623,-0.0104258532865681));
#45649=CARTESIAN_POINT('Origin',(-0.0139,-0.0295787743898723,-0.0151758532865581));
#45650=CARTESIAN_POINT('',(-0.0129,-0.0295787743898723,-0.0189258532865581));
#45651=CARTESIAN_POINT('',(-0.0139,-0.0285787743898723,-0.0189258532865581));
#45652=CARTESIAN_POINT('Origin',(-0.01389999999999,-0.0295787743898623,
-0.0189258532865681));
#45653=CARTESIAN_POINT('',(-0.0139,-0.0285787743898723,-0.0139258532865581));
#45654=CARTESIAN_POINT('',(-0.01389999999999,-0.0285787743898623,-0.0151758532865681));
#45655=CARTESIAN_POINT('',(-0.0129,-0.0295787743898723,-0.0139258532865581));
#45656=CARTESIAN_POINT('Origin',(-0.01389999999999,-0.0295787743898623,
-0.0139258532865681));
#45657=CARTESIAN_POINT('',(-0.01289999999999,-0.0295787743898623,-0.0151758532865681));
#45658=CARTESIAN_POINT('Origin',(-0.01455,-0.0285787743898723,-0.0164258532865581));
#45659=CARTESIAN_POINT('',(-0.01620000000001,-0.0285787743898623,-0.0189258532865681));
#45660=CARTESIAN_POINT('',(-0.01289999999999,-0.0285787743898623,-0.0139258532865681));
#45661=CARTESIAN_POINT('Origin',(-0.0129,-0.0297787743898723,-0.0189258532865581));
#45662=CARTESIAN_POINT('',(-0.0129,-0.0297787743898723,-0.0189258532865581));
#45663=CARTESIAN_POINT('',(-0.01289999999999,-0.0297787743898623,-0.0189258532865681));
#45664=CARTESIAN_POINT('',(-0.01620000000001,-0.0297787743898623,-0.0189258532865681));
#45665=CARTESIAN_POINT('Origin',(-0.0015,-0.0295787743898723,-0.0190758532865581));
#45666=CARTESIAN_POINT('',(0.0045,-0.0295787743898723,-0.0180758532865581));
#45667=CARTESIAN_POINT('',(0.0045,-0.0285787743898723,-0.0190758532865581));
#45668=CARTESIAN_POINT('Origin',(0.00450000000001,-0.0295787743898623,-0.0190758532865681));
#45669=CARTESIAN_POINT('',(-0.0035,-0.0285787743898723,-0.0190758532865581));
#45670=CARTESIAN_POINT('',(-0.00149999999999,-0.0285787743898623,-0.0190758532865681));
#45671=CARTESIAN_POINT('',(-0.0035,-0.0295787743898723,-0.0180758532865581));
#45672=CARTESIAN_POINT('Origin',(-0.00349999999999,-0.0295787743898623,
-0.0190758532865681));
#45673=CARTESIAN_POINT('',(-0.00149999999999,-0.0295787743898623,-0.0180758532865681));
#45674=CARTESIAN_POINT('Origin',(-0.0035,-0.0372787743898723,-0.00297585328655811));
#45675=CARTESIAN_POINT('',(-0.00349999999999,-0.0285787743898623,-0.0213758532865681));
#45676=CARTESIAN_POINT('',(-0.0035,-0.0372787743898723,-0.0201758532865581));
#45677=CARTESIAN_POINT('',(-0.00349999999999,-0.0372787743898623,-0.0029758532865481));
#45678=CARTESIAN_POINT('',(-0.0035,-0.0297787743898723,-0.0201758532865581));
#45679=CARTESIAN_POINT('',(-0.00349999999999,-0.0364037743470214,-0.0201758532865681));
#45680=CARTESIAN_POINT('',(-0.0035,-0.0297787743898723,-0.0180758532865581));
#45681=CARTESIAN_POINT('',(-0.00349999999999,-0.0297787743898623,-0.0213758532865681));
#45682=CARTESIAN_POINT('',(-0.00349999999999,-0.0297787743898623,-0.0180758532865681));
#45683=CARTESIAN_POINT('Origin',(0.0005,-0.0285787743898723,-0.0197258532865581));
#45684=CARTESIAN_POINT('',(0.00450000000001,-0.0285787743898623,-0.0180758532865681));
#45685=CARTESIAN_POINT('Origin',(0.0025,-0.0295787743898723,-0.0052758532865581));
#45686=CARTESIAN_POINT('',(-0.0035,-0.0295787743898723,-0.0062758532865581));
#45687=CARTESIAN_POINT('',(-0.0035,-0.0285787743898723,-0.0052758532865581));
#45688=CARTESIAN_POINT('Origin',(-0.00349999999999,-0.0295787743898623,
-0.0052758532865681));
#45689=CARTESIAN_POINT('',(0.0045,-0.0285787743898723,-0.0052758532865581));
#45690=CARTESIAN_POINT('',(0.00250000000001,-0.0285787743898623,-0.0052758532865681));
#45691=CARTESIAN_POINT('',(0.0045,-0.0295787743898723,-0.0062758532865581));
#45692=CARTESIAN_POINT('Origin',(0.00450000000001,-0.0295787743898623,-0.0052758532865681));
#45693=CARTESIAN_POINT('',(0.00250000000001,-0.0295787743898623,-0.0062758532865681));
#45694=CARTESIAN_POINT('Origin',(0.0045,-0.035138261906077,-0.0041758532865581));
#45695=CARTESIAN_POINT('',(0.0045,-0.0285787743898723,-0.0029758532865581));
#45696=CARTESIAN_POINT('',(0.00450000000001,-0.0285787743898623,-0.0062758532865681));
#45697=CARTESIAN_POINT('',(0.0045,-0.035138261906077,-0.00297585328655811));
#45698=CARTESIAN_POINT('',(0.00450000000001,-0.0355287743898623,-0.0029758532865481));
#45699=CARTESIAN_POINT('',(0.0045,-0.035138261906077,-0.0041758532865581));
#45700=CARTESIAN_POINT('',(0.00450000000001,-0.035138261906067,-0.0041758532865581));
#45701=CARTESIAN_POINT('',(0.0045,-0.0297787743898723,-0.0041758532865581));
#45702=CARTESIAN_POINT('',(0.00450000000001,-0.0355287743898623,-0.0041758532865581));
#45703=CARTESIAN_POINT('',(0.0045,-0.0297787743898723,-0.0062758532865581));
#45704=CARTESIAN_POINT('',(0.00450000000001,-0.0297787743898623,-0.0062758532865681));
#45705=CARTESIAN_POINT('',(0.00450000000001,-0.0297787743898623,-0.0062758532865681));
#45706=CARTESIAN_POINT('Origin',(0.0005,-0.0285787743898723,-0.0046258532865581));
#45707=CARTESIAN_POINT('',(-0.0035,-0.0285787743898723,-0.0029758532865581));
#45708=CARTESIAN_POINT('',(-0.00349999999999,-0.0285787743898623,-0.00297585328654809));
#45709=CARTESIAN_POINT('',(0.00450000000001,-0.0285787743898623,-0.00297585328654809));
#45710=CARTESIAN_POINT('Origin',(0.0069,-0.0295787743898723,-0.0155508532865581));
#45711=CARTESIAN_POINT('',(0.0059,-0.0295787743898723,-0.0054258532865581));
#45712=CARTESIAN_POINT('',(0.0069,-0.0285787743898723,-0.0054258532865581));
#45713=CARTESIAN_POINT('Origin',(0.00690000000001,-0.0295787743898623,-0.0054258532865681));
#45714=CARTESIAN_POINT('',(0.0069,-0.0285787743898723,-0.0189258532865581));
#45715=CARTESIAN_POINT('',(0.00690000000001,-0.0285787743898623,-0.0155508532865681));
#45716=CARTESIAN_POINT('',(0.0059,-0.0295787743898723,-0.0189258532865581));
#45717=CARTESIAN_POINT('Origin',(0.00690000000001,-0.0295787743898623,-0.0189258532865681));
#45718=CARTESIAN_POINT('',(0.00590000000001,-0.0295787743898623,-0.0155508532865681));
#45719=CARTESIAN_POINT('Origin',(0.00755,-0.0285787743898723,-0.0121758532865581));
#45720=CARTESIAN_POINT('',(0.0092,-0.0285787743898723,-0.0054258532865581));
#45721=CARTESIAN_POINT('',(0.00920000000001,-0.0285787743898623,-0.0054258532865681));
#45722=CARTESIAN_POINT('',(0.0092,-0.0285787743898723,-0.0189258532865581));
#45723=CARTESIAN_POINT('',(0.00920000000001,-0.0285787743898623,-0.0189258532865681));
#45724=CARTESIAN_POINT('',(0.00590000000001,-0.0285787743898623,-0.0189258532865681));
#45725=CARTESIAN_POINT('Origin',(0.0059,-0.0297787743898723,-0.0054258532865581));
#45726=CARTESIAN_POINT('',(0.0059,-0.0297787743898723,-0.0054258532865581));
#45727=CARTESIAN_POINT('',(0.00590000000001,-0.0297787743898623,-0.0054258532865681));
#45728=CARTESIAN_POINT('',(0.008,-0.0297787743898723,-0.0054258532865581));
#45729=CARTESIAN_POINT('',(0.00920000000001,-0.0297787743898623,-0.0054258532865681));
#45730=CARTESIAN_POINT('',(0.0092,-0.0297787743898723,-0.0054258532865581));
#45731=CARTESIAN_POINT('',(0.00695000000001,-0.0297787743898623,-0.0054258532865681));
#45732=CARTESIAN_POINT('',(0.00920000000001,-0.0297787743898623,-0.0054258532865681));
#45733=CARTESIAN_POINT('Origin',(0.00755,-0.0297787743898723,-0.0121758532865581));
#45734=CARTESIAN_POINT('',(0.008,-0.0297787743898723,-0.0189258532865581));
#45735=CARTESIAN_POINT('',(0.00800000000001,-0.0297787743898623,-0.0029758532865481));
#45736=CARTESIAN_POINT('',(0.0059,-0.0297787743898723,-0.0189258532865581));
#45737=CARTESIAN_POINT('',(0.00590000000001,-0.0297787743898623,-0.0054258532865681));
#45738=CARTESIAN_POINT('',(0.00590000000001,-0.0297787743898623,-0.0189258532865681));
#45739=CARTESIAN_POINT('Origin',(0.0059,-0.0297787743898723,-0.0189258532865581));
#45740=CARTESIAN_POINT('',(0.00590000000001,-0.0297787743898623,-0.0189258532865681));
#45741=CARTESIAN_POINT('Origin',(0.0092,-0.0297787743898723,-0.0189258532865581));
#45742=CARTESIAN_POINT('',(0.0092,-0.0297787743898723,-0.0189258532865581));
#45743=CARTESIAN_POINT('',(0.00920000000001,-0.0297787743898623,-0.0189258532865681));
#45744=CARTESIAN_POINT('',(0.00860000000001,-0.0297787743898623,-0.0189258532865681));
#45745=CARTESIAN_POINT('Origin',(0.008,-0.0297787743898723,-0.0041758532865581));
#45746=CARTESIAN_POINT('',(0.00920000000001,-0.0297787743898623,-0.0029758532865481));
#45747=CARTESIAN_POINT('',(0.008,-0.0297787743898723,-0.0041758532865581));
#45748=CARTESIAN_POINT('',(0.00800000000001,-0.0297787743898623,-0.0029758532865481));
#45749=CARTESIAN_POINT('',(0.0075,-0.0297787743898723,-0.0041758532865581));
#45750=CARTESIAN_POINT('',(-0.015,-0.0297787743898623,-0.0041758532865581));
#45751=CARTESIAN_POINT('',(0.0075,-0.0297787743898723,-0.0029758532865581));
#45752=CARTESIAN_POINT('',(0.00750000000001,-0.0297787743898623,-0.0041758532865581));
#45753=CARTESIAN_POINT('',(0.00800000000001,-0.0297787743898623,-0.0029758532865481));
#45754=CARTESIAN_POINT('Origin',(0.008,-0.0297787743898723,-0.0041758532865581));
#45755=CARTESIAN_POINT('',(0.0075,-0.0297787743898723,-0.0201758532865581));
#45756=CARTESIAN_POINT('',(0.00750000000001,-0.0297787743898623,-0.0029758532865481));
#45757=CARTESIAN_POINT('',(0.008,-0.0297787743898723,-0.0201758532865581));
#45758=CARTESIAN_POINT('',(0.00200000000001,-0.0297787743898623,-0.0201758532865681));
#45759=CARTESIAN_POINT('',(0.00800000000001,-0.0297787743898623,-0.0029758532865481));
#45760=CARTESIAN_POINT('',(0.00920000000001,-0.0297787743898623,-0.0029758532865481));
#45761=CARTESIAN_POINT('Origin',(-0.0129,-0.0297787743898723,-0.0054258532865581));
#45762=CARTESIAN_POINT('',(-0.0129,-0.0297787743898723,-0.0054258532865581));
#45763=CARTESIAN_POINT('',(-0.01289999999999,-0.0297787743898623,-0.0054258532865681));
#45764=CARTESIAN_POINT('',(-0.01289999999999,-0.0297787743898623,-0.0054258532865681));
#45765=CARTESIAN_POINT('Origin',(-0.0162,-0.0297787743898723,-0.0054258532865581));
#45766=CARTESIAN_POINT('',(-0.01620000000001,-0.0297787743898623,-0.0054258532865681));
#45767=CARTESIAN_POINT('Origin',(-0.01455,-0.0297787743898723,-0.0079258532865581));
#45768=CARTESIAN_POINT('',(-0.015,-0.0297787743898623,-0.0213758532865681));
#45769=CARTESIAN_POINT('Origin',(-0.0095,-0.0297787743898723,-0.0041758532865581));
#45770=CARTESIAN_POINT('',(-0.015,-0.0297787743898723,-0.0139258532865581));
#45771=CARTESIAN_POINT('',(-0.015,-0.0297787743898623,-0.0213758532865681));
#45772=CARTESIAN_POINT('',(-0.01284999999999,-0.0297787743898623,-0.0139258532865681));
#45773=CARTESIAN_POINT('Origin',(0.0045,-0.0297787743898723,-0.0062758532865581));
#45774=CARTESIAN_POINT('',(-0.0035,-0.0297787743898723,-0.0062758532865581));
#45775=CARTESIAN_POINT('',(-0.00349999999999,-0.0297787743898623,-0.0062758532865681));
#45776=CARTESIAN_POINT('',(-0.00349999999999,-0.0297787743898623,-0.0062758532865681));
#45777=CARTESIAN_POINT('Origin',(0.0005,-0.0297787743898723,-0.0046258532865581));
#45778=CARTESIAN_POINT('',(-0.0035,-0.0297787743898723,-0.0041758532865581));
#45779=CARTESIAN_POINT('',(-0.015,-0.0297787743898623,-0.0041758532865581));
#45780=CARTESIAN_POINT('',(-0.00349999999999,-0.0297787743898623,-0.0029758532865481));
#45781=CARTESIAN_POINT('Origin',(-0.01455,-0.0297787743898723,-0.0164258532865581));
#45782=CARTESIAN_POINT('',(-0.015,-0.0297787743898623,-0.0213758532865681));
#45783=CARTESIAN_POINT('',(-0.0129,-0.0297787743898723,-0.0139258532865581));
#45784=CARTESIAN_POINT('',(-0.01289999999999,-0.0297787743898623,-0.0189258532865681));
#45785=CARTESIAN_POINT('',(-0.01289999999999,-0.0297787743898623,-0.0139258532865681));
#45786=CARTESIAN_POINT('Origin',(-0.0129,-0.0297787743898723,-0.0139258532865581));
#45787=CARTESIAN_POINT('',(-0.01289999999999,-0.0297787743898623,-0.0139258532865681));
#45788=CARTESIAN_POINT('Origin',(-0.0162,-0.0297787743898723,-0.0139258532865581));
#45789=CARTESIAN_POINT('Origin',(-0.0035,-0.0297787743898723,-0.0180758532865581));
#45790=CARTESIAN_POINT('',(0.0045,-0.0297787743898723,-0.0180758532865581));
#45791=CARTESIAN_POINT('',(-0.00349999999999,-0.0297787743898623,-0.0180758532865681));
#45792=CARTESIAN_POINT('',(0.00450000000001,-0.0297787743898623,-0.0180758532865681));
#45793=CARTESIAN_POINT('Origin',(0.0005,-0.0297787743898723,-0.0197258532865581));
#45794=CARTESIAN_POINT('',(0.0045,-0.0297787743898723,-0.0201758532865581));
#45795=CARTESIAN_POINT('',(-0.00349999999999,-0.0297787743898623,-0.0201758532865681));
#45796=CARTESIAN_POINT('',(0.00450000000001,-0.0297787743898623,-0.0180758532865681));
#45797=CARTESIAN_POINT('Origin',(0.,-0.0440787743898723,-0.0121758532865581));
#45798=CARTESIAN_POINT('',(-0.00525,-0.0440787743898823,-0.0121758532865581));
#45799=CARTESIAN_POINT('Origin',(-0.00685,-0.0440787743898723,-0.0121758532865581));
#45800=CARTESIAN_POINT('Origin',(1.00006808390063E-14,-0.0440787743898823,
-0.0121758532865681));
#45801=CARTESIAN_POINT('Origin',(0.,-0.0412787743898723,-0.0121758532865581));
#45802=CARTESIAN_POINT('',(-0.0041,-0.0412787743898723,-0.0121758532865581));
#45803=CARTESIAN_POINT('Origin',(1.00006808390063E-14,-0.0412787743898723,
-0.0121758532865681));
#45804=CARTESIAN_POINT('',(-0.0041,-0.0440787743898823,-0.0121758532865581));
#45805=CARTESIAN_POINT('',(-0.0041,-0.0412787743898723,-0.0121758532865581));
#45806=CARTESIAN_POINT('Origin',(1.00006808390063E-14,-0.0440787743898823,
-0.0121758532865681));
#45807=CARTESIAN_POINT('Origin',(0.,-0.0440787743898723,-0.0121758532865581));
#45808=CARTESIAN_POINT('Origin',(-0.0035,-0.0412787743898723,-0.0121758532865581));
#45809=CARTESIAN_POINT('',(-0.015,-0.0412787743898723,-0.0121758532865581));
#45810=CARTESIAN_POINT('Origin',(-0.01249999999999,-0.0412787743898723,
-0.0121758532865681));
#45811=CARTESIAN_POINT('',(-0.015,-0.0412787743898723,-0.00417585328655811));
#45812=CARTESIAN_POINT('',(-0.015,-0.0412787743898723,-0.00297585328654811));
#45813=CARTESIAN_POINT('',(0.008,-0.0412787743898723,-0.00417585328655811));
#45814=CARTESIAN_POINT('',(0.00800000000001,-0.0412787743898723,-0.00417585328655811));
#45815=CARTESIAN_POINT('',(0.008,-0.0412787743898723,-0.0201758532865581));
#45816=CARTESIAN_POINT('',(0.00800000000001,-0.0412787743898723,-0.0213758532865681));
#45817=CARTESIAN_POINT('',(-0.015,-0.0412787743898723,-0.0201758532865581));
#45818=CARTESIAN_POINT('',(0.00225000000001,-0.0412787743898723,-0.0201758532865681));
#45819=CARTESIAN_POINT('',(-0.015,-0.0412787743898723,-0.00297585328654811));
#45820=CARTESIAN_POINT('Origin',(-0.0125,-0.0412787743898723,-0.0121758532865581));
#45821=CARTESIAN_POINT('',(-0.015,-0.0412787743898723,-0.0121758532865581));
#45822=CARTESIAN_POINT('Origin',(0.008,-0.0355287743898723,-0.0121758532865581));
#45823=CARTESIAN_POINT('',(0.00800000000001,-0.0297787743898623,-0.0041758532865581));
#45824=CARTESIAN_POINT('',(0.00800000000001,-0.0326537743470214,-0.0201758532865681));
#45825=CARTESIAN_POINT('Origin',(0.0092,-0.0355287743898723,-0.0121758532865581));
#45826=CARTESIAN_POINT('Origin',(-0.0035,-0.0355287743041906,-0.0201758532865581));
#45827=CARTESIAN_POINT('',(0.0045,-0.035138261906077,-0.0201758532865581));
#45828=CARTESIAN_POINT('',(0.00450000000001,-0.0326537743470214,-0.0201758532865681));
#45829=CARTESIAN_POINT('',(-0.0095,-0.0372787743898723,-0.0201758532865581));
#45830=CARTESIAN_POINT('Origin',(-0.00649999999999,-0.0372787743898623,
-0.0201758532865681));
#45831=CARTESIAN_POINT('',(-0.00949999999999,-0.0326537743470214,-0.0201758532865681));
#45832=CARTESIAN_POINT('',(-0.015,-0.0355287743470215,-0.0201758532865681));
#45833=CARTESIAN_POINT('',(0.0075,-0.035138261906077,-0.0201758532865581));
#45834=CARTESIAN_POINT('',(0.00750000000001,-0.0353335181051238,-0.0201758532865681));
#45835=CARTESIAN_POINT('Origin',(0.00600000000001,-0.0355287743898623,-0.0201758532865681));
#45836=CARTESIAN_POINT('Origin',(-0.0095,-0.0297787743898723,-0.0029758532865581));
#45837=CARTESIAN_POINT('',(-0.00949999999999,-0.0372787743898623,-0.0029758532865481));
#45838=CARTESIAN_POINT('Origin',(-0.0065,-0.0372787743898723,-0.00297585328655811));
#45839=CARTESIAN_POINT('Origin',(0.0045,-0.0297787743898723,-0.0029758532865581));
#45840=CARTESIAN_POINT('',(0.00450000000001,-0.035138261906067,-0.0029758532865481));
#45841=CARTESIAN_POINT('Origin',(0.0075,-0.035138261906077,-0.00297585328655811));
#45842=CARTESIAN_POINT('',(0.00750000000001,-0.035138261906067,-0.0029758532865481));
#45843=CARTESIAN_POINT('Origin',(0.006,-0.0355287743898723,-0.00297585328655811));
#45844=CARTESIAN_POINT('Origin',(-0.015,-0.0355287743898723,-0.0121758532865581));
#45845=CARTESIAN_POINT('',(-0.015,-0.0412787743898723,-0.00417585328655811));
#45846=CARTESIAN_POINT('Origin',(0.006,-0.0355287743898723,-0.0041758532865581));
#45847=CARTESIAN_POINT('',(0.0075,-0.035138261906077,-0.0041758532865581));
#45848=CARTESIAN_POINT('Origin',(0.00600000000001,-0.0355287743898623,-0.0041758532865581));
#45849=CARTESIAN_POINT('',(0.0075,-0.035138261906077,-0.00297585328655811));
#45850=CARTESIAN_POINT('Origin',(0.00600000000001,-0.0355287743898623,-0.0029758532865481));
#45851=CARTESIAN_POINT('',(0.00750000000001,-0.035138261906067,-0.0041758532865581));
#45852=CARTESIAN_POINT('Origin',(0.0075,-0.0297787743898723,-0.0041758532865581));
#45853=CARTESIAN_POINT('',(0.00750000000001,-0.0355287743898623,-0.0041758532865581));
#45854=CARTESIAN_POINT('',(0.00750000000001,-0.0355287743898623,-0.0029758532865481));
#45855=CARTESIAN_POINT('Origin',(-0.0095,-0.0372787743898723,-0.0041758532865581));
#45856=CARTESIAN_POINT('',(-0.0095,-0.0372787743898723,-0.0041758532865581));
#45857=CARTESIAN_POINT('',(-0.00949999999999,-0.0372787743898623,-0.0041758532865581));
#45858=CARTESIAN_POINT('',(-0.0095,-0.0372787743898723,-0.00297585328655811));
#45859=CARTESIAN_POINT('',(-0.00949999999999,-0.0372787743898623,-0.0029758532865481));
#45860=CARTESIAN_POINT('',(-0.00949999999999,-0.0372787743898623,-0.0041758532865581));
#45861=CARTESIAN_POINT('Origin',(-0.0065,-0.0372787743898723,-0.0041758532865581));
#45862=CARTESIAN_POINT('',(-0.0035,-0.0372787743898723,-0.0041758532865581));
#45863=CARTESIAN_POINT('Origin',(-0.00649999999999,-0.0372787743898623,
-0.0041758532865581));
#45864=CARTESIAN_POINT('',(-0.0035,-0.0372787743898723,-0.00297585328655811));
#45865=CARTESIAN_POINT('Origin',(-0.00649999999999,-0.0372787743898623,
-0.0029758532865481));
#45866=CARTESIAN_POINT('',(-0.00349999999999,-0.0372787743898623,-0.0041758532865581));
#45867=CARTESIAN_POINT('Origin',(-0.0035,-0.0297787743898723,-0.0041758532865581));
#45868=CARTESIAN_POINT('',(-0.00349999999999,-0.0372787743898623,-0.0041758532865581));
#45869=CARTESIAN_POINT('',(-0.00349999999999,-0.0297787743898623,-0.0029758532865481));
#45870=CARTESIAN_POINT('Origin',(-0.0035,-0.0355287743041906,-0.00297585328655811));
#45871=CARTESIAN_POINT('Origin',(-0.0035,-0.0355287743041906,-0.0041758532865581));
#45872=CARTESIAN_POINT('',(0.,0.,0.));
#45873=CARTESIAN_POINT('Origin',(0.006,-0.0355287743898723,-0.0193758532865581));
#45874=CARTESIAN_POINT('',(0.00536607260738471,-0.0368882360704363,-0.0191758532865481));
#45875=CARTESIAN_POINT('Origin',(0.006,-0.0355287743898723,-0.0191758532865481));
#45876=CARTESIAN_POINT('',(0.00553511991208311,-0.0365257129556171,-0.0195758532865531));
#45877=CARTESIAN_POINT('',(0.00545059625973708,-0.0367069745130199,-0.0193758532865581));
#45878=CARTESIAN_POINT('Origin',(0.006,-0.0355287743898723,-0.0195758532865581));
#45879=CARTESIAN_POINT('Origin',(0.006,-0.0355287743898723,-0.0195758532865581));
#45880=CARTESIAN_POINT('',(0.00536607260738894,-0.0368882360704273,-0.0045758532865481));
#45881=CARTESIAN_POINT('Origin',(0.006,-0.0355287743898724,-0.0045758532865481));
#45882=CARTESIAN_POINT('',(0.00536607260738894,-0.0368882360704273,-0.0195758532865581));
#45883=CARTESIAN_POINT('Origin',(0.006,-0.0355287743898723,-0.0195758532865581));
#45884=CARTESIAN_POINT('Origin',(0.006,-0.0355287743898724,-0.0045758532865581));
#45885=CARTESIAN_POINT('',(0.,0.,0.));
#45886=CARTESIAN_POINT('Origin',(-0.0125,-0.0332787743898722,-0.0121758532865583));
#45887=CARTESIAN_POINT('',(-0.0125000000000001,-0.0410287743898722,-0.013675853286558));
#45888=CARTESIAN_POINT('',(-0.0125,-0.0410912743898722,-0.013675853286558));
#45889=CARTESIAN_POINT('',(-0.0125,-0.0332787743898722,-0.0136758532865583));
#45890=CARTESIAN_POINT('',(-0.0125,-0.0412787743898722,-0.0106758532865581));
#45891=CARTESIAN_POINT('Ctrl Pts',(-0.0125000000000001,-0.0410287743898722,
-0.013675853286558));
#45892=CARTESIAN_POINT('Ctrl Pts',(-0.0123310037568044,-0.0410369052254139,
-0.013675853286558));
#45893=CARTESIAN_POINT('Ctrl Pts',(-0.0121630120248185,-0.0410457809002103,
-0.0136472992089388));
#45894=CARTESIAN_POINT('Ctrl Pts',(-0.011817556294753,-0.0410657705028026,
-0.0135260203918559));
#45895=CARTESIAN_POINT('Ctrl Pts',(-0.0116465966412278,-0.0410768017393218,
-0.013425006683115));
#45896=CARTESIAN_POINT('Ctrl Pts',(-0.0113584236030566,-0.041097826154242,
-0.0131672580894708));
#45897=CARTESIAN_POINT('Ctrl Pts',(-0.0112422133833523,-0.0411071596872922,
-0.0130149179329953));
#45898=CARTESIAN_POINT('Ctrl Pts',(-0.0110687981756656,-0.0411264893050654,
-0.0126669848130804));
#45899=CARTESIAN_POINT('Ctrl Pts',(-0.0110163755255651,-0.041137257974845,
-0.0124731487570469));
#45900=CARTESIAN_POINT('Ctrl Pts',(-0.0109904456301969,-0.0411590554039909,
-0.0120807950324208));
#45901=CARTESIAN_POINT('Ctrl Pts',(-0.0110154549296438,-0.0411698689270392,
-0.0118861516175517));
#45902=CARTESIAN_POINT('Ctrl Pts',(-0.0111374431285804,-0.0411902090678481,
-0.0115200290829898));
#45903=CARTESIAN_POINT('Ctrl Pts',(-0.0112321814406848,-0.0411990041550593,
-0.0113516555803048));
#45904=CARTESIAN_POINT('Ctrl Pts',(-0.0114852510225052,-0.0412194684440373,
-0.0110532705506603));
#45905=CARTESIAN_POINT('Ctrl Pts',(-0.0116435964173627,-0.0412305591150924,
-0.0109282686617132));
#45906=CARTESIAN_POINT('Ctrl Pts',(-0.0119282935685727,-0.0412482657298701,
-0.0107839404603842));
#45907=CARTESIAN_POINT('Ctrl Pts',(-0.0120409179303487,-0.0412548259507756,
-0.0107428436245518));
#45908=CARTESIAN_POINT('Ctrl Pts',(-0.0122696303330434,-0.0412673211268715,
-0.0106891587868862));
#45909=CARTESIAN_POINT('Ctrl Pts',(-0.0123846449056647,-0.0412732243653083,
-0.010675853286558));
#45910=CARTESIAN_POINT('Ctrl Pts',(-0.0125000000000008,-0.0412787743898722,
-0.010675853286558));
#45911=CARTESIAN_POINT('',(-0.0114490560961827,-0.0412787743898703,-0.0111055650491926));
#45912=CARTESIAN_POINT('Origin',(-0.0125,-0.0412787743898622,-0.0121758532865581));
#45913=CARTESIAN_POINT('Ctrl Pts',(-0.0114490560961864,-0.0412787743898736,
-0.0111055650491953));
#45914=CARTESIAN_POINT('Ctrl Pts',(-0.011369903560121,-0.0412728072190045,
-0.0111832869864692));
#45915=CARTESIAN_POINT('Ctrl Pts',(-0.0112996137814574,-0.0412670291836058,
-0.0112695507929254));
#45916=CARTESIAN_POINT('Ctrl Pts',(-0.0111804215237056,-0.041256161491045,
-0.0114543406788185));
#45917=CARTESIAN_POINT('Ctrl Pts',(-0.0111315202178879,-0.0412509305323926,
-0.0115520427211916));
#45918=CARTESIAN_POINT('Ctrl Pts',(-0.0110262339331569,-0.0412351603642107,
-0.0118359057484655));
#45919=CARTESIAN_POINT('Ctrl Pts',(-0.0109946931267627,-0.0412244372150451,
-0.0120289224334467));
#45920=CARTESIAN_POINT('Ctrl Pts',(-0.0110069213898787,-0.0412026370083603,
-0.012421326153772));
#45921=CARTESIAN_POINT('Ctrl Pts',(-0.0110525758723153,-0.0411917716832378,
-0.0126169020059778));
#45922=CARTESIAN_POINT('Ctrl Pts',(-0.0112138449798316,-0.0411721120389683,
-0.0129707756028294));
#45923=CARTESIAN_POINT('Ctrl Pts',(-0.0113247528666018,-0.0411630611644425,
-0.0131271171485231));
#45924=CARTESIAN_POINT('Ctrl Pts',(-0.0116033993474256,-0.0411422340676681,
-0.0133942627702646));
#45925=CARTESIAN_POINT('Ctrl Pts',(-0.0117700971634697,-0.0411312526809726,
-0.0135008636044037));
#45926=CARTESIAN_POINT('Ctrl Pts',(-0.012127119866988,-0.0411101878892364,
-0.0136408146449594));
#45927=CARTESIAN_POINT('Ctrl Pts',(-0.0123128074865679,-0.0411002806938739,
-0.013675853286558));
#45928=CARTESIAN_POINT('Ctrl Pts',(-0.0125,-0.0410912743898722,-0.013675853286558));
#45929=CARTESIAN_POINT('Origin',(-0.0125,-0.0332787743898722,-0.0121758532865583));
#45930=CARTESIAN_POINT('',(-0.0125000000060198,-0.0405287743892929,-0.0136758532865581));
#45931=CARTESIAN_POINT('',(-0.0125,-0.0405912743898722,-0.013675853286558));
#45932=CARTESIAN_POINT('',(-0.0125,-0.0332787743898722,-0.0136758532865583));
#45933=CARTESIAN_POINT('Ctrl Pts',(-0.0125000000120396,-0.0405287743892929,
-0.013675853286558));
#45934=CARTESIAN_POINT('Ctrl Pts',(-0.0124987572094776,-0.0405288341836588,
-0.013675853286568));
#45935=CARTESIAN_POINT('Ctrl Pts',(-0.0124975143416151,-0.0405288940240707,
-0.0136758517420196));
#45936=CARTESIAN_POINT('Ctrl Pts',(-0.0122974686446526,-0.0405385325399391,
-0.013675354481734));
#45937=CARTESIAN_POINT('Ctrl Pts',(-0.0121007703785393,-0.0405491076079653,
-0.0136353434234573));
#45938=CARTESIAN_POINT('Ctrl Pts',(-0.0117374538093306,-0.0405708394897221,
-0.0134822784373148));
#45939=CARTESIAN_POINT('Ctrl Pts',(-0.0115738416018138,-0.0405817781404356,
-0.0133718716677857));
#45940=CARTESIAN_POINT('Ctrl Pts',(-0.011301901014316,-0.0406024633052192,
-0.0130982206497631));
#45941=CARTESIAN_POINT('Ctrl Pts',(-0.0111947045203311,-0.0406113771296748,
-0.0129390039701075));
#45942=CARTESIAN_POINT('Ctrl Pts',(-0.011042116736427,-0.0406312662509237,
-0.0125809997876281));
#45943=CARTESIAN_POINT('Ctrl Pts',(-0.0110013057341337,-0.0406421920366129,
-0.0123843356452229));
#45944=CARTESIAN_POINT('Ctrl Pts',(-0.0109987917193966,-0.0406639779942384,
-0.0119921884079635));
#45945=CARTESIAN_POINT('Ctrl Pts',(-0.011034922411109,-0.0406746296998768,
-0.011800457706473));
#45946=CARTESIAN_POINT('Ctrl Pts',(-0.0111781023805049,-0.0406946024933454,
-0.0114409474240369));
#45947=CARTESIAN_POINT('Ctrl Pts',(-0.0112838956978466,-0.0407035761797072,
-0.0112766344138636));
#45948=CARTESIAN_POINT('Ctrl Pts',(-0.0115555377678104,-0.040724503960149,
-0.0109937321846102));
#45949=CARTESIAN_POINT('Ctrl Pts',(-0.0117201175586749,-0.0407356025304129,
-0.0108792442147851));
#45950=CARTESIAN_POINT('Ctrl Pts',(-0.0120774319930893,-0.0407571067909325,
-0.0107239775907649));
#45951=CARTESIAN_POINT('Ctrl Pts',(-0.0122656438239637,-0.0407673282668937,
-0.0106819969098197));
#45952=CARTESIAN_POINT('Ctrl Pts',(-0.0126553925473199,-0.0407863927730581,
-0.0106707392789394));
#45953=CARTESIAN_POINT('Ctrl Pts',(-0.0128533159096088,-0.0407965705151329,
-0.0107045526893804));
#45954=CARTESIAN_POINT('Ctrl Pts',(-0.013221934375852,-0.0408182477555405,
-0.0108464674319101));
#45955=CARTESIAN_POINT('Ctrl Pts',(-0.013389366022574,-0.0408292385129775,
-0.0109521345807257));
#45956=CARTESIAN_POINT('Ctrl Pts',(-0.0136696297580511,-0.0408500994714692,
-0.0112176980570621));
#45957=CARTESIAN_POINT('Ctrl Pts',(-0.0137814349586155,-0.0408591910787262,
-0.0113733536859315));
#45958=CARTESIAN_POINT('Ctrl Pts',(-0.0139447812266889,-0.0408787950173215,
-0.0117262245806454));
#45959=CARTESIAN_POINT('Ctrl Pts',(-0.0139915942490026,-0.0408896448117446,
-0.0119215208802603));
#45960=CARTESIAN_POINT('Ctrl Pts',(-0.0140061572662983,-0.0409114464355421,
-0.0123139501086151));
#45961=CARTESIAN_POINT('Ctrl Pts',(-0.0139757246497111,-0.0409221858438013,
-0.0125072594572816));
#45962=CARTESIAN_POINT('Ctrl Pts',(-0.0138434593065443,-0.0409423501554539,
-0.0128702170670279));
#45963=CARTESIAN_POINT('Ctrl Pts',(-0.0137434259685003,-0.0409511935153639,
-0.013036618757154));
#45964=CARTESIAN_POINT('Ctrl Pts',(-0.0134813821431137,-0.0409718843948055,
-0.0133276171976694));
#45965=CARTESIAN_POINT('Ctrl Pts',(-0.0133199546623563,-0.0409829838826118,
-0.0134475981602884));
#45966=CARTESIAN_POINT('Ctrl Pts',(-0.0129665065567941,-0.0410046194391406,
-0.0136142881186541));
#45967=CARTESIAN_POINT('Ctrl Pts',(-0.0127790874858517,-0.0410149640512427,
-0.0136620748011502));
#45968=CARTESIAN_POINT('Ctrl Pts',(-0.0125584819942821,-0.0410259369456405,
-0.0136749990796436));
#45969=CARTESIAN_POINT('Ctrl Pts',(-0.0125292271033337,-0.0410273682002074,
-0.013675853286558));
#45970=CARTESIAN_POINT('Ctrl Pts',(-0.0125000000000001,-0.0410287743898722,
-0.013675853286558));
#45971=CARTESIAN_POINT('Ctrl Pts',(-0.0125,-0.0410912743898722,-0.013675853286558));
#45972=CARTESIAN_POINT('Ctrl Pts',(-0.0125113747299722,-0.0410907271229213,
-0.013675853286558));
#45973=CARTESIAN_POINT('Ctrl Pts',(-0.0125227546763987,-0.0410901760109885,
-0.0136757239023752));
#45974=CARTESIAN_POINT('Ctrl Pts',(-0.0127251001422328,-0.0410803127085477,
-0.0136711176420125));
#45975=CARTESIAN_POINT('Ctrl Pts',(-0.0129134534013763,-0.0410701177212372,
-0.0136303355134427));
#45976=CARTESIAN_POINT('Ctrl Pts',(-0.0132715207217928,-0.0410486429794191,
-0.0134774355994801));
#45977=CARTESIAN_POINT('Ctrl Pts',(-0.0134367284628191,-0.0410375459405851,
-0.0133640904027179));
#45978=CARTESIAN_POINT('Ctrl Pts',(-0.0137103402832416,-0.0410165702878582,
-0.0130828764790717));
#45979=CARTESIAN_POINT('Ctrl Pts',(-0.0138173294561724,-0.0410075597821429,
-0.0129189903474292));
#45980=CARTESIAN_POINT('Ctrl Pts',(-0.0139627406925233,-0.0409876267591427,
-0.0125601959334253));
#45981=CARTESIAN_POINT('Ctrl Pts',(-0.0140000274969595,-0.0409769941033067,
-0.0123688081283793));
#45982=CARTESIAN_POINT('Ctrl Pts',(-0.013999971375087,-0.040955102830591,
-0.0119747652194958));
#45983=CARTESIAN_POINT('Ctrl Pts',(-0.0139595925151208,-0.0409440550648995,
-0.0117759054370492));
#45984=CARTESIAN_POINT('Ctrl Pts',(-0.0138070343033204,-0.0409240423457135,
-0.0114156764917013));
#45985=CARTESIAN_POINT('Ctrl Pts',(-0.0137001812896997,-0.0409151386209105,
-0.011256190631885));
#45986=CARTESIAN_POINT('Ctrl Pts',(-0.0134288624351978,-0.0408944667371465,
-0.0109819408574324));
#45987=CARTESIAN_POINT('Ctrl Pts',(-0.0132655396963218,-0.0408835323615525,
-0.0108711866178111));
#45988=CARTESIAN_POINT('Ctrl Pts',(-0.0129026172736487,-0.0408617964416594,
-0.010717293576936));
#45989=CARTESIAN_POINT('Ctrl Pts',(-0.0127060091691163,-0.0408512130176722,
-0.0106768255396282));
#45990=CARTESIAN_POINT('Ctrl Pts',(-0.0123168175128777,-0.0408324360956953,
-0.0106749560709455));
#45991=CARTESIAN_POINT('Ctrl Pts',(-0.0121279086191053,-0.0408224153260697,
-0.0107102984066759));
#45992=CARTESIAN_POINT('Ctrl Pts',(-0.0117665402452652,-0.0408010779468522,
-0.0108525356747639));
#45993=CARTESIAN_POINT('Ctrl Pts',(-0.0115985989294966,-0.0407899934803529,
-0.0109606935771387));
#45994=CARTESIAN_POINT('Ctrl Pts',(-0.0113161557621315,-0.0407688064846784,
-0.0112342195052963));
#45995=CARTESIAN_POINT('Ctrl Pts',(-0.0112037429817825,-0.0407595888241137,
-0.0113961934702125));
#45996=CARTESIAN_POINT('Ctrl Pts',(-0.0110483591824526,-0.0407398361172091,
-0.0117517421944951));
#45997=CARTESIAN_POINT('Ctrl Pts',(-0.0110059452638139,-0.0407292931602785,
-0.0119415154192466));
#45998=CARTESIAN_POINT('Ctrl Pts',(-0.0109950050778346,-0.040707471801418,
-0.012334299878735));
#45999=CARTESIAN_POINT('Ctrl Pts',(-0.0110295836685338,-0.0406963977400064,
-0.0125336329841446));
#46000=CARTESIAN_POINT('Ctrl Pts',(-0.0111715482076857,-0.0406761503208377,
-0.0128980865291808));
#46001=CARTESIAN_POINT('Ctrl Pts',(-0.0112740700591782,-0.0406673359253655,
-0.0130610109528272));
#46002=CARTESIAN_POINT('Ctrl Pts',(-0.0115375390549893,-0.0406468334447887,
-0.013342758566626));
#46003=CARTESIAN_POINT('Ctrl Pts',(-0.0116971602707559,-0.0406359575123747,
-0.0134578200778564));
#46004=CARTESIAN_POINT('Ctrl Pts',(-0.0120549643964648,-0.0406141809859732,
-0.0136220401034243));
#46005=CARTESIAN_POINT('Ctrl Pts',(-0.0122503452868441,-0.0406034974610594,
-0.0136682373713582));
#46006=CARTESIAN_POINT('Ctrl Pts',(-0.0124660532323911,-0.0405929156522489,
-0.0136755653672513));
#46007=CARTESIAN_POINT('Ctrl Pts',(-0.012483031769083,-0.0405920907742628,
-0.013675853286558));
#46008=CARTESIAN_POINT('Ctrl Pts',(-0.0125,-0.0405912743898722,-0.013675853286558));
#46009=CARTESIAN_POINT('Origin',(-0.0125,-0.0332787743898722,-0.0121758532865583));
#46010=CARTESIAN_POINT('',(-0.0124999999999999,-0.0400287743898722,-0.0136758532865581));
#46011=CARTESIAN_POINT('',(-0.0124999999999999,-0.0400912743898722,-0.0136758532865581));
#46012=CARTESIAN_POINT('',(-0.0125,-0.0332787743898722,-0.0136758532865583));
#46013=CARTESIAN_POINT('Ctrl Pts',(-0.0124999999999999,-0.0400287743898722,
-0.0136758532865581));
#46014=CARTESIAN_POINT('Ctrl Pts',(-0.0124694471611225,-0.0400302443640181,
-0.0136758532865581));
#46015=CARTESIAN_POINT('Ctrl Pts',(-0.0124388664803809,-0.0400317416070417,
-0.0136749198304824));
#46016=CARTESIAN_POINT('Ctrl Pts',(-0.0122098031798663,-0.040043152132264,
-0.0136608901971213));
#46017=CARTESIAN_POINT('Ctrl Pts',(-0.0120157224682894,-0.0400539206585675,
-0.0136093809034139));
#46018=CARTESIAN_POINT('Ctrl Pts',(-0.0116629600624993,-0.0400757180652648,
-0.0134356766721402));
#46019=CARTESIAN_POINT('Ctrl Pts',(-0.0115068921859352,-0.0400865317053801,
-0.0133167031196287));
#46020=CARTESIAN_POINT('Ctrl Pts',(-0.0112508017365673,-0.040106872136986,
-0.0130280092514512));
#46021=CARTESIAN_POINT('Ctrl Pts',(-0.0111523479187016,-0.0401156672027425,
-0.0128617826548918));
#46022=CARTESIAN_POINT('Ctrl Pts',(-0.0110204556653628,-0.0401361311101657,
-0.0124934323212756));
#46023=CARTESIAN_POINT('Ctrl Pts',(-0.010991363760272,-0.0401472217588229,
-0.0122938006454451));
#46024=CARTESIAN_POINT('Ctrl Pts',(-0.0110126554031447,-0.0401689616212987,
-0.0119024831208814));
#46025=CARTESIAN_POINT('Ctrl Pts',(-0.0110598708065288,-0.0401794126837581,
-0.0117143639966109));
#46026=CARTESIAN_POINT('Ctrl Pts',(-0.0112247217947709,-0.040198990321795,
-0.0113619665119461));
#46027=CARTESIAN_POINT('Ctrl Pts',(-0.0113424057089055,-0.0402084693809643,
-0.0112018214805116));
#46028=CARTESIAN_POINT('Ctrl Pts',(-0.0116332683993669,-0.0402298525779533,
-0.0109358153468117));
#46029=CARTESIAN_POINT('Ctrl Pts',(-0.0118036878778282,-0.0402409162520149,
-0.0108326982758898));
#46030=CARTESIAN_POINT('Ctrl Pts',(-0.0121679453562284,-0.0402621064966329,
-0.010700761929268));
#46031=CARTESIAN_POINT('Ctrl Pts',(-0.0123573587950066,-0.0402717657912653,
-0.0106706055510168));
#46032=CARTESIAN_POINT('Ctrl Pts',(-0.0127460490307744,-0.0402908073618348,
-0.010682870854761));
#46033=CARTESIAN_POINT('Ctrl Pts',(-0.0129415380509213,-0.0403014829530466,
-0.010728595223169));
#46034=CARTESIAN_POINT('Ctrl Pts',(-0.0132997771202757,-0.0403232568342346,
-0.0108919666765583));
#46035=CARTESIAN_POINT('Ctrl Pts',(-0.0134597089744393,-0.0403341379321879,
-0.0110066761057188));
#46036=CARTESIAN_POINT('Ctrl Pts',(-0.0137238299600728,-0.0403546546024114,
-0.0112878052673025));
#46037=CARTESIAN_POINT('Ctrl Pts',(-0.0138267112847511,-0.0403634737192496,
-0.0114504412153531));
#46038=CARTESIAN_POINT('Ctrl Pts',(-0.0139695604469646,-0.0403837018117274,
-0.0118145468799539));
#46039=CARTESIAN_POINT('Ctrl Pts',(-0.0140046223532685,-0.0403947740259202,
-0.0120138467354232));
#46040=CARTESIAN_POINT('Ctrl Pts',(-0.013994596363098,-0.0404166018478708,
-0.0124067475305343));
#46041=CARTESIAN_POINT('Ctrl Pts',(-0.0139526076603594,-0.0404271525714348,
-0.0125966605546868));
#46042=CARTESIAN_POINT('Ctrl Pts',(-0.0137980560284191,-0.0404469204853329,
-0.0129524830048515));
#46043=CARTESIAN_POINT('Ctrl Pts',(-0.0136861008222104,-0.0404561181892372,
-0.0131146169506719));
#46044=CARTESIAN_POINT('Ctrl Pts',(-0.013404396191646,-0.0404772877229826,
-0.0133887934326412));
#46045=CARTESIAN_POINT('Ctrl Pts',(-0.0132366782755996,-0.0404883736009471,
-0.013497389087432));
#46046=CARTESIAN_POINT('Ctrl Pts',(-0.0128767235416822,-0.0405096552507722,
-0.0136400685935656));
#46047=CARTESIAN_POINT('Ctrl Pts',(-0.0126891657892081,-0.0405196731465533,
-0.0136758532850397));
#46048=CARTESIAN_POINT('Ctrl Pts',(-0.0125000000120396,-0.0405287743892929,
-0.013675853286558));
#46049=CARTESIAN_POINT('Ctrl Pts',(-0.0125,-0.0405912743898722,-0.013675853286558));
#46050=CARTESIAN_POINT('Ctrl Pts',(-0.0126727962989084,-0.0405829607240647,
-0.013675853286558));
#46051=CARTESIAN_POINT('Ctrl Pts',(-0.0128444453311079,-0.0405738729629493,
-0.0136459987312399));
#46052=CARTESIAN_POINT('Ctrl Pts',(-0.0131929587111633,-0.040553625536909,
-0.0135207342751592));
#46053=CARTESIAN_POINT('Ctrl Pts',(-0.0133635929868223,-0.0405425641398687,
-0.0134180712166641));
#46054=CARTESIAN_POINT('Ctrl Pts',(-0.0136552065447141,-0.0405211637088506,
-0.0131527451984548));
#46055=CARTESIAN_POINT('Ctrl Pts',(-0.0137733655749261,-0.0405116583157249,
-0.0129927639519044));
#46056=CARTESIAN_POINT('Ctrl Pts',(-0.0139390592873679,-0.0404920964463481,
-0.012640650303122));
#46057=CARTESIAN_POINT('Ctrl Pts',(-0.0139866987686684,-0.0404816538751068,
-0.0124526840207797));
#46058=CARTESIAN_POINT('Ctrl Pts',(-0.0140089072219678,-0.0404599219717202,
-0.012061509759821));
#46059=CARTESIAN_POINT('Ctrl Pts',(-0.0139803025204997,-0.0404488302397,
-0.0118618585834583));
#46060=CARTESIAN_POINT('Ctrl Pts',(-0.013849307610282,-0.0404283473669271,
-0.0114931668735456));
#46061=CARTESIAN_POINT('Ctrl Pts',(-0.0137512141637692,-0.0404195509932525,
-0.011326644505451));
#46062=CARTESIAN_POINT('Ctrl Pts',(-0.0134957770731844,-0.0403992250386819,
-0.0110373401599413));
#46063=CARTESIAN_POINT('Ctrl Pts',(-0.0133400270608699,-0.0403884172488764,
-0.0109180266615527));
#46064=CARTESIAN_POINT('Ctrl Pts',(-0.01298772143095,-0.0403666187882543,
-0.01074349332997));
#46065=CARTESIAN_POINT('Ctrl Pts',(-0.0127937625255864,-0.0403558431576918,
-0.0106915173083895));
#46066=CARTESIAN_POINT('Ctrl Pts',(-0.012405793577543,-0.0403364909631712,
-0.010666820235419));
#46067=CARTESIAN_POINT('Ctrl Pts',(-0.0122157058669701,-0.0403271798962426,
-0.0106908431745191));
#46068=CARTESIAN_POINT('Ctrl Pts',(-0.0118481678724113,-0.0403061687289893,
-0.0108106507153509));
#46069=CARTESIAN_POINT('Ctrl Pts',(-0.0116750154297604,-0.0402951404696745,
-0.0109077592225594));
#46070=CARTESIAN_POINT('Ctrl Pts',(-0.0113743103213689,-0.0402735349761782,
-0.0111647204625964));
#46071=CARTESIAN_POINT('Ctrl Pts',(-0.0112503297515439,-0.0402636715557126,
-0.0113227043014299));
#46072=CARTESIAN_POINT('Ctrl Pts',(-0.0110744481394087,-0.0402443027342696,
-0.0116713430874041));
#46073=CARTESIAN_POINT('Ctrl Pts',(-0.0110217276392305,-0.0402339667415927,
-0.0118573909555889));
#46074=CARTESIAN_POINT('Ctrl Pts',(-0.0109885016422904,-0.0402123400312024,
-0.0122466717426135));
#46075=CARTESIAN_POINT('Ctrl Pts',(-0.0110112352664487,-0.04020124024701,
-0.0124464678580768));
#46076=CARTESIAN_POINT('Ctrl Pts',(-0.0111313730440562,-0.0401805319503916,
-0.012819217197209));
#46077=CARTESIAN_POINT('Ctrl Pts',(-0.0112251248681721,-0.0401716818652295,
-0.0129893326753298));
#46078=CARTESIAN_POINT('Ctrl Pts',(-0.0114727097220533,-0.0401515313486256,
-0.0132859217269655));
#46079=CARTESIAN_POINT('Ctrl Pts',(-0.0116246004946155,-0.0401407980247833,
-0.0134092388500089));
#46080=CARTESIAN_POINT('Ctrl Pts',(-0.0119712889551903,-0.0401189968436632,
-0.013593599342218));
#46081=CARTESIAN_POINT('Ctrl Pts',(-0.0121637008225687,-0.0401081411524129,
-0.0136511370969502));
#46082=CARTESIAN_POINT('Ctrl Pts',(-0.0124077851078071,-0.0400957700688394,
-0.0136737297222342));
#46083=CARTESIAN_POINT('Ctrl Pts',(-0.0124539166169377,-0.0400934915776735,
-0.0136758532865581));
#46084=CARTESIAN_POINT('Ctrl Pts',(-0.0124999999999998,-0.0400912743898722,
-0.0136758532865581));
#46085=CARTESIAN_POINT('Origin',(-0.0125,-0.0332787743898722,-0.0121758532865583));
#46086=CARTESIAN_POINT('',(-0.0124999999999999,-0.0395287743898722,-0.0136758532865581));
#46087=CARTESIAN_POINT('',(-0.0125,-0.0395912743898722,-0.0136758532865581));
#46088=CARTESIAN_POINT('',(-0.0125,-0.0332787743898722,-0.0136758532865583));
#46089=CARTESIAN_POINT('Ctrl Pts',(-0.0124999999999998,-0.0395287743898722,
-0.0136758532865581));
#46090=CARTESIAN_POINT('Ctrl Pts',(-0.0124397722908538,-0.0395316720968796,
-0.0136758532865581));
#46091=CARTESIAN_POINT('Ctrl Pts',(-0.0123794869155727,-0.0395346733294052,
-0.0136722262485745));
#46092=CARTESIAN_POINT('Ctrl Pts',(-0.0121219968180532,-0.0395479289769376,
-0.0136410088687577));
#46093=CARTESIAN_POINT('Ctrl Pts',(-0.0119312721431936,-0.0395588546503147,
-0.0135780294542973));
#46094=CARTESIAN_POINT('Ctrl Pts',(-0.0115903954706135,-0.039580640649201,
-0.0133841492104154));
#46095=CARTESIAN_POINT('Ctrl Pts',(-0.0114424103773941,-0.0395912925013576,
-0.0132570002329958));
#46096=CARTESIAN_POINT('Ctrl Pts',(-0.0112026418538901,-0.0396112656029744,
-0.0129532598395549));
#46097=CARTESIAN_POINT('Ctrl Pts',(-0.0111132317672345,-0.03962023901688,
-0.0127794900004168));
#46098=CARTESIAN_POINT('Ctrl Pts',(-0.0110040333182525,-0.0396411664246257,
-0.0124027966609954));
#46099=CARTESIAN_POINT('Ctrl Pts',(-0.0109871636068316,-0.0396522650049775,
-0.0122030222146618));
#46100=CARTESIAN_POINT('Ctrl Pts',(-0.0110313371454244,-0.0396737694912329,
-0.0118159414620639));
#46101=CARTESIAN_POINT('Ctrl Pts',(-0.0110890781104405,-0.0396839911712235,
-0.0116319512222338));
#46102=CARTESIAN_POINT('Ctrl Pts',(-0.0112741873004969,-0.0397030562170287,
-0.011288780397739));
#46103=CARTESIAN_POINT('Ctrl Pts',(-0.0114024250252582,-0.0397132333722956,
-0.0111342742979425));
#46104=CARTESIAN_POINT('Ctrl Pts',(-0.0117096250808491,-0.03973491050597,
-0.0108859835900327));
#46105=CARTESIAN_POINT('Ctrl Pts',(-0.0118848478870789,-0.039745901334608,
-0.0107938085621011));
#46106=CARTESIAN_POINT('Ctrl Pts',(-0.0122549601010164,-0.0397667625550083,
-0.0106838577867322));
#46107=CARTESIAN_POINT('Ctrl Pts',(-0.0124456633148463,-0.0397758544896276,
-0.0106648507771582));
#46108=CARTESIAN_POINT('Ctrl Pts',(-0.0128329329067826,-0.0397954579958913,
-0.0106998063931913));
#46109=CARTESIAN_POINT('Ctrl Pts',(-0.0130254735586308,-0.0398063076685071,
-0.0107569044158373));
#46110=CARTESIAN_POINT('Ctrl Pts',(-0.0133726179144054,-0.0398281093002484,
-0.0109404914967616));
#46111=CARTESIAN_POINT('Ctrl Pts',(-0.0135248186503528,-0.0398388488330703,
-0.0110634952707375));
#46112=CARTESIAN_POINT('Ctrl Pts',(-0.0137730290862697,-0.0398590134280308,
-0.0113595076033407));
#46113=CARTESIAN_POINT('Ctrl Pts',(-0.0138671274858221,-0.0398678566542454,
-0.0115293340452784));
#46114=CARTESIAN_POINT('Ctrl Pts',(-0.0139881351226471,-0.0398885471754151,
-0.0119017634263324));
#46115=CARTESIAN_POINT('Ctrl Pts',(-0.0140113373792064,-0.0398996466565376,
-0.012101554086537));
#46116=CARTESIAN_POINT('Ctrl Pts',(-0.0139789887328644,-0.0399212823937301,
-0.0124909973560022));
#46117=CARTESIAN_POINT('Ctrl Pts',(-0.0139266718072984,-0.0399316271824345,
-0.0126772035526814));
#46118=CARTESIAN_POINT('Ctrl Pts',(-0.0137516058177497,-0.0399510116243861,
-0.0130261235078094));
#46119=CARTESIAN_POINT('Ctrl Pts',(-0.013628096636719,-0.0399608436849657,
-0.0131842686005688));
#46120=CARTESIAN_POINT('Ctrl Pts',(-0.0133281201988757,-0.0399824329953701,
-0.013441909343706));
#46121=CARTESIAN_POINT('Ctrl Pts',(-0.0131551638916299,-0.0399934642923688,
-0.0135394669240204));
#46122=CARTESIAN_POINT('Ctrl Pts',(-0.0128169677388121,-0.0400128231181185,
-0.013650611731408));
#46123=CARTESIAN_POINT('Ctrl Pts',(-0.0126588938146744,-0.0400211296076493,
-0.0136758532865581));
#46124=CARTESIAN_POINT('Ctrl Pts',(-0.0124999999999999,-0.0400287743898722,
-0.0136758532865581));
#46125=CARTESIAN_POINT('Ctrl Pts',(-0.0124999999999998,-0.0400912743898722,
-0.0136758532865581));
#46126=CARTESIAN_POINT('Ctrl Pts',(-0.012643270042393,-0.0400843813067437,
-0.0136758532865581));
#46127=CARTESIAN_POINT('Ctrl Pts',(-0.0127860199934178,-0.0400769432292705,
-0.013655332665471));
#46128=CARTESIAN_POINT('Ctrl Pts',(-0.0131119931383006,-0.0400585920843435,
-0.0135592934969406));
#46129=CARTESIAN_POINT('Ctrl Pts',(-0.0132873867431685,-0.0400476048159138,
-0.0134675424684249));
#46130=CARTESIAN_POINT('Ctrl Pts',(-0.0135967024168737,-0.0400258116011465,
-0.0132187371992349));
#46131=CARTESIAN_POINT('Ctrl Pts',(-0.0137263197857993,-0.0400155425052295,
-0.0130626793629855));
#46132=CARTESIAN_POINT('Ctrl Pts',(-0.0139118317301532,-0.0399963603319162,
-0.0127174002433472));
#46133=CARTESIAN_POINT('Ctrl Pts',(-0.0139692730889719,-0.0399861315727515,
-0.0125332825783836));
#46134=CARTESIAN_POINT('Ctrl Pts',(-0.0140127915577626,-0.0399646192699105,
-0.0121460611272465));
#46135=CARTESIAN_POINT('Ctrl Pts',(-0.0139955701085837,-0.0399535203560068,
-0.011946280676979));
#46136=CARTESIAN_POINT('Ctrl Pts',(-0.0138857124295479,-0.0399326059177996,
-0.0115698207892499));
#46137=CARTESIAN_POINT('Ctrl Pts',(-0.0137960414682695,-0.0399236418495419,
-0.0113962721629051));
#46138=CARTESIAN_POINT('Ctrl Pts',(-0.0135558045660159,-0.0399036580386168,
-0.0110929574901586));
#46139=CARTESIAN_POINT('Ctrl Pts',(-0.0134075838011624,-0.0398930011048476,
-0.0109660337699312));
#46140=CARTESIAN_POINT('Ctrl Pts',(-0.0130663529960187,-0.0398712137032887,
-0.0107727164054306));
#46141=CARTESIAN_POINT('Ctrl Pts',(-0.0128755232127017,-0.0398602919526901,
-0.0107100602641833));
#46142=CARTESIAN_POINT('Ctrl Pts',(-0.0124891318972407,-0.0398404188604484,
-0.0106638783334612));
#46143=CARTESIAN_POINT('Ctrl Pts',(-0.0122976941481818,-0.039831497093174,
-0.0106774319536756));
#46144=CARTESIAN_POINT('Ctrl Pts',(-0.0119248928036891,-0.0398108018848791,
-0.0107767485825008));
#46145=CARTESIAN_POINT('Ctrl Pts',(-0.0117475906205829,-0.0397998600318385,
-0.0108635589025283));
#46146=CARTESIAN_POINT('Ctrl Pts',(-0.0114337693742506,-0.0397781312888341,
-0.0111022393075453));
#46147=CARTESIAN_POINT('Ctrl Pts',(-0.011301035805563,-0.0397675625902032,
-0.0112528111734217));
#46148=CARTESIAN_POINT('Ctrl Pts',(-0.0111061596572095,-0.0397488264073279,
-0.0115897783668008));
#46149=CARTESIAN_POINT('Ctrl Pts',(-0.0110430381314342,-0.0397387448591258,
-0.0117713848399931));
#46150=CARTESIAN_POINT('Ctrl Pts',(-0.0109871330632712,-0.0397173852783954,
-0.0121558572931412));
#46151=CARTESIAN_POINT('Ctrl Pts',(-0.0109976930687457,-0.039706298373389,
-0.0123554215832577));
#46152=CARTESIAN_POINT('Ctrl Pts',(-0.0110949915117192,-0.0396851421175358,
-0.0127362341886165));
#46153=CARTESIAN_POINT('Ctrl Pts',(-0.0111797045151038,-0.0396759592379689,
-0.0129140176159246));
#46154=CARTESIAN_POINT('Ctrl Pts',(-0.0114110754907633,-0.0396561797995405,
-0.0132253311141067));
#46155=CARTESIAN_POINT('Ctrl Pts',(-0.0115548035822409,-0.0396456232140526,
-0.0133564238347563));
#46156=CARTESIAN_POINT('Ctrl Pts',(-0.0118904751661538,-0.0396237905618976,
-0.0135609990743401));
#46157=CARTESIAN_POINT('Ctrl Pts',(-0.0120807658386286,-0.0396127197921006,
-0.0136299536740986));
#46158=CARTESIAN_POINT('Ctrl Pts',(-0.0123523154948988,-0.0395985312031165,
-0.0136704050760884));
#46159=CARTESIAN_POINT('Ctrl Pts',(-0.0124261829920253,-0.0395948259123243,
-0.0136758532865581));
#46160=CARTESIAN_POINT('Ctrl Pts',(-0.0124999999999999,-0.0395912743898722,
-0.0136758532865581));
#46161=CARTESIAN_POINT('Origin',(-0.0125,-0.0332787743898722,-0.0121758532865583));
#46162=CARTESIAN_POINT('',(-0.0125,-0.0390287743898722,-0.0136758532865581));
#46163=CARTESIAN_POINT('',(-0.0125,-0.0390912743898722,-0.0136758532865581));
#46164=CARTESIAN_POINT('',(-0.0125,-0.0332787743898722,-0.0136758532865583));
#46165=CARTESIAN_POINT('Ctrl Pts',(-0.0125,-0.0390287743898722,-0.0136758532865581));
#46166=CARTESIAN_POINT('Ctrl Pts',(-0.0124102850117373,-0.0390330908042575,
-0.0136758532865581));
#46167=CARTESIAN_POINT('Ctrl Pts',(-0.012320558270234,-0.0390376313209618,
-0.0136678059602836));
#46168=CARTESIAN_POINT('Ctrl Pts',(-0.01203533333192,-0.0390527935499012,
-0.0136159898032078));
#46169=CARTESIAN_POINT('Ctrl Pts',(-0.0118478964733522,-0.0390638841748649,
-0.0135413774667673));
#46170=CARTESIAN_POINT('Ctrl Pts',(-0.0115196390269793,-0.0390856242050675,
-0.0133272949545545));
#46171=CARTESIAN_POINT('Ctrl Pts',(-0.0113803234820742,-0.0390960754472454,
-0.0131923518382069));
#46172=CARTESIAN_POINT('Ctrl Pts',(-0.0111575496436965,-0.0391156534197134,
-0.0128734004360286));
#46173=CARTESIAN_POINT('Ctrl Pts',(-0.011077693887836,-0.0391251319252631,
-0.0126914176495188));
#46174=CARTESIAN_POINT('Ctrl Pts',(-0.0109927367071867,-0.0391465147559555,
-0.0123065266970562));
#46175=CARTESIAN_POINT('Ctrl Pts',(-0.0109886338190343,-0.0391575784775955,
-0.0121073797075351));
#46176=CARTESIAN_POINT('Ctrl Pts',(-0.0110564826923846,-0.0391787690060196,
-0.011725950195901));
#46177=CARTESIAN_POINT('Ctrl Pts',(-0.0111250641709478,-0.0391884289306804,
-0.0115468311043905));
#46178=CARTESIAN_POINT('Ctrl Pts',(-0.0113300146585407,-0.0392074699993104,
-0.0112163372912574));
#46179=CARTESIAN_POINT('Ctrl Pts',(-0.0114673500864563,-0.0392181454215954,
-0.0110698940278283));
#46180=CARTESIAN_POINT('Ctrl Pts',(-0.0117879424564227,-0.0392399192452917,
-0.0108413186480632));
#46181=CARTESIAN_POINT('Ctrl Pts',(-0.0119672464793475,-0.0392508004521428,
-0.0107601588791299));
#46182=CARTESIAN_POINT('Ctrl Pts',(-0.0123427675174401,-0.0392713174229338,
-0.0106719694479415));
#46183=CARTESIAN_POINT('Ctrl Pts',(-0.0125350535616568,-0.0392801366451525,
-0.0106641799268804));
#46184=CARTESIAN_POINT('Ctrl Pts',(-0.0129218058778295,-0.0393003643275987,
-0.0107225018333852));
#46185=CARTESIAN_POINT('Ctrl Pts',(-0.0131119400693353,-0.0393114365019678,
-0.010791778030731));
#46186=CARTESIAN_POINT('Ctrl Pts',(-0.0134472009486803,-0.0393332644596337,
-0.0109968956298863));
#46187=CARTESIAN_POINT('Ctrl Pts',(-0.0135906831652189,-0.0393438153472172,
-0.0111282090938635));
#46188=CARTESIAN_POINT('Ctrl Pts',(-0.0138215724648837,-0.0393635835830235,
-0.0114399535849478));
#46189=CARTESIAN_POINT('Ctrl Pts',(-0.0139060147553127,-0.0393727808693334,
-0.0116179699168607));
#46190=CARTESIAN_POINT('Ctrl Pts',(-0.0140026259839428,-0.0393939500327153,
-0.0119990148577352));
#46191=CARTESIAN_POINT('Ctrl Pts',(-0.0140128240180074,-0.0394050359398672,
-0.0121985611864688));
#46192=CARTESIAN_POINT('Ctrl Pts',(-0.013956248745159,-0.0394263862253205,
-0.0125828663246282));
#46193=CARTESIAN_POINT('Ctrl Pts',(-0.0138928231002549,-0.0394364421224273,
-0.0127643320341397));
#46194=CARTESIAN_POINT('Ctrl Pts',(-0.0136973858617855,-0.0394551953887276,
-0.0131009423942271));
#46195=CARTESIAN_POINT('Ctrl Pts',(-0.0135643935655737,-0.0394657702792724,
-0.0132512890397871));
#46196=CARTESIAN_POINT('Ctrl Pts',(-0.0132501881407943,-0.0394875020742744,
-0.0134894139001271));
#46197=CARTESIAN_POINT('Ctrl Pts',(-0.0130727702861836,-0.0394984408148763,
-0.0135759118234382));
#46198=CARTESIAN_POINT('Ctrl Pts',(-0.0127582698832516,-0.0395158841726235,
-0.0136591420254606));
#46199=CARTESIAN_POINT('Ctrl Pts',(-0.0126292903182273,-0.0395225539065362,
-0.0136758532865581));
#46200=CARTESIAN_POINT('Ctrl Pts',(-0.0124999999999998,-0.0395287743898722,
-0.0136758532865581));
#46201=CARTESIAN_POINT('Ctrl Pts',(-0.0124999999999999,-0.0395912743898722,
-0.0136758532865581));
#46202=CARTESIAN_POINT('Ctrl Pts',(-0.012616080968727,-0.0395856894416603,
-0.0136758532865581));
#46203=CARTESIAN_POINT('Ctrl Pts',(-0.0127320006990499,-0.0395797380488127,
-0.0136623820065603));
#46204=CARTESIAN_POINT('Ctrl Pts',(-0.0130352221126667,-0.0395631559363599,
-0.0135906208525869));
#46205=CARTESIAN_POINT('Ctrl Pts',(-0.0132144148882381,-0.0395522709514737,
-0.0135091323883231));
#46206=CARTESIAN_POINT('Ctrl Pts',(-0.0135346236164816,-0.0395304991674054,
-0.0132799659482055));
#46207=CARTESIAN_POINT('Ctrl Pts',(-0.0136716958454091,-0.0395198296493871,
-0.0131332793643585));
#46208=CARTESIAN_POINT('Ctrl Pts',(-0.0138760644607809,-0.0395008060819552,
-0.0128024077621056));
#46209=CARTESIAN_POINT('Ctrl Pts',(-0.0139443304909923,-0.0394911240563624,
-0.0126231472833809));
#46210=CARTESIAN_POINT('Ctrl Pts',(-0.0140114946017313,-0.0394699236436718,
-0.0122415398549506));
#46211=CARTESIAN_POINT('Ctrl Pts',(-0.0140070212567482,-0.0394588582824967,
-0.0120423633537985));
#46212=CARTESIAN_POINT('Ctrl Pts',(-0.013921351111115,-0.0394374882375592,
-0.0116577025449237));
#46213=CARTESIAN_POINT('Ctrl Pts',(-0.0138412148809848,-0.0394280288982809,
-0.0114759632715372));
#46214=CARTESIAN_POINT('Ctrl Pts',(-0.0136179473921991,-0.0394084392709806,
-0.0111574473229837));
#46215=CARTESIAN_POINT('Ctrl Pts',(-0.0134783771898,-0.0393979817752759,
-0.0110227201593938));
#46216=CARTESIAN_POINT('Ctrl Pts',(-0.0131496894052637,-0.0393762359278434,
-0.0108091735944673));
#46217=CARTESIAN_POINT('Ctrl Pts',(-0.0129620852800822,-0.0393651461472728,
-0.0107348813704491));
#46218=CARTESIAN_POINT('Ctrl Pts',(-0.0125770224262023,-0.0393446967179505,
-0.0106656503418758));
#46219=CARTESIAN_POINT('Ctrl Pts',(-0.0123838966512107,-0.0393359023193282,
-0.0106681509271087));
#46220=CARTESIAN_POINT('Ctrl Pts',(-0.0120059896027197,-0.039315550867305,
-0.0107462489914163));
#46221=CARTESIAN_POINT('Ctrl Pts',(-0.0118250255834797,-0.0393047328042361,
-0.0108222603862315));
#46222=CARTESIAN_POINT('Ctrl Pts',(-0.0114985868770511,-0.0392829362870622,
-0.0110415265794009));
#46223=CARTESIAN_POINT('Ctrl Pts',(-0.0113572005343832,-0.0392721732215874,
-0.011184108607497));
#46224=CARTESIAN_POINT('Ctrl Pts',(-0.0111431977622291,-0.0392528616647807,
-0.0115086609782096));
#46225=CARTESIAN_POINT('Ctrl Pts',(-0.0110697032319431,-0.0392435098340271,
-0.0116856152917699));
#46226=CARTESIAN_POINT('Ctrl Pts',(-0.0109912787660915,-0.0392224748475099,
-0.0120642450490785));
#46227=CARTESIAN_POINT('Ctrl Pts',(-0.0109896599278592,-0.0392114412748625,
-0.0122628493567319));
#46228=CARTESIAN_POINT('Ctrl Pts',(-0.0110635220924074,-0.0391898643579785,
-0.0126512338606453));
#46229=CARTESIAN_POINT('Ctrl Pts',(-0.0111390114930965,-0.039180055942407,
-0.0128370186377876));
#46230=CARTESIAN_POINT('Ctrl Pts',(-0.011354149385122,-0.0391606595848464,
-0.0131626577503477));
#46231=CARTESIAN_POINT('Ctrl Pts',(-0.011489508880533,-0.039150308105931,
-0.01330086146796));
#46232=CARTESIAN_POINT('Ctrl Pts',(-0.0118110442018891,-0.0391286655421054,
-0.0135230782526652));
#46233=CARTESIAN_POINT('Ctrl Pts',(-0.0119958440066602,-0.0391175663324443,
-0.0136025671493725));
#46234=CARTESIAN_POINT('Ctrl Pts',(-0.01229269653651,-0.03910154681736,
-0.0136651060283512));
#46235=CARTESIAN_POINT('Ctrl Pts',(-0.0123963195413974,-0.0390962627182625,
-0.0136758532865581));
#46236=CARTESIAN_POINT('Ctrl Pts',(-0.0125,-0.0390912743898722,-0.0136758532865581));
#46237=CARTESIAN_POINT('Origin',(-0.0125,-0.0332787743898722,-0.0121758532865583));
#46238=CARTESIAN_POINT('',(-0.0125,-0.0385287743898722,-0.0136758532865581));
#46239=CARTESIAN_POINT('',(-0.0125000000000001,-0.0385912743898721,-0.0136758532865581));
#46240=CARTESIAN_POINT('',(-0.0125,-0.0332787743898722,-0.0136758532865583));
#46241=CARTESIAN_POINT('Ctrl Pts',(-0.0125000000000001,-0.0385287743898722,
-0.0136758532865581));
#46242=CARTESIAN_POINT('Ctrl Pts',(-0.0123794141842183,-0.038534576077639,
-0.0136758532865581));
#46243=CARTESIAN_POINT('Ctrl Pts',(-0.0122590243636787,-0.0385407721431061,
-0.0136613162156284));
#46244=CARTESIAN_POINT('Ctrl Pts',(-0.0119486306014825,-0.0385578286507219,
-0.0135848997079368));
#46245=CARTESIAN_POINT('Ctrl Pts',(-0.0117671804892131,-0.0385689272417041,
-0.0134996312460684));
#46246=CARTESIAN_POINT('Ctrl Pts',(-0.0114540318222995,-0.0385904319664484,
-0.01326785055669));
#46247=CARTESIAN_POINT('Ctrl Pts',(-0.0113235541708813,-0.0386006538620198,
-0.0131258562376278));
#46248=CARTESIAN_POINT('Ctrl Pts',(-0.0111188968888253,-0.0386197194780385,
-0.012793970871615));
#46249=CARTESIAN_POINT('Ctrl Pts',(-0.0110492001005163,-0.0386298960133832,
-0.0126056640633596));
#46250=CARTESIAN_POINT('Ctrl Pts',(-0.0109877544422508,-0.0386515730342179,
-0.0122154776883335));
#46251=CARTESIAN_POINT('Ctrl Pts',(-0.0109955302872684,-0.0386625639380715,
-0.0120176414189686));
#46252=CARTESIAN_POINT('Ctrl Pts',(-0.0110853483635358,-0.0386834254352273,
-0.0116421344701649));
#46253=CARTESIAN_POINT('Ctrl Pts',(-0.0111642308846139,-0.0386925177159721,
-0.0114674735719249));
#46254=CARTESIAN_POINT('Ctrl Pts',(-0.0113881225163157,-0.038712120765372,
-0.0111495554750252));
#46255=CARTESIAN_POINT('Ctrl Pts',(-0.0115338344365946,-0.0387229703092475,
-0.0110113523446981));
#46256=CARTESIAN_POINT('Ctrl Pts',(-0.0118663882652761,-0.0387447719493325,
-0.0108024934291675));
#46257=CARTESIAN_POINT('Ctrl Pts',(-0.0120490105383213,-0.038755511613758,
-0.0107321765653561));
#46258=CARTESIAN_POINT('Ctrl Pts',(-0.0124294659781935,-0.0387756765080802,
-0.0106652085216324));
#46259=CARTESIAN_POINT('Ctrl Pts',(-0.0126235875562038,-0.0387845195932171,
-0.0106686206804526));
#46260=CARTESIAN_POINT('Ctrl Pts',(-0.0130066280278391,-0.0388052097357883,
-0.0107500202547862));
#46261=CARTESIAN_POINT('Ctrl Pts',(-0.0131912578178942,-0.038816309209822,
-0.0108298131430346));
#46262=CARTESIAN_POINT('Ctrl Pts',(-0.0135123635693991,-0.0388379451378713,
-0.0110525350766006));
#46263=CARTESIAN_POINT('Ctrl Pts',(-0.0136474716068829,-0.0388482901131671,
-0.0111909402018134));
#46264=CARTESIAN_POINT('Ctrl Pts',(-0.0138621260050081,-0.0388676748870375,
-0.0115169997375278));
#46265=CARTESIAN_POINT('Ctrl Pts',(-0.0139373370580137,-0.0388775062857149,
-0.0117030274117301));
#46266=CARTESIAN_POINT('Ctrl Pts',(-0.0140104925159708,-0.0388990952514589,
-0.0120916287951207));
#46267=CARTESIAN_POINT('Ctrl Pts',(-0.0140085120609981,-0.0389101266123352,
-0.0122901932908941));
#46268=CARTESIAN_POINT('Ctrl Pts',(-0.0139294190175121,-0.038931151586005,
-0.0126686428169504));
#46269=CARTESIAN_POINT('Ctrl Pts',(-0.0138556111572235,-0.0389404860779281,
-0.0128454614561909));
#46270=CARTESIAN_POINT('Ctrl Pts',(-0.0136410319840247,-0.0389598147421072,
-0.0131696313364146));
#46271=CARTESIAN_POINT('Ctrl Pts',(-0.0134993905740551,-0.0389705831167817,
-0.0133119627061757));
#46272=CARTESIAN_POINT('Ctrl Pts',(-0.0131725875188633,-0.0389923804997031,
-0.013530628995685));
#46273=CARTESIAN_POINT('Ctrl Pts',(-0.0129915223515988,-0.0390031942634895,
-0.0136063104228091));
#46274=CARTESIAN_POINT('Ctrl Pts',(-0.0127017552483669,-0.0390187847025531,
-0.0136656748839404));
#46275=CARTESIAN_POINT('Ctrl Pts',(-0.0126008988146715,-0.0390239198933879,
-0.0136758532865581));
#46276=CARTESIAN_POINT('Ctrl Pts',(-0.0125,-0.0390287743898722,-0.0136758532865581));
#46277=CARTESIAN_POINT('Ctrl Pts',(-0.0125,-0.0390912743898722,-0.0136758532865581));
#46278=CARTESIAN_POINT('Ctrl Pts',(-0.0125877964667036,-0.0390870502803984,
-0.0136758532865581));
#46279=CARTESIAN_POINT('Ctrl Pts',(-0.0126756132986267,-0.0390826111114244,
-0.0136681464181381));
#46280=CARTESIAN_POINT('Ctrl Pts',(-0.0129533820634803,-0.0390678757946181,
-0.0136187846265947));
#46281=CARTESIAN_POINT('Ctrl Pts',(-0.0131359171196588,-0.0390571315460259,
-0.0135481516687388));
#46282=CARTESIAN_POINT('Ctrl Pts',(-0.0134681410692972,-0.0390353296470555,
-0.0133387120660686));
#46283=CARTESIAN_POINT('Ctrl Pts',(-0.0136136171138924,-0.0390244846183957,
-0.0132002629348385));
#46284=CARTESIAN_POINT('Ctrl Pts',(-0.0138369629638526,-0.0390048975436701,
-0.0128819746045067));
#46285=CARTESIAN_POINT('Ctrl Pts',(-0.0139155473163728,-0.0389957930392524,
-0.0127071889753984));
#46286=CARTESIAN_POINT('Ctrl Pts',(-0.0140047407173374,-0.038974921874698,
-0.0123315080134204));
#46287=CARTESIAN_POINT('Ctrl Pts',(-0.0140121793945736,-0.0389639283573359,
-0.0121336247009018));
#46288=CARTESIAN_POINT('Ctrl Pts',(-0.0139497766392526,-0.0389421607788429,
-0.0117418082880286));
#46289=CARTESIAN_POINT('Ctrl Pts',(-0.0138788071942519,-0.0389319518037048,
-0.0115520760702422));
#46290=CARTESIAN_POINT('Ctrl Pts',(-0.0136714681141962,-0.0389127435133528,
-0.0112196994386224));
#46291=CARTESIAN_POINT('Ctrl Pts',(-0.0135401761026448,-0.0389024995235825,
-0.0110783202415268));
#46292=CARTESIAN_POINT('Ctrl Pts',(-0.013225621670663,-0.0388809705086359,
-0.0108480999613873));
#46293=CARTESIAN_POINT('Ctrl Pts',(-0.0130436057320444,-0.0388698709869924,
-0.0107637780356961));
#46294=CARTESIAN_POINT('Ctrl Pts',(-0.0126623790169372,-0.0388489847068865,
-0.0106721759916537));
#46295=CARTESIAN_POINT('Ctrl Pts',(-0.012467377748664,-0.038840040025568,
-0.0106637870047411));
#46296=CARTESIAN_POINT('Ctrl Pts',(-0.0120848733994664,-0.0388200330567339,
-0.0107215209158405));
#46297=CARTESIAN_POINT('Ctrl Pts',(-0.0119010131213935,-0.0388093652043643,
-0.0107871082580299));
#46298=CARTESIAN_POINT('Ctrl Pts',(-0.0115636563115328,-0.0387875749787294,
-0.0109872372459273));
#46299=CARTESIAN_POINT('Ctrl Pts',(-0.0114144740244839,-0.0387766618409924,
-0.0111217189037022));
#46300=CARTESIAN_POINT('Ctrl Pts',(-0.011182456665273,-0.0387568225883833,
-0.0114340661432391));
#46301=CARTESIAN_POINT('Ctrl Pts',(-0.0110991208743787,-0.0387478832409401,
-0.0116068939673372));
#46302=CARTESIAN_POINT('Ctrl Pts',(-0.0110000573294581,-0.0387271668939019,
-0.0119797882140237));
#46303=CARTESIAN_POINT('Ctrl Pts',(-0.0109872994414402,-0.0387162183877965,
-0.0121768613239213));
#46304=CARTESIAN_POINT('Ctrl Pts',(-0.0110385688249589,-0.0386944898572231,
-0.0125679748742433));
#46305=CARTESIAN_POINT('Ctrl Pts',(-0.0111033523870144,-0.0386839675002031,
-0.01275796594061));
#46306=CARTESIAN_POINT('Ctrl Pts',(-0.0112990288784539,-0.0386652033326514,
-0.0130945543474498));
#46307=CARTESIAN_POINT('Ctrl Pts',(-0.0114253717544253,-0.038655096449513,
-0.0132395698600731));
#46308=CARTESIAN_POINT('Ctrl Pts',(-0.0117313428234367,-0.0386337227421488,
-0.0134790658880104));
#46309=CARTESIAN_POINT('Ctrl Pts',(-0.0119098782540256,-0.0386226337802118,
-0.0135690360810097));
#46310=CARTESIAN_POINT('Ctrl Pts',(-0.0122310551597517,-0.0386047175243793,
-0.0136577265720446));
#46311=CARTESIAN_POINT('Ctrl Pts',(-0.0123653456229713,-0.0385977529516076,
-0.0136758532865581));
#46312=CARTESIAN_POINT('Ctrl Pts',(-0.0125000000000002,-0.0385912743898721,
-0.0136758532865581));
#46313=CARTESIAN_POINT('Origin',(-0.0125,-0.0332787743898722,-0.0121758532865583));
#46314=CARTESIAN_POINT('',(-0.0125000000000001,-0.0380287743898722,-0.0136758532865581));
#46315=CARTESIAN_POINT('',(-0.0125000000000001,-0.0380912743898722,-0.0136758532865581));
#46316=CARTESIAN_POINT('',(-0.0125,-0.0332787743898722,-0.0136758532865583));
#46317=CARTESIAN_POINT('Ctrl Pts',(-0.0125000000000002,-0.0380287743898722,
-0.0136758532865581));
#46318=CARTESIAN_POINT('Ctrl Pts',(-0.0123468034371259,-0.03803614506294,
-0.0136758532865582));
#46319=CARTESIAN_POINT('Ctrl Pts',(-0.0121942736987196,-0.0380441354069111,
-0.0136523901601837));
#46320=CARTESIAN_POINT('Ctrl Pts',(-0.0118596124296688,-0.0380631766785471,
-0.0135465547026092));
#46321=CARTESIAN_POINT('Ctrl Pts',(-0.0116850882356659,-0.0380742404504398,
-0.0134505436856338));
#46322=CARTESIAN_POINT('Ctrl Pts',(-0.0113886699720512,-0.0380954312788031,
-0.0132010853574274));
#46323=CARTESIAN_POINT('Ctrl Pts',(-0.0112678305352291,-0.0381050918695822,
-0.0130521386517754));
#46324=CARTESIAN_POINT('Ctrl Pts',(-0.0110840709912425,-0.0381241324077053,
-0.0127094089655602));
#46325=CARTESIAN_POINT('Ctrl Pts',(-0.0110259047331901,-0.0381348076514243,
-0.0125172545786196));
#46326=CARTESIAN_POINT('Ctrl Pts',(-0.0109882274892282,-0.0381565814142957,
-0.0121253268469331));
#46327=CARTESIAN_POINT('Ctrl Pts',(-0.0110075827607697,-0.0381674627362096,
-0.0119294630524846));
#46328=CARTESIAN_POINT('Ctrl Pts',(-0.0111189496812055,-0.0381879800246486,
-0.0115601518605821));
#46329=CARTESIAN_POINT('Ctrl Pts',(-0.0112083371616353,-0.0381967993584789,
-0.011389728754414));
#46330=CARTESIAN_POINT('Ctrl Pts',(-0.0114522049126026,-0.0382170266075629,
-0.0110839391223943));
#46331=CARTESIAN_POINT('Ctrl Pts',(-0.0116072608860987,-0.0382280987398141,
-0.0109539071854659));
#46332=CARTESIAN_POINT('Ctrl Pts',(-0.0119525203723629,-0.038249926840854,
-0.0107661025200344));
#46333=CARTESIAN_POINT('Ctrl Pts',(-0.0121379802140337,-0.0382604779017553,
-0.0107074901961218));
#46334=CARTESIAN_POINT('Ctrl Pts',(-0.0125233994980509,-0.0382802464777539,
-0.010663387242309));
#46335=CARTESIAN_POINT('Ctrl Pts',(-0.0127197852926541,-0.0382894433229697,
-0.0106792555844373));
#46336=CARTESIAN_POINT('Ctrl Pts',(-0.0130980898374368,-0.0383106120949194,
-0.0107860886823309));
#46337=CARTESIAN_POINT('Ctrl Pts',(-0.0132760070182737,-0.0383216980328853,
-0.010877020852352));
#46338=CARTESIAN_POINT('Ctrl Pts',(-0.0135805519682038,-0.0383430486008001,
-0.0111181539708168));
#46339=CARTESIAN_POINT('Ctrl Pts',(-0.0137060013753424,-0.0383531052730338,
-0.011263809183469));
#46340=CARTESIAN_POINT('Ctrl Pts',(-0.013899813786559,-0.0383718580207817,
-0.01160135864293));
#46341=CARTESIAN_POINT('Ctrl Pts',(-0.013963531508504,-0.0383824327237375,
-0.011791703296134));
#46342=CARTESIAN_POINT('Ctrl Pts',(-0.014012671420935,-0.0384041644269998,
-0.0121828739548556));
#46343=CARTESIAN_POINT('Ctrl Pts',(-0.0139988818636063,-0.0384151032625681,
-0.0123797729950841));
#46344=CARTESIAN_POINT('Ctrl Pts',(-0.0138978995332542,-0.0384357890048659,
-0.0127521163564446));
#46345=CARTESIAN_POINT('Ctrl Pts',(-0.0138136297020046,-0.0384447032789115,
-0.0129245666781789));
#46346=CARTESIAN_POINT('Ctrl Pts',(-0.0135799148579252,-0.0384645914793258,
-0.0132357359086626));
#46347=CARTESIAN_POINT('Ctrl Pts',(-0.0134300176507454,-0.0384755170339867,
-0.0133694262977071));
#46348=CARTESIAN_POINT('Ctrl Pts',(-0.0130916835139492,-0.0384973030764192,
-0.0135677119104125));
#46349=CARTESIAN_POINT('Ctrl Pts',(-0.012907579061836,-0.0385079550833858,
-0.0136323058962518));
#46350=CARTESIAN_POINT('Ctrl Pts',(-0.0126444967607305,-0.038521677422535,
-0.013670638193534));
#46351=CARTESIAN_POINT('Ctrl Pts',(-0.0125722202694161,-0.0385252996905398,
-0.0136758532865581));
#46352=CARTESIAN_POINT('Ctrl Pts',(-0.0125000000000001,-0.0385287743898722,
-0.0136758532865581));
#46353=CARTESIAN_POINT('Ctrl Pts',(-0.0125000000000002,-0.0385912743898721,
-0.0136758532865581));
#46354=CARTESIAN_POINT('Ctrl Pts',(-0.0125594873863622,-0.0385884123016614,
-0.0136758532865581));
#46355=CARTESIAN_POINT('Ctrl Pts',(-0.0126190362728254,-0.0385854489647548,
-0.0136723148548114));
#46356=CARTESIAN_POINT('Ctrl Pts',(-0.0128698073234571,-0.03857254964562,
-0.013642287566719));
#46357=CARTESIAN_POINT('Ctrl Pts',(-0.0130550497567754,-0.0385619806919748,
-0.0135826545417134));
#46358=CARTESIAN_POINT('Ctrl Pts',(-0.013399470622655,-0.0385401379867543,
-0.0133928715926655));
#46359=CARTESIAN_POINT('Ctrl Pts',(-0.0135538922728016,-0.0385290704095098,
-0.0132619049557047));
#46360=CARTESIAN_POINT('Ctrl Pts',(-0.0137960248429441,-0.0385088883780659,
-0.0129547377373805));
#46361=CARTESIAN_POINT('Ctrl Pts',(-0.0138844117973256,-0.0385000560761349,
-0.0127839236392865));
#46362=CARTESIAN_POINT('Ctrl Pts',(-0.0139937657294113,-0.0384795057647236,
-0.0124140180338837));
#46363=CARTESIAN_POINT('Ctrl Pts',(-0.0140120447189885,-0.0384686126132817,
-0.0122179413079291));
#46364=CARTESIAN_POINT('Ctrl Pts',(-0.0139721430713558,-0.0384468455456825,
-0.0118261340911449));
#46365=CARTESIAN_POINT('Ctrl Pts',(-0.0139128954156917,-0.0384361890881392,
-0.0116343178553643));
#46366=CARTESIAN_POINT('Ctrl Pts',(-0.0137271825090755,-0.0384172039469478,
-0.0112925853139198));
#46367=CARTESIAN_POINT('Ctrl Pts',(-0.0136054562112809,-0.0384074724867839,
-0.0111442784519007));
#46368=CARTESIAN_POINT('Ctrl Pts',(-0.0133074675371577,-0.0383862504485875,
-0.010896416600494));
#46369=CARTESIAN_POINT('Ctrl Pts',(-0.0131322781585097,-0.0383751816197932,
-0.0108013756686641));
#46370=CARTESIAN_POINT('Ctrl Pts',(-0.0127559744500297,-0.0383538397431168,
-0.0106848452504786));
#46371=CARTESIAN_POINT('Ctrl Pts',(-0.0125586701070593,-0.0383444215515382,
-0.0106641750728909));
#46372=CARTESIAN_POINT('Ctrl Pts',(-0.0121714806461621,-0.03832480637397,
-0.0106996896469178));
#46373=CARTESIAN_POINT('Ctrl Pts',(-0.0119851516068347,-0.0383143352349756,
-0.0107539192876731));
#46374=CARTESIAN_POINT('Ctrl Pts',(-0.0116364222186638,-0.0382925768265017,
-0.0109332049743318));
#46375=CARTESIAN_POINT('Ctrl Pts',(-0.0114787086991418,-0.0382814890247829,
-0.0110591980073559));
#46376=CARTESIAN_POINT('Ctrl Pts',(-0.0112274347351725,-0.0382610706184389,
-0.0113590413635251));
#46377=CARTESIAN_POINT('Ctrl Pts',(-0.011133746819209,-0.038252276689046,
-0.0115278119014317));
#46378=CARTESIAN_POINT('Ctrl Pts',(-0.0110138243780798,-0.0382319017134448,
-0.0118945614622528));
#46379=CARTESIAN_POINT('Ctrl Pts',(-0.0109899111987811,-0.038221074298395,
-0.01208945493315));
#46380=CARTESIAN_POINT('Ctrl Pts',(-0.0110181266666995,-0.0381992799340672,
-0.0124817534910504));
#46381=CARTESIAN_POINT('Ctrl Pts',(-0.0110716710870686,-0.0381885286786585,
-0.0126752760884084));
#46382=CARTESIAN_POINT('Ctrl Pts',(-0.0112471031745442,-0.0381692548532336,
-0.0130222049460577));
#46383=CARTESIAN_POINT('Ctrl Pts',(-0.0113642073769202,-0.0381598638672979,
-0.0131738826292774));
#46384=CARTESIAN_POINT('Ctrl Pts',(-0.0116539785569142,-0.0381388068708262,
-0.0134300360959381));
#46385=CARTESIAN_POINT('Ctrl Pts',(-0.0118256383976094,-0.0381277685483548,
-0.013530092139203));
#46386=CARTESIAN_POINT('Ctrl Pts',(-0.0121690566623018,-0.0381079616211234,
-0.0136483236368381));
#46387=CARTESIAN_POINT('Ctrl Pts',(-0.0123340617498559,-0.0380992580976547,
-0.0136758532865582));
#46388=CARTESIAN_POINT('Ctrl Pts',(-0.0125000000000002,-0.0380912743898722,
-0.0136758532865581));
#46389=CARTESIAN_POINT('Origin',(-0.0125,-0.0332787743898722,-0.0121758532865583));
#46390=CARTESIAN_POINT('',(-0.0125,-0.0375287743898722,-0.0136758532865582));
#46391=CARTESIAN_POINT('',(-0.0124999999604478,-0.0375912743936781,-0.0136758532865582));
#46392=CARTESIAN_POINT('',(-0.0125,-0.0332787743898722,-0.0136758532865583));
#46393=CARTESIAN_POINT('Ctrl Pts',(-0.0125,-0.0375287743898722,-0.0136758532865582));
#46394=CARTESIAN_POINT('Ctrl Pts',(-0.0123159669085782,-0.0375376286861116,
-0.0136758532865582));
#46395=CARTESIAN_POINT('Ctrl Pts',(-0.012133343711675,-0.0375473558415515,
-0.0136419883463988));
#46396=CARTESIAN_POINT('Ctrl Pts',(-0.0117782621206025,-0.0375682353262687,
-0.0135053462531493));
#46397=CARTESIAN_POINT('Ctrl Pts',(-0.0116108124726789,-0.0375792263096031,
-0.013399702151021));
#46398=CARTESIAN_POINT('Ctrl Pts',(-0.011330508950688,-0.0376000880992964,
-0.0131341776636912));
#46399=CARTESIAN_POINT('Ctrl Pts',(-0.011218681662231,-0.0376091807461351,
-0.0129785388738239));
#46400=CARTESIAN_POINT('Ctrl Pts',(-0.0110552843729969,-0.037628783312591,
-0.012625692677619));
#46401=CARTESIAN_POINT('Ctrl Pts',(-0.0110084428972583,-0.0376396327203533,
-0.0124304033378973));
#46402=CARTESIAN_POINT('Ctrl Pts',(-0.0109938224843649,-0.0376614343692014,
-0.0120379736586325));
#46403=CARTESIAN_POINT('Ctrl Pts',(-0.011024227833506,-0.037672174172713,
-0.0118446571954231));
#46404=CARTESIAN_POINT('Ctrl Pts',(-0.0111564412509518,-0.0376923393834609,
-0.0114816834019601));
#46405=CARTESIAN_POINT('Ctrl Pts',(-0.0112564475347326,-0.0377011823196947,
-0.0113152717612241));
#46406=CARTESIAN_POINT('Ctrl Pts',(-0.0115184458539515,-0.0377218720620583,
-0.0110242354365176));
#46407=CARTESIAN_POINT('Ctrl Pts',(-0.0116798580306075,-0.0377329715285701,
-0.0109042287330237));
#46408=CARTESIAN_POINT('Ctrl Pts',(-0.0120332870355569,-0.037754607658306,
-0.0107374850559715));
#46409=CARTESIAN_POINT('Ctrl Pts',(-0.0122207019429658,-0.0377649528308088,
-0.0106896709875991));
#46410=CARTESIAN_POINT('Ctrl Pts',(-0.01261040128369,-0.0377843379555074,
-0.0106667855562598));
#46411=CARTESIAN_POINT('Ctrl Pts',(-0.0128091093455027,-0.0377941686547767,
-0.010694653731616));
#46412=CARTESIAN_POINT('Ctrl Pts',(-0.0131822307660401,-0.0378157572561895,
-0.0108255781247143));
#46413=CARTESIAN_POINT('Ctrl Pts',(-0.0133532089612384,-0.0378267886845521,
-0.0109265666246989));
#46414=CARTESIAN_POINT('Ctrl Pts',(-0.0136414241920234,-0.0378478139616304,
-0.0111842731762835));
#46415=CARTESIAN_POINT('Ctrl Pts',(-0.0137576579952084,-0.0378571489746186,
-0.0113365958119946));
#46416=CARTESIAN_POINT('Ctrl Pts',(-0.013931126525451,-0.0378764771209369,
-0.0116845024457244));
#46417=CARTESIAN_POINT('Ctrl Pts',(-0.0139835788430444,-0.0378872453353139,
-0.0118783303045099));
#46418=CARTESIAN_POINT('Ctrl Pts',(-0.0140095691307863,-0.0379090426930424,
-0.0122706827436235));
#46419=CARTESIAN_POINT('Ctrl Pts',(-0.0139845887701048,-0.0379198565875163,
-0.0124653328441524));
#46420=CARTESIAN_POINT('Ctrl Pts',(-0.0138626551541139,-0.037940197651112,
-0.012831471988875));
#46421=CARTESIAN_POINT('Ctrl Pts',(-0.0137679446581723,-0.0379489926709229,
-0.0129998559735247));
#46422=CARTESIAN_POINT('Ctrl Pts',(-0.0135149225571613,-0.0379694557490269,
-0.0132982796508804));
#46423=CARTESIAN_POINT('Ctrl Pts',(-0.013356593807172,-0.0379805463489167,
-0.0134233078076331));
#46424=CARTESIAN_POINT('Ctrl Pts',(-0.0130070717177654,-0.0380022865563384,
-0.0136005652575964));
#46425=CARTESIAN_POINT('Ctrl Pts',(-0.0128205515789315,-0.0380127379884413,
-0.0136537544562052));
#46426=CARTESIAN_POINT('Ctrl Pts',(-0.0125860660101643,-0.0380245821562937,
-0.0136740035801463));
#46427=CARTESIAN_POINT('Ctrl Pts',(-0.0125430091945582,-0.0380267051090342,
-0.0136758532865581));
#46428=CARTESIAN_POINT('Ctrl Pts',(-0.0125000000000002,-0.0380287743898722,
-0.0136758532865581));
#46429=CARTESIAN_POINT('Ctrl Pts',(-0.0125000000000002,-0.0380912743898722,
-0.0136758532865581));
#46430=CARTESIAN_POINT('Ctrl Pts',(-0.0125318766297121,-0.0380897407248101,
-0.0136758532865581));
#46431=CARTESIAN_POINT('Ctrl Pts',(-0.0125637850048779,-0.0380881773075196,
-0.0136748371910692));
#46432=CARTESIAN_POINT('Ctrl Pts',(-0.0127870750712986,-0.0380770378262157,
-0.0136605656039966));
#46433=CARTESIAN_POINT('Ctrl Pts',(-0.0129743333509333,-0.0380666720839346,
-0.0136117397363397));
#46434=CARTESIAN_POINT('Ctrl Pts',(-0.0133270509590668,-0.0380450150808707,
-0.0134430124440513));
#46435=CARTESIAN_POINT('Ctrl Pts',(-0.0134878948346635,-0.0380339165703657,
-0.0133220558304902));
#46436=CARTESIAN_POINT('Ctrl Pts',(-0.0137482102722622,-0.0380132689682407,
-0.0130296217179064));
#46437=CARTESIAN_POINT('Ctrl Pts',(-0.0138472176633938,-0.0380044404119239,
-0.0128628416834866));
#46438=CARTESIAN_POINT('Ctrl Pts',(-0.0139775095350967,-0.0379842420100572,
-0.0124992704498853));
#46439=CARTESIAN_POINT('Ctrl Pts',(-0.0140069048435702,-0.0379734877277754,
-0.0123056933688139));
#46440=CARTESIAN_POINT('Ctrl Pts',(-0.0139901601365045,-0.0379516854820057,
-0.0119132529449597));
#46441=CARTESIAN_POINT('Ctrl Pts',(-0.0139422664741222,-0.0379408505493004,
-0.0117182241562649));
#46442=CARTESIAN_POINT('Ctrl Pts',(-0.0137769821896819,-0.037921298859816,
-0.0113662937455464));
#46443=CARTESIAN_POINT('Ctrl Pts',(-0.0136643363738046,-0.0379121664429356,
-0.0112112774403091));
#46444=CARTESIAN_POINT('Ctrl Pts',(-0.0133825592776287,-0.0378912739307356,
-0.0109471992480974));
#46445=CARTESIAN_POINT('Ctrl Pts',(-0.0132144446938143,-0.0378802747382287,
-0.0108424113185088));
#46446=CARTESIAN_POINT('Ctrl Pts',(-0.0128435550131623,-0.0378585312368616,
-0.0107020450401858));
#46447=CARTESIAN_POINT('Ctrl Pts',(-0.0126439075086321,-0.0378483773262782,
-0.0106694026924819));
#46448=CARTESIAN_POINT('Ctrl Pts',(-0.0122526357967572,-0.0378291446963842,
-0.0106840748841354));
#46449=CARTESIAN_POINT('Ctrl Pts',(-0.0120646357701901,-0.0378188865762998,
-0.0107277416093345));
#46450=CARTESIAN_POINT('Ctrl Pts',(-0.0117084066167368,-0.0377973421874111,
-0.0108863326164094));
#46451=CARTESIAN_POINT('Ctrl Pts',(-0.011544723362927,-0.0377862422388562,
-0.0110024230524411));
#46452=CARTESIAN_POINT('Ctrl Pts',(-0.0112758587586708,-0.0377653823997635,
-0.0112876901048509));
#46453=CARTESIAN_POINT('Ctrl Pts',(-0.0111717434886811,-0.0377564548055052,
-0.0114526058051654));
#46454=CARTESIAN_POINT('Ctrl Pts',(-0.0110317145148108,-0.0377364262054051,
-0.0118131206069678));
#46455=CARTESIAN_POINT('Ctrl Pts',(-0.0109972217211189,-0.037725748241553,
-0.0120053239563055));
#46456=CARTESIAN_POINT('Ctrl Pts',(-0.011003210473034,-0.0377039556384248,
-0.012397590812612));
#46457=CARTESIAN_POINT('Ctrl Pts',(-0.0110457582473621,-0.0376930507076776,
-0.0125938795660615));
#46458=CARTESIAN_POINT('Ctrl Pts',(-0.0112014588956732,-0.037673243245692,
-0.0129504138818026));
#46459=CARTESIAN_POINT('Ctrl Pts',(-0.01130997920573,-0.0376642863833723,
-0.0131085979982951));
#46460=CARTESIAN_POINT('Ctrl Pts',(-0.0115843144457518,-0.0376435502570075,
-0.0133799359734051));
#46461=CARTESIAN_POINT('Ctrl Pts',(-0.0117490362736719,-0.0376325956333979,
-0.0134889958482765));
#46462=CARTESIAN_POINT('Ctrl Pts',(-0.0121109673025152,-0.0376110523351543,
-0.0136376716542548));
#46463=CARTESIAN_POINT('Ctrl Pts',(-0.0123045998806578,-0.0376006755826408,
-0.0136758532813938));
#46464=CARTESIAN_POINT('Ctrl Pts',(-0.0124999999603558,-0.0375912743917796,
-0.0136758532865582));
#46465=CARTESIAN_POINT('Origin',(-0.0125,-0.0332787743898722,-0.0121758532865583));
#46466=CARTESIAN_POINT('',(-0.0125,-0.0370287743898722,-0.0136758532865582));
#46467=CARTESIAN_POINT('',(-0.0124999999999999,-0.0370912743898722,-0.0136758532865582));
#46468=CARTESIAN_POINT('',(-0.0125,-0.0332787743898722,-0.0136758532865583));
#46469=CARTESIAN_POINT('Ctrl Pts',(-0.0124999999999999,-0.0370287743898722,
-0.0136758532865582));
#46470=CARTESIAN_POINT('Ctrl Pts',(-0.0124805219657667,-0.0370297115272312,
-0.0136758532865582));
#46471=CARTESIAN_POINT('Ctrl Pts',(-0.0124610298195439,-0.0370306598821878,
-0.013675473895722));
#46472=CARTESIAN_POINT('Ctrl Pts',(-0.0122503614464783,-0.0370410239320082,
-0.0136672564278871));
#46473=CARTESIAN_POINT('Ctrl Pts',(-0.0120624000233708,-0.0370512883889477,
-0.01362329471275));
#46474=CARTESIAN_POINT('Ctrl Pts',(-0.0117063638989342,-0.037072839630674,
-0.0134641226674579));
#46475=CARTESIAN_POINT('Ctrl Pts',(-0.0115428390887165,-0.037083939727006,
-0.0133477524790992));
#46476=CARTESIAN_POINT('Ctrl Pts',(-0.0112744612341667,-0.0371047876072881,
-0.0130620728686492));
#46477=CARTESIAN_POINT('Ctrl Pts',(-0.0111706390738156,-0.0371137078262836,
-0.0128970514311515));
#46478=CARTESIAN_POINT('Ctrl Pts',(-0.0110311629065429,-0.0371337461738722,
-0.0125363611745579));
#46479=CARTESIAN_POINT('Ctrl Pts',(-0.0109969580789391,-0.0371444286662987,
-0.0123440763108809));
#46480=CARTESIAN_POINT('Ctrl Pts',(-0.0110035567944185,-0.0371662222578953,
-0.011951791662141));
#46481=CARTESIAN_POINT('Ctrl Pts',(-0.0110464089534472,-0.0371771234389558,
-0.0117555704030513));
#46482=CARTESIAN_POINT('Ctrl Pts',(-0.0112026551375385,-0.0371969165177683,
-0.0113992949844256));
#46483=CARTESIAN_POINT('Ctrl Pts',(-0.0113114082349763,-0.0372058816211278,
-0.0112412916348739));
#46484=CARTESIAN_POINT('Ctrl Pts',(-0.0115861642794054,-0.0372266266711798,
-0.0109703612616427));
#46485=CARTESIAN_POINT('Ctrl Pts',(-0.0117510802187798,-0.0372375840203846,
-0.0108615394762437));
#46486=CARTESIAN_POINT('Ctrl Pts',(-0.0121162858873101,-0.0372593035509491,
-0.0107121911490276));
#46487=CARTESIAN_POINT('Ctrl Pts',(-0.012313420021904,-0.0372697542965391,
-0.0106742959283085));
#46488=CARTESIAN_POINT('Ctrl Pts',(-0.0127028546731965,-0.0372885784314582,
-0.0106774441831272));
#46489=CARTESIAN_POINT('Ctrl Pts',(-0.0128915164495543,-0.0372987083579849,
-0.0107153497559918));
#46490=CARTESIAN_POINT('Ctrl Pts',(-0.0132513277654239,-0.0373201088947214,
-0.0108625575982811));
#46491=CARTESIAN_POINT('Ctrl Pts',(-0.0134180109124625,-0.0373312003917612,
-0.0109731478122762));
#46492=CARTESIAN_POINT('Ctrl Pts',(-0.0136963350140692,-0.0373522894961551,
-0.0112502840855021));
#46493=CARTESIAN_POINT('Ctrl Pts',(-0.0138062052478684,-0.0373614019821378,
-0.0114131499473394));
#46494=CARTESIAN_POINT('Ctrl Pts',(-0.0139569437368682,-0.0373812392034485,
-0.0117702199309313));
#46495=CARTESIAN_POINT('Ctrl Pts',(-0.0139969777988742,-0.0373918248627651,
-0.0119607617986294));
#46496=CARTESIAN_POINT('Ctrl Pts',(-0.0140028065907852,-0.0374136808391922,
-0.0123541693743183));
#46497=CARTESIAN_POINT('Ctrl Pts',(-0.0139655282866358,-0.0374247437817464,
-0.0125533023402924));
#46498=CARTESIAN_POINT('Ctrl Pts',(-0.0138186270954199,-0.0374448827113351,
-0.0129158030728906));
#46499=CARTESIAN_POINT('Ctrl Pts',(-0.0137140942408266,-0.0374537297954097,
-0.0130771207993225));
#46500=CARTESIAN_POINT('Ctrl Pts',(-0.0134446521312873,-0.037474490623306,
-0.0133578231799252));
#46501=CARTESIAN_POINT('Ctrl Pts',(-0.0132800878972543,-0.0374855892255531,
-0.013472339243484));
#46502=CARTESIAN_POINT('Ctrl Pts',(-0.0129227921909198,-0.037507094202374,
-0.0136276640923396));
#46503=CARTESIAN_POINT('Ctrl Pts',(-0.0127345839372821,-0.0375173163258038,
-0.0136696742781088));
#46504=CARTESIAN_POINT('Ctrl Pts',(-0.0125290175939898,-0.0375273724361939,
-0.0136756429012426));
#46505=CARTESIAN_POINT('Ctrl Pts',(-0.0125145046942967,-0.0375280765324425,
-0.0136758532865582));
#46506=CARTESIAN_POINT('Ctrl Pts',(-0.0125,-0.0375287743898722,-0.0136758532865582));
#46507=CARTESIAN_POINT('Ctrl Pts',(-0.0124999999603558,-0.0375912743917796,
-0.0136758532865582));
#46508=CARTESIAN_POINT('Ctrl Pts',(-0.0125032493611257,-0.0375911180549098,
-0.013675853286644));
#46509=CARTESIAN_POINT('Ctrl Pts',(-0.0125064992227011,-0.0375909614025844,
-0.0136758427281261));
#46510=CARTESIAN_POINT('Ctrl Pts',(-0.0127004506407383,-0.0375815948927042,
-0.013674582082679));
#46511=CARTESIAN_POINT('Ctrl Pts',(-0.0128891431155838,-0.0375714721149941,
-0.0136369870385509));
#46512=CARTESIAN_POINT('Ctrl Pts',(-0.013249137391045,-0.0375500798720693,
-0.013490394668792));
#46513=CARTESIAN_POINT('Ctrl Pts',(-0.0134159771391333,-0.0375389891306121,
-0.0133801028967398));
#46514=CARTESIAN_POINT('Ctrl Pts',(-0.0136948086964579,-0.037517887901,
-0.0131034090547456));
#46515=CARTESIAN_POINT('Ctrl Pts',(-0.0138049909252382,-0.0375087632650271,
-0.012940653039345));
#46516=CARTESIAN_POINT('Ctrl Pts',(-0.0139563022466104,-0.0374889364163352,
-0.0125837697628913));
#46517=CARTESIAN_POINT('Ctrl Pts',(-0.0139966305884438,-0.0374783559366218,
-0.0123933211280314));
#46518=CARTESIAN_POINT('Ctrl Pts',(-0.0140029748889338,-0.0374568959234863,
-0.0120070408915934));
#46519=CARTESIAN_POINT('Ctrl Pts',(-0.0139686964613012,-0.0374462145860024,
-0.0118147768169018));
#46520=CARTESIAN_POINT('Ctrl Pts',(-0.0138290790375217,-0.0374261787279252,
-0.0114541313715126));
#46521=CARTESIAN_POINT('Ctrl Pts',(-0.013725182016287,-0.0374172566445162,
-0.0112891369530126));
#46522=CARTESIAN_POINT('Ctrl Pts',(-0.013456679799678,-0.037396405707353,
-0.011003562696253));
#46523=CARTESIAN_POINT('Ctrl Pts',(-0.0132931144705065,-0.0373853056461237,
-0.0108872639524797));
#46524=CARTESIAN_POINT('Ctrl Pts',(-0.0129370289480666,-0.037363756150175,
-0.0107282403150346));
#46525=CARTESIAN_POINT('Ctrl Pts',(-0.0127490576199794,-0.0373534933098602,
-0.0106843539543152));
#46526=CARTESIAN_POINT('Ctrl Pts',(-0.0123578682010972,-0.0373342525252803,
-0.0106692456583258));
#46527=CARTESIAN_POINT('Ctrl Pts',(-0.0121582709968624,-0.0373241168536264,
-0.0107016325955487));
#46528=CARTESIAN_POINT('Ctrl Pts',(-0.0117872594786064,-0.0373023814590014,
-0.0108414960022373));
#46529=CARTESIAN_POINT('Ctrl Pts',(-0.0116189904163143,-0.0372913803973135,
-0.0109460836577695));
#46530=CARTESIAN_POINT('Ctrl Pts',(-0.0113368698709304,-0.0372704807421901,
-0.0112098241237532));
#46531=CARTESIAN_POINT('Ctrl Pts',(-0.0112240331471482,-0.0372613387017296,
-0.0113646956731273));
#46532=CARTESIAN_POINT('Ctrl Pts',(-0.0110583098028844,-0.0372417988860765,
-0.0117164123548818));
#46533=CARTESIAN_POINT('Ctrl Pts',(-0.0110101713675452,-0.0372309673701446,
-0.0119113796416551));
#46534=CARTESIAN_POINT('Ctrl Pts',(-0.0109929319633865,-0.0372091650776687,
-0.0123038209062213));
#46535=CARTESIAN_POINT('Ctrl Pts',(-0.0110220918246519,-0.037198407465585,
-0.0124974579237282));
#46536=CARTESIAN_POINT('Ctrl Pts',(-0.0111519362910508,-0.037178201358147,
-0.0128611678576125));
#46537=CARTESIAN_POINT('Ctrl Pts',(-0.0112507117349764,-0.0371693757875885,
-0.0130280337170929));
#46538=CARTESIAN_POINT('Ctrl Pts',(-0.0115106356485122,-0.0371487380142908,
-0.0133207921314658));
#46539=CARTESIAN_POINT('Ctrl Pts',(-0.011671346658901,-0.0371376397731738,
-0.0134419691763465));
#46540=CARTESIAN_POINT('Ctrl Pts',(-0.0120238973594344,-0.0371159780044628,
-0.0136111571243781));
#46541=CARTESIAN_POINT('Ctrl Pts',(-0.0122111184598395,-0.0371056075197522,
-0.0136602181158069));
#46542=CARTESIAN_POINT('Ctrl Pts',(-0.0124350149926267,-0.0370944302790649,
-0.013674798610125));
#46543=CARTESIAN_POINT('Ctrl Pts',(-0.0124675238174636,-0.037092836900933,
-0.0136758532865582));
#46544=CARTESIAN_POINT('Ctrl Pts',(-0.0124999999999998,-0.0370912743898722,
-0.0136758532865582));
#46545=CARTESIAN_POINT('Origin',(-0.0125,-0.0332787743898722,-0.0121758532865583));
#46546=CARTESIAN_POINT('',(-0.0124999999999999,-0.0365287743898722,-0.0136758532865582));
#46547=CARTESIAN_POINT('',(-0.0124999999999999,-0.0365912743898722,-0.0136758532865582));
#46548=CARTESIAN_POINT('',(-0.0125,-0.0332787743898722,-0.0136758532865583));
#46549=CARTESIAN_POINT('Ctrl Pts',(-0.0124999999999997,-0.0365287743898722,
-0.0136758532865582));
#46550=CARTESIAN_POINT('Ctrl Pts',(-0.0124535093249928,-0.0365310111735164,
-0.0136758532865582));
#46551=CARTESIAN_POINT('Ctrl Pts',(-0.012406966782071,-0.0365333104878328,
-0.0136736920202203));
#46552=CARTESIAN_POINT('Ctrl Pts',(-0.0121690102954786,-0.0365453764787804,
-0.0136514690708763));
#46553=CARTESIAN_POINT('Ctrl Pts',(-0.0119827417180806,-0.0365558536735853,
-0.0135969166978075));
#46554=CARTESIAN_POINT('Ctrl Pts',(-0.0116342606295698,-0.0365776175990539,
-0.0134170023317158));
#46555=CARTESIAN_POINT('Ctrl Pts',(-0.0114767391645149,-0.036588704461173,
-0.0132907104761859));
#46556=CARTESIAN_POINT('Ctrl Pts',(-0.0112260082151735,-0.0366091089558757,
-0.0129904274101747));
#46557=CARTESIAN_POINT('Ctrl Pts',(-0.0111326373314,-0.0366179030978354,
-0.0128215365432175));
#46558=CARTESIAN_POINT('Ctrl Pts',(-0.0110133402329699,-0.0366382885824072,
-0.0124545978209253));
#46559=CARTESIAN_POINT('Ctrl Pts',(-0.0109897592263766,-0.0366491201358768,
-0.0122596298584732));
#46560=CARTESIAN_POINT('Ctrl Pts',(-0.0110186665446301,-0.036670913425847,
-0.0118673506390097));
#46561=CARTESIAN_POINT('Ctrl Pts',(-0.0110725501203965,-0.036681659337187,
-0.0116739242348894));
#46562=CARTESIAN_POINT('Ctrl Pts',(-0.0112485922780147,-0.0367009162315802,
-0.0113273001358099));
#46563=CARTESIAN_POINT('Ctrl Pts',(-0.0113659676935067,-0.0367103251945031,
-0.0111758227475674));
#46564=CARTESIAN_POINT('Ctrl Pts',(-0.0116562231892481,-0.0367313920343304,
-0.0109201537795875));
#46565=CARTESIAN_POINT('Ctrl Pts',(-0.0118280943561151,-0.0367424324307944,
-0.0108203891002514));
#46566=CARTESIAN_POINT('Ctrl Pts',(-0.0122019002970657,-0.0367639706655118,
-0.0106924635323234));
#46567=CARTESIAN_POINT('Ctrl Pts',(-0.012400312647355,-0.0367737073272017,
-0.0106661025900807));
#46568=CARTESIAN_POINT('Ctrl Pts',(-0.0127895004386877,-0.0367931406180201,
-0.0106916080312694));
#46569=CARTESIAN_POINT('Ctrl Pts',(-0.0129767087322032,-0.0368035127244026,
-0.0107407495850726));
#46570=CARTESIAN_POINT('Ctrl Pts',(-0.0133292021056302,-0.0368251761186331,
-0.0109100953452619));
#46571=CARTESIAN_POINT('Ctrl Pts',(-0.0134898675216707,-0.0368362742633472,
-0.0110313478913681));
#46572=CARTESIAN_POINT('Ctrl Pts',(-0.0137496572444568,-0.0368569086657708,
-0.0113242173794656));
#46573=CARTESIAN_POINT('Ctrl Pts',(-0.0138483532293192,-0.0368657332442425,
-0.0114911126652259));
#46574=CARTESIAN_POINT('Ctrl Pts',(-0.0139780443210008,-0.0368859419912625,
-0.0118548701115842));
#46575=CARTESIAN_POINT('Ctrl Pts',(-0.0140071234453432,-0.0368967007412299,
-0.0120485276109984));
#46576=CARTESIAN_POINT('Ctrl Pts',(-0.0139897144477836,-0.036918503041693,
-0.0124409690193337));
#46577=CARTESIAN_POINT('Ctrl Pts',(-0.0139414921209812,-0.0369293333822894,
-0.0126359151500683));
#46578=CARTESIAN_POINT('Ctrl Pts',(-0.0137756182890593,-0.0369488691250739,
-0.0129875585201895));
#46579=CARTESIAN_POINT('Ctrl Pts',(-0.0136627160916694,-0.0369580144962438,
-0.0131423804614874));
#46580=CARTESIAN_POINT('Ctrl Pts',(-0.0133804777785285,-0.0369789165991125,
-0.013406005066556));
#46581=CARTESIAN_POINT('Ctrl Pts',(-0.0132121557897494,-0.0369899182978853,
-0.0135105239857802));
#46582=CARTESIAN_POINT('Ctrl Pts',(-0.0128593701136842,-0.037010580977242,
-0.0136433377274973));
#46583=CARTESIAN_POINT('Ctrl Pts',(-0.012680332605693,-0.0370200981333355,
-0.0136758532865582));
#46584=CARTESIAN_POINT('Ctrl Pts',(-0.0124999999999999,-0.0370287743898722,
-0.0136758532865582));
#46585=CARTESIAN_POINT('Ctrl Pts',(-0.0124999999999998,-0.0370912743898722,
-0.0136758532865582));
#46586=CARTESIAN_POINT('Ctrl Pts',(-0.0126652476264479,-0.0370833239097378,
-0.0136758532865582));
#46587=CARTESIAN_POINT('Ctrl Pts',(-0.012829577798866,-0.0370746592126169,
-0.0136485523980478));
#46588=CARTESIAN_POINT('Ctrl Pts',(-0.0131725324316519,-0.037054893602503,
-0.0135310052826243));
#46589=CARTESIAN_POINT('Ctrl Pts',(-0.0133443497294871,-0.0370438537318456,
-0.0134311662284271));
#46590=CARTESIAN_POINT('Ctrl Pts',(-0.0136344816805116,-0.0370227894016187,
-0.013175373620329));
#46591=CARTESIAN_POINT('Ctrl Pts',(-0.0137517878987089,-0.0370133850494514,
-0.0130238451589815));
#46592=CARTESIAN_POINT('Ctrl Pts',(-0.0139276744830711,-0.0369941238350818,
-0.0126771433003291));
#46593=CARTESIAN_POINT('Ctrl Pts',(-0.0139814715786065,-0.0369833765575813,
-0.0124836923053207));
#46594=CARTESIAN_POINT('Ctrl Pts',(-0.0140102024472209,-0.0369615829871331,
-0.0120914080372542));
#46595=CARTESIAN_POINT('Ctrl Pts',(-0.013986536706735,-0.0369507524861803,
-0.0118964590201025));
#46596=CARTESIAN_POINT('Ctrl Pts',(-0.0138670801188791,-0.0369303696802525,
-0.0115295685134022));
#46597=CARTESIAN_POINT('Ctrl Pts',(-0.0137736284195215,-0.0369215756173142,
-0.0113607083418922));
#46598=CARTESIAN_POINT('Ctrl Pts',(-0.0135227590025235,-0.0369011675735817,
-0.0110605373438294));
#46599=CARTESIAN_POINT('Ctrl Pts',(-0.013365188521414,-0.0368900804687017,
-0.0109343216472075));
#46600=CARTESIAN_POINT('Ctrl Pts',(-0.0130166440242008,-0.0368683179439088,
-0.0107545675325336));
#46601=CARTESIAN_POINT('Ctrl Pts',(-0.0128303599796439,-0.0368578422903703,
-0.0107000974349616));
#46602=CARTESIAN_POINT('Ctrl Pts',(-0.0124432664521831,-0.0368382186202807,
-0.0106641109685799));
#46603=CARTESIAN_POINT('Ctrl Pts',(-0.0122460134054272,-0.0368288138396488,
-0.0106845154083571));
#46604=CARTESIAN_POINT('Ctrl Pts',(-0.011869596414965,-0.0368074813678198,
-0.010800511041888));
#46605=CARTESIAN_POINT('Ctrl Pts',(-0.0116942542727957,-0.0367964114250926,
-0.0108953274811244));
#46606=CARTESIAN_POINT('Ctrl Pts',(-0.0113959034381422,-0.0367751822121979,
-0.0111428203412331));
#46607=CARTESIAN_POINT('Ctrl Pts',(-0.0112739723597906,-0.0367654340214763,
-0.0112909799176879));
#46608=CARTESIAN_POINT('Ctrl Pts',(-0.0110878097215295,-0.0367464616705573,
-0.0116324822342288));
#46609=CARTESIAN_POINT('Ctrl Pts',(-0.0110283132596915,-0.0367358095895788,
-0.0118242196918422));
#46610=CARTESIAN_POINT('Ctrl Pts',(-0.0109878992504014,-0.0367140441641329,
-0.0122159973498669));
#46611=CARTESIAN_POINT('Ctrl Pts',(-0.0110059300757061,-0.0367031483334851,
-0.0124121223015279));
#46612=CARTESIAN_POINT('Ctrl Pts',(-0.0111148202181895,-0.0366825904386729,
-0.0127821644081477));
#46613=CARTESIAN_POINT('Ctrl Pts',(-0.0112029772453076,-0.0366737547753834,
-0.0129530687178596));
#46614=CARTESIAN_POINT('Ctrl Pts',(-0.0114447104426529,-0.036653583173973,
-0.013260552188956));
#46615=CARTESIAN_POINT('Ctrl Pts',(-0.0115989854789676,-0.0366425166922058,
-0.0133917333313388));
#46616=CARTESIAN_POINT('Ctrl Pts',(-0.0119432119671359,-0.0366206707177402,
-0.0135819706452803));
#46617=CARTESIAN_POINT('Ctrl Pts',(-0.0121284036297215,-0.0366100976904278,
-0.013641838259792));
#46618=CARTESIAN_POINT('Ctrl Pts',(-0.0123797614962902,-0.0365971596534063,
-0.0136722429967861));
#46619=CARTESIAN_POINT('Ctrl Pts',(-0.0124399115641857,-0.0365941653960882,
-0.0136758532865582));
#46620=CARTESIAN_POINT('Ctrl Pts',(-0.0124999999999998,-0.0365912743898722,
-0.0136758532865582));
#46621=CARTESIAN_POINT('Origin',(-0.0125,-0.0332787743898722,-0.0121758532865583));
#46622=CARTESIAN_POINT('',(-0.0125,-0.0360287743898722,-0.0136758532865582));
#46623=CARTESIAN_POINT('',(-0.0125,-0.0360912743898722,-0.0136758532865582));
#46624=CARTESIAN_POINT('',(-0.0125,-0.0332787743898722,-0.0136758532865583));
#46625=CARTESIAN_POINT('Ctrl Pts',(-0.0125,-0.0360287743898722,-0.0136758532865582));
#46626=CARTESIAN_POINT('Ctrl Pts',(-0.01242444109938,-0.0360324097191733,
-0.0136758532865582));
#46627=CARTESIAN_POINT('Ctrl Pts',(-0.0123488306048482,-0.0360362060960539,
-0.0136701449369665));
#46628=CARTESIAN_POINT('Ctrl Pts',(-0.0120825640737028,-0.0360501450852568,
-0.0136295284859621));
#46629=CARTESIAN_POINT('Ctrl Pts',(-0.0118987796343164,-0.0360608177353903,
-0.0135636370678137));
#46630=CARTESIAN_POINT('Ctrl Pts',(-0.0115617241681493,-0.0360826091181342,
-0.0133629444814025));
#46631=CARTESIAN_POINT('Ctrl Pts',(-0.0114127616918364,-0.0360935183899258,
-0.0132282212743018));
#46632=CARTESIAN_POINT('Ctrl Pts',(-0.011181264564215,-0.0361133426135339,
-0.0129155140112531));
#46633=CARTESIAN_POINT('Ctrl Pts',(-0.011098214750844,-0.036122290120798,
-0.0127425701298929));
#46634=CARTESIAN_POINT('Ctrl Pts',(-0.0109997401142268,-0.0361430158280654,
-0.0123695073990797));
#46635=CARTESIAN_POINT('Ctrl Pts',(-0.0109872990402609,-0.0361539672422251,
-0.0121723819442055));
#46636=CARTESIAN_POINT('Ctrl Pts',(-0.0110392177022437,-0.0361756929000075,
-0.0117813201041219));
#46637=CARTESIAN_POINT('Ctrl Pts',(-0.0111043157059502,-0.0361861917332313,
-0.0115914328170068));
#46638=CARTESIAN_POINT('Ctrl Pts',(-0.0113005680489685,-0.0362049754743923,
-0.0112551371644226));
#46639=CARTESIAN_POINT('Ctrl Pts',(-0.0114271766305707,-0.036215089887779,
-0.0111103107785103));
#46640=CARTESIAN_POINT('Ctrl Pts',(-0.0117336109130104,-0.036236472392845,
-0.0108713003425021));
#46641=CARTESIAN_POINT('Ctrl Pts',(-0.0119123357012763,-0.0362475622148453,
-0.0107816271643373));
#46642=CARTESIAN_POINT('Ctrl Pts',(-0.0122912238587956,-0.036268677548959,
-0.0106777286754561));
#46643=CARTESIAN_POINT('Ctrl Pts',(-0.012487336948627,-0.0362778166274809,
-0.0106633068888324));
#46644=CARTESIAN_POINT('Ctrl Pts',(-0.0128722075965176,-0.0362976313768669,
-0.0107100223502403));
#46645=CARTESIAN_POINT('Ctrl Pts',(-0.0130573818425314,-0.0363082057927803,
-0.0107699701207729));
#46646=CARTESIAN_POINT('Ctrl Pts',(-0.013401541774164,-0.0363300528768179,
-0.0109603626586073));
#46647=CARTESIAN_POINT('Ctrl Pts',(-0.0135557666436706,-0.0363411189801075,
-0.0110916170672557));
#46648=CARTESIAN_POINT('Ctrl Pts',(-0.0137973633312287,-0.0363612870144914,
-0.0113992085672866));
#46649=CARTESIAN_POINT('Ctrl Pts',(-0.0138854417969202,-0.0363701238590329,
-0.011570143731452));
#46650=CARTESIAN_POINT('Ctrl Pts',(-0.0139941733700868,-0.0363906843444493,
-0.0119402324689471));
#46651=CARTESIAN_POINT('Ctrl Pts',(-0.0140121193322341,-0.0364015810871345,
-0.0121363738372794));
#46652=CARTESIAN_POINT('Ctrl Pts',(-0.013971530159525,-0.0364233459425802,
-0.0125281412353024));
#46653=CARTESIAN_POINT('Ctrl Pts',(-0.0139119486611866,-0.036433996523078,
-0.0127198516842618));
#46654=CARTESIAN_POINT('Ctrl Pts',(-0.0137256322874889,-0.0364529644987118,
-0.01306127524567));
#46655=CARTESIAN_POINT('Ctrl Pts',(-0.0136036311559106,-0.0364627184441798,
-0.0132093844764852));
#46656=CARTESIAN_POINT('Ctrl Pts',(-0.0133051564697893,-0.0364839501087037,
-0.0134567510782099));
#46657=CARTESIAN_POINT('Ctrl Pts',(-0.0131297621407755,-0.0364950204278691,
-0.0135514906789523));
#46658=CARTESIAN_POINT('Ctrl Pts',(-0.0127979006941046,-0.0365138230573143,
-0.0136535844522717));
#46659=CARTESIAN_POINT('Ctrl Pts',(-0.012649247406269,-0.0365215937206901,
-0.0136758532865582));
#46660=CARTESIAN_POINT('Ctrl Pts',(-0.0124999999999997,-0.0365287743898722,
-0.0136758532865582));
#46661=CARTESIAN_POINT('Ctrl Pts',(-0.0124999999999998,-0.0365912743898722,
-0.0136758532865582));
#46662=CARTESIAN_POINT('Ctrl Pts',(-0.0126339852058531,-0.03658482802365,
-0.0136758532865582));
#46663=CARTESIAN_POINT('Ctrl Pts',(-0.0127676156499676,-0.0365779001980971,
-0.0136579062852937));
#46664=CARTESIAN_POINT('Ctrl Pts',(-0.0130882901520083,-0.0365600247360929,
-0.0135698141833699));
#46665=CARTESIAN_POINT('Ctrl Pts',(-0.0132669667741575,-0.0365489351298924,
-0.0134800653478386));
#46666=CARTESIAN_POINT('Ctrl Pts',(-0.0135732831917688,-0.0365275548590379,
-0.0132409311955683));
#46667=CARTESIAN_POINT('Ctrl Pts',(-0.0136998241499775,-0.0365174423603507,
-0.0130960566116852));
#46668=CARTESIAN_POINT('Ctrl Pts',(-0.0138959299193217,-0.0364986635982211,
-0.0127596863311846));
#46669=CARTESIAN_POINT('Ctrl Pts',(-0.0139609478795168,-0.0364881587948206,
-0.0125697725756292));
#46670=CARTESIAN_POINT('Ctrl Pts',(-0.0140127012380386,-0.0364664324003575,
-0.0121786974752932));
#46671=CARTESIAN_POINT('Ctrl Pts',(-0.0140001794909881,-0.0364554817239551,
-0.0119815853000501));
#46672=CARTESIAN_POINT('Ctrl Pts',(-0.0139015549098239,-0.0364347583984683,
-0.0116085654412878));
#46673=CARTESIAN_POINT('Ctrl Pts',(-0.0138184323132252,-0.0364258129894517,
-0.0114356511185721));
#46674=CARTESIAN_POINT('Ctrl Pts',(-0.0135868027609335,-0.036405984938985,
-0.0111230354548772));
#46675=CARTESIAN_POINT('Ctrl Pts',(-0.0134377843005641,-0.0363950746804312,
-0.0109883736915671));
#46676=CARTESIAN_POINT('Ctrl Pts',(-0.0131006520467281,-0.0363732835866736,
-0.0107878245088091));
#46677=CARTESIAN_POINT('Ctrl Pts',(-0.012916848257935,-0.0363626121552087,
-0.0107220104768881));
#46678=CARTESIAN_POINT('Ctrl Pts',(-0.0125344407406388,-0.0363425975504287,
-0.0106638339539603));
#46679=CARTESIAN_POINT('Ctrl Pts',(-0.0123394827638854,-0.0363336590140195,
-0.0106719828088111));
#46680=CARTESIAN_POINT('Ctrl Pts',(-0.0119581661425258,-0.03631278205237,
-0.0107630936662273));
#46681=CARTESIAN_POINT('Ctrl Pts',(-0.0117760219033341,-0.0363016823644665,
-0.0108471993541692));
#46682=CARTESIAN_POINT('Ctrl Pts',(-0.011461148124963,-0.0362801478962951,
-0.0110770628262301));
#46683=CARTESIAN_POINT('Ctrl Pts',(-0.0113296709011859,-0.0362698989078036,
-0.0112183011803048));
#46684=CARTESIAN_POINT('Ctrl Pts',(-0.0111219776131219,-0.0362506820193385,
-0.0115503738377329));
#46685=CARTESIAN_POINT('Ctrl Pts',(-0.011050801427276,-0.0362404926029528,
-0.0117399254511084));
#46686=CARTESIAN_POINT('Ctrl Pts',(-0.0109878754452061,-0.036218733509438,
-0.0121315891343748));
#46687=CARTESIAN_POINT('Ctrl Pts',(-0.0109950504691957,-0.0362077379708741,
-0.0123295088285253));
#46688=CARTESIAN_POINT('Ctrl Pts',(-0.0110837554713219,-0.0361868592603589,
-0.012705325617798));
#46689=CARTESIAN_POINT('Ctrl Pts',(-0.0111621069339057,-0.0361777450344641,
-0.0128802088468219));
#46690=CARTESIAN_POINT('Ctrl Pts',(-0.011385026356248,-0.0361581704503927,
-0.0131987861079011));
#46691=CARTESIAN_POINT('Ctrl Pts',(-0.0115303178694841,-0.0361473289706943,
-0.0133374270942092));
#46692=CARTESIAN_POINT('Ctrl Pts',(-0.0118622834508789,-0.0361255269137158,
-0.0135473198920959));
#46693=CARTESIAN_POINT('Ctrl Pts',(-0.0120447500101688,-0.0361147791043814,
-0.0136181996767634));
#46694=CARTESIAN_POINT('Ctrl Pts',(-0.0123231115071583,-0.0361000021471243,
-0.0136680338823606));
#46695=CARTESIAN_POINT('Ctrl Pts',(-0.0124115647816169,-0.0360955292313004,
-0.0136758532865582));
#46696=CARTESIAN_POINT('Ctrl Pts',(-0.0125,-0.0360912743898722,-0.0136758532865582));
#46697=CARTESIAN_POINT('Origin',(-0.0125,-0.0332787743898722,-0.0121758532865583));
#46698=CARTESIAN_POINT('',(-0.0125,-0.0355287743898722,-0.0136758532865582));
#46699=CARTESIAN_POINT('',(-0.0125,-0.0355912743898722,-0.0136758532865582));
#46700=CARTESIAN_POINT('',(-0.0125,-0.0332787743898722,-0.0136758532865583));
#46701=CARTESIAN_POINT('Ctrl Pts',(-0.0125,-0.0355287743898722,-0.0136758532865582));
#46702=CARTESIAN_POINT('Ctrl Pts',(-0.0123973442969718,-0.035533713414687,
-0.0136758532865582));
#46703=CARTESIAN_POINT('Ctrl Pts',(-0.0122947420425006,-0.035538942531353,
-0.0136653174042946));
#46704=CARTESIAN_POINT('Ctrl Pts',(-0.0120033924529855,-0.035554647740067,
-0.0136045621823964));
#46705=CARTESIAN_POINT('Ctrl Pts',(-0.011822534712545,-0.035565470259822,
-0.0135282062665997));
#46706=CARTESIAN_POINT('Ctrl Pts',(-0.0114964777476188,-0.0355872657978458,
-0.0133083141271581));
#46707=CARTESIAN_POINT('Ctrl Pts',(-0.01135535830582,-0.0355980232805698,
-0.0131654707922246));
#46708=CARTESIAN_POINT('Ctrl Pts',(-0.0111419578240932,-0.0356173169465204,
-0.0128405192947112));
#46709=CARTESIAN_POINT('Ctrl Pts',(-0.0110687906194607,-0.0356266871868369,
-0.0126634229411933));
#46710=CARTESIAN_POINT('Ctrl Pts',(-0.010991065366143,-0.0356477326223681,
-0.0122846051016316));
#46711=CARTESIAN_POINT('Ctrl Pts',(-0.0109898247408614,-0.0356587684692245,
-0.0120859598582161));
#46712=CARTESIAN_POINT('Ctrl Pts',(-0.0110644253212016,-0.0356803327561648,
-0.0116978026932913));
#46713=CARTESIAN_POINT('Ctrl Pts',(-0.0111402055168341,-0.0356901174045244,
-0.0115122716263748));
#46714=CARTESIAN_POINT('Ctrl Pts',(-0.0113558489600221,-0.0357095258635238,
-0.011187072502319));
#46715=CARTESIAN_POINT('Ctrl Pts',(-0.0114914712724027,-0.0357198841194876,
-0.0110490800233052));
#46716=CARTESIAN_POINT('Ctrl Pts',(-0.0118134552809888,-0.0357415335636135,
-0.010827392696869));
#46717=CARTESIAN_POINT('Ctrl Pts',(-0.0119984324801342,-0.0357526324616988,
-0.0107482222729592));
#46718=CARTESIAN_POINT('Ctrl Pts',(-0.0123817112461122,-0.0357732954923294,
-0.0106682114663947));
#46719=CARTESIAN_POINT('Ctrl Pts',(-0.0125757163912609,-0.0357821290156334,
-0.0106654751773376));
#46720=CARTESIAN_POINT('Ctrl Pts',(-0.0129558867186165,-0.0358023152945974,
-0.0107337068975336));
#46721=CARTESIAN_POINT('Ctrl Pts',(-0.0131383298476193,-0.0358130643140553,
-0.010804670829092));
#46722=CARTESIAN_POINT('Ctrl Pts',(-0.0134702071915908,-0.0358348664160461,
-0.0110147180791208));
#46723=CARTESIAN_POINT('Ctrl Pts',(-0.0136154357263315,-0.035845706681201,
-0.0111534244238167));
#46724=CARTESIAN_POINT('Ctrl Pts',(-0.0138382097237242,-0.0358652770036945,
-0.011472100151494));
#46725=CARTESIAN_POINT('Ctrl Pts',(-0.0139164817782309,-0.0358743945791995,
-0.0116470166944518));
#46726=CARTESIAN_POINT('Ctrl Pts',(-0.0140050201548324,-0.0358952758616462,
-0.012022879778492));
#46727=CARTESIAN_POINT('Ctrl Pts',(-0.0140121052211236,-0.0359062720853291,
-0.012220811804784));
#46728=CARTESIAN_POINT('Ctrl Pts',(-0.0139490008074887,-0.0359280282804241,
-0.0126124233164942));
#46729=CARTESIAN_POINT('Ctrl Pts',(-0.0138777541279319,-0.0359382110540525,
-0.0128019133469663));
#46730=CARTESIAN_POINT('Ctrl Pts',(-0.0136699400069597,-0.0359574308744097,
-0.013133882263771));
#46731=CARTESIAN_POINT('Ctrl Pts',(-0.0135383996098182,-0.0359676815656632,
-0.0132750724978011));
#46732=CARTESIAN_POINT('Ctrl Pts',(-0.0132234169383219,-0.0359892178877941,
-0.0135048141039771));
#46733=CARTESIAN_POINT('Ctrl Pts',(-0.0130412289705088,-0.0360003176285395,
-0.0135888459540308));
#46734=CARTESIAN_POINT('Ctrl Pts',(-0.0127337078466152,-0.0360171503918094,
-0.0136621832207637));
#46735=CARTESIAN_POINT('Ctrl Pts',(-0.0126169341724723,-0.036023148391876,
-0.0136758532865582));
#46736=CARTESIAN_POINT('Ctrl Pts',(-0.0125,-0.0360287743898722,-0.0136758532865582));
#46737=CARTESIAN_POINT('Ctrl Pts',(-0.0125,-0.0360912743898722,-0.0136758532865582));
#46738=CARTESIAN_POINT('Ctrl Pts',(-0.0126029942953792,-0.0360863190745253,
-0.0136758532865582));
#46739=CARTESIAN_POINT('Ctrl Pts',(-0.0127059354300288,-0.0360810717196226,
-0.0136652477854601));
#46740=CARTESIAN_POINT('Ctrl Pts',(-0.0130022256212186,-0.0360650943354945,
-0.0136032516217705));
#46741=CARTESIAN_POINT('Ctrl Pts',(-0.0131871577799667,-0.0360539953548263,
-0.0135240002126186));
#46742=CARTESIAN_POINT('Ctrl Pts',(-0.0135090278211091,-0.036032347653377,
-0.0133021782251363));
#46743=CARTESIAN_POINT('Ctrl Pts',(-0.013644583361116,-0.0360219911172423,
-0.013164132006828));
#46744=CARTESIAN_POINT('Ctrl Pts',(-0.0138600983406451,-0.0360025857322556,
-0.0128388210416437));
#46745=CARTESIAN_POINT('Ctrl Pts',(-0.0139358046676858,-0.0359927950701439,
-0.012653225531447));
#46746=CARTESIAN_POINT('Ctrl Pts',(-0.0140102176635265,-0.0359712275708235,
-0.0122650105436802));
#46747=CARTESIAN_POINT('Ctrl Pts',(-0.0140088809225687,-0.0359601922981304,
-0.0120663756352049));
#46748=CARTESIAN_POINT('Ctrl Pts',(-0.013930977982065,-0.0359391495157561,
-0.0116876055524676));
#46749=CARTESIAN_POINT('Ctrl Pts',(-0.0138577276307545,-0.0359297839804837,
-0.0115105453092611));
#46750=CARTESIAN_POINT('Ctrl Pts',(-0.0136441741427528,-0.0359104857680691,
-0.0111856951536888));
#46751=CARTESIAN_POINT('Ctrl Pts',(-0.0135029868608712,-0.035899726863706,
-0.0110429181422186));
#46752=CARTESIAN_POINT('Ctrl Pts',(-0.0131768328187235,-0.0358779310697273,
-0.0108231849310812));
#46753=CARTESIAN_POINT('Ctrl Pts',(-0.0129959480223017,-0.0358671096786955,
-0.0107469165116545));
#46754=CARTESIAN_POINT('Ctrl Pts',(-0.0126181581242682,-0.0358467498906632,
-0.0106683154404723));
#46755=CARTESIAN_POINT('Ctrl Pts',(-0.0124250757754456,-0.0358379558073767,
-0.0106655496927537));
#46756=CARTESIAN_POINT('Ctrl Pts',(-0.012039925485056,-0.0358175173530894,
-0.0107342341755916));
#46757=CARTESIAN_POINT('Ctrl Pts',(-0.0118521914988264,-0.0358064282541243,
-0.0108082769358769));
#46758=CARTESIAN_POINT('Ctrl Pts',(-0.0115231692681669,-0.0357846779220503,
-0.0110214056702193));
#46759=CARTESIAN_POINT('Ctrl Pts',(-0.0113834010332159,-0.0357742155777443,
-0.0111559643810162));
#46760=CARTESIAN_POINT('Ctrl Pts',(-0.0111597494657645,-0.0357546168898119,
-0.0114741412685692));
#46761=CARTESIAN_POINT('Ctrl Pts',(-0.0110793951575888,-0.0357451722793311,
-0.0116556912762991));
#46762=CARTESIAN_POINT('Ctrl Pts',(-0.0109931706618282,-0.035723812201625,
-0.0120401726750083));
#46763=CARTESIAN_POINT('Ctrl Pts',(-0.0109884090513756,-0.0357127455908268,
-0.0122393716693753));
#46764=CARTESIAN_POINT('Ctrl Pts',(-0.0110550403015091,-0.0356915375024731,
-0.0126211172597409));
#46765=CARTESIAN_POINT('Ctrl Pts',(-0.0111230610732549,-0.0356818381010433,
-0.0128004878644392));
#46766=CARTESIAN_POINT('Ctrl Pts',(-0.0113269772540736,-0.035662828151014,
-0.0131316528798298));
#46767=CARTESIAN_POINT('Ctrl Pts',(-0.0114638446058427,-0.0356521632461508,
-0.0132785282477472));
#46768=CARTESIAN_POINT('Ctrl Pts',(-0.0117837543913012,-0.0356303930961302,
-0.0135081536462352));
#46769=CARTESIAN_POINT('Ctrl Pts',(-0.0119628602916793,-0.0356195051970148,
-0.0135898974949996));
#46770=CARTESIAN_POINT('Ctrl Pts',(-0.0122666642932065,-0.035602879297975,
-0.0136622258942475));
#46771=CARTESIAN_POINT('Ctrl Pts',(-0.0123832482692233,-0.0355968916101383,
-0.0136758532865582));
#46772=CARTESIAN_POINT('Ctrl Pts',(-0.0125000000000001,-0.0355912743898722,
-0.0136758532865582));
#46773=CARTESIAN_POINT('Origin',(-0.0125,-0.0332787743898722,-0.0121758532865583));
#46774=CARTESIAN_POINT('',(-0.0125000000000001,-0.0350287743898722,-0.0136758532865582));
#46775=CARTESIAN_POINT('',(-0.0125000000000001,-0.0350912743898723,-0.0136758532865582));
#46776=CARTESIAN_POINT('',(-0.0125,-0.0332787743898722,-0.0136758532865583));
#46777=CARTESIAN_POINT('Ctrl Pts',(-0.0125000000000002,-0.0350287743898722,
-0.0136758532865582));
#46778=CARTESIAN_POINT('Ctrl Pts',(-0.0123690260553798,-0.0350350758767208,
-0.0136758532865583));
#46779=CARTESIAN_POINT('Ctrl Pts',(-0.0122383852229765,-0.0350418377063322,
-0.0136587039798108));
#46780=CARTESIAN_POINT('Ctrl Pts',(-0.0119224772799044,-0.0350593906313495,
-0.013573967287105));
#46781=CARTESIAN_POINT('Ctrl Pts',(-0.0117452953091194,-0.0350703356724196,
-0.0134868339841646));
#46782=CARTESIAN_POINT('Ctrl Pts',(-0.0114317811740397,-0.0350920675195657,
-0.0132475098977541));
#46783=CARTESIAN_POINT('Ctrl Pts',(-0.0112993449231415,-0.0351026178745569,
-0.013096670562235));
#46784=CARTESIAN_POINT('Ctrl Pts',(-0.0111050513615919,-0.0351213588999748,
-0.0127593321047111));
#46785=CARTESIAN_POINT('Ctrl Pts',(-0.0110422862343725,-0.0351314568690709,
-0.0125775686609812));
#46786=CARTESIAN_POINT('Ctrl Pts',(-0.0109870935977505,-0.0351528201246496,
-0.0121930300605649));
#46787=CARTESIAN_POINT('Ctrl Pts',(-0.010998029993029,-0.0351639080293944,
-0.0119934477751578));
#46788=CARTESIAN_POINT('Ctrl Pts',(-0.0110960424747355,-0.0351850508379232,
-0.0116128772216393));
#46789=CARTESIAN_POINT('Ctrl Pts',(-0.011181036805097,-0.0351942190108102,
-0.0114353356659036));
#46790=CARTESIAN_POINT('Ctrl Pts',(-0.0114129086325599,-0.0352140100870733,
-0.0111244707064398));
#46791=CARTESIAN_POINT('Ctrl Pts',(-0.0115568922039538,-0.0352245725709683,
-0.0109936081473295));
#46792=CARTESIAN_POINT('Ctrl Pts',(-0.0118929902252958,-0.0352464100411046,
-0.0107895980717107));
#46793=CARTESIAN_POINT('Ctrl Pts',(-0.0120834431656559,-0.0352574793131677,
-0.010720978446593));
#46794=CARTESIAN_POINT('Ctrl Pts',(-0.0124704063087179,-0.0352776778052715,
-0.0106640725552989));
#46795=CARTESIAN_POINT('Ctrl Pts',(-0.0126625876140318,-0.0352865050838931,
-0.0106725482631292));
#46796=CARTESIAN_POINT('Ctrl Pts',(-0.0130377914433727,-0.0353070434015203,
-0.0107620556020949));
#46797=CARTESIAN_POINT('Ctrl Pts',(-0.013216867725968,-0.0353179322870024,
-0.0108438862595647));
#46798=CARTESIAN_POINT('Ctrl Pts',(-0.0135366757238662,-0.0353397018717546,
-0.0110736676096182));
#46799=CARTESIAN_POINT('Ctrl Pts',(-0.0136734733591466,-0.0353503652034107,
-0.0112206070945778));
#46800=CARTESIAN_POINT('Ctrl Pts',(-0.0138772356830381,-0.0353693705207853,
-0.0115518718224145));
#46801=CARTESIAN_POINT('Ctrl Pts',(-0.0139451730544627,-0.0353790758692342,
-0.0117312799150757));
#46802=CARTESIAN_POINT('Ctrl Pts',(-0.0140116230129778,-0.0354002865658375,
-0.012113072453934));
#46803=CARTESIAN_POINT('Ctrl Pts',(-0.0140067633305862,-0.0354113535965583,
-0.0123122790069097));
#46804=CARTESIAN_POINT('Ctrl Pts',(-0.013920350323081,-0.0354327102796505,
-0.0126966993025684));
#46805=CARTESIAN_POINT('Ctrl Pts',(-0.0138399218549572,-0.0354421499161469,
-0.0128781849634066));
#46806=CARTESIAN_POINT('Ctrl Pts',(-0.0136161396278266,-0.0354617516849645,
-0.0131962464536166));
#46807=CARTESIAN_POINT('Ctrl Pts',(-0.0134763040444793,-0.0354722156753386,
-0.0133307477720209));
#46808=CARTESIAN_POINT('Ctrl Pts',(-0.0131471681135012,-0.0354939675247689,
-0.0135437341964632));
#46809=CARTESIAN_POINT('Ctrl Pts',(-0.0129593900056609,-0.0355050563869362,
-0.0136176920111582));
#46810=CARTESIAN_POINT('Ctrl Pts',(-0.0126757376743542,-0.035520104819105,
-0.0136681353197265));
#46811=CARTESIAN_POINT('Ctrl Pts',(-0.0125878596923307,-0.035524547238454,
-0.0136758532865582));
#46812=CARTESIAN_POINT('Ctrl Pts',(-0.0125,-0.0355287743898722,-0.0136758532865582));
#46813=CARTESIAN_POINT('Ctrl Pts',(-0.0125000000000001,-0.0355912743898722,
-0.0136758532865582));
#46814=CARTESIAN_POINT('Ctrl Pts',(-0.0125731215724756,-0.0355877563265762,
-0.0136758532865582));
#46815=CARTESIAN_POINT('Ctrl Pts',(-0.0126462945114834,-0.035584087290529,
-0.01367050723696));
#46816=CARTESIAN_POINT('Ctrl Pts',(-0.0129172360277393,-0.0355699411921168,
-0.0136305321661541));
#46817=CARTESIAN_POINT('Ctrl Pts',(-0.0131076478651028,-0.0355588715366797,
-0.0135618275470965));
#46818=CARTESIAN_POINT('Ctrl Pts',(-0.0134436378156878,-0.0355370352820993,
-0.0133576740474468));
#46819=CARTESIAN_POINT('Ctrl Pts',(-0.0135875566235559,-0.035526474291301,
-0.0132267530660998));
#46820=CARTESIAN_POINT('Ctrl Pts',(-0.0138193014513857,-0.0355066861649722,
-0.0129157743344553));
#46821=CARTESIAN_POINT('Ctrl Pts',(-0.013904224462027,-0.0354975142893684,
-0.0127381714774883));
#46822=CARTESIAN_POINT('Ctrl Pts',(-0.0140020559383961,-0.0354763680685431,
-0.0123575395026348));
#46823=CARTESIAN_POINT('Ctrl Pts',(-0.0140128968929006,-0.0354652804136489,
-0.0121579617145387));
#46824=CARTESIAN_POINT('Ctrl Pts',(-0.0139575274879115,-0.0354439195749494,
-0.0117734666179479));
#46825=CARTESIAN_POINT('Ctrl Pts',(-0.0138946820051359,-0.0354338236622805,
-0.011591740189908));
#46826=CARTESIAN_POINT('Ctrl Pts',(-0.0137002418276673,-0.035415087971294,
-0.0112544977521507));
#46827=CARTESIAN_POINT('Ctrl Pts',(-0.0135677386958255,-0.0354045311341893,
-0.0111037184115987));
#46828=CARTESIAN_POINT('Ctrl Pts',(-0.0132541247299294,-0.0353827985347396,
-0.0108645401543042));
#46829=CARTESIAN_POINT('Ctrl Pts',(-0.0130769123191492,-0.035371854296484,
-0.0107774884763052));
#46830=CARTESIAN_POINT('Ctrl Pts',(-0.0127042296422369,-0.0353511515527453,
-0.010677695033225));
#46831=CARTESIAN_POINT('Ctrl Pts',(-0.0125128264173641,-0.0353422236530032,
-0.0106638958203951));
#46832=CARTESIAN_POINT('Ctrl Pts',(-0.0121263928261186,-0.0353223626077001,
-0.0107095708375193));
#46833=CARTESIAN_POINT('Ctrl Pts',(-0.0119354822516037,-0.0353114439086704,
-0.0107719771878248));
#46834=CARTESIAN_POINT('Ctrl Pts',(-0.0115939785841702,-0.0352896554669203,
-0.0109648593878639));
#46835=CARTESIAN_POINT('Ctrl Pts',(-0.0114455760355385,-0.0352789946276801,
-0.0110916088463094));
#46836=CARTESIAN_POINT('Ctrl Pts',(-0.0112049775822295,-0.0352590025567665,
-0.011394594653846));
#46837=CARTESIAN_POINT('Ctrl Pts',(-0.0111151053160591,-0.0352500455327326,
-0.011567972715073));
#46838=CARTESIAN_POINT('Ctrl Pts',(-0.0110047390885022,-0.0352291411203124,
-0.0119442521386352));
#46839=CARTESIAN_POINT('Ctrl Pts',(-0.0109872461493976,-0.0352180419718032,
-0.0121440368118008));
#46840=CARTESIAN_POINT('Ctrl Pts',(-0.0110302588603089,-0.0351965236781261,
-0.0125313660979891));
#46841=CARTESIAN_POINT('Ctrl Pts',(-0.0110874688325119,-0.0351862894743138,
-0.0127155817666109));
#46842=CARTESIAN_POINT('Ctrl Pts',(-0.011272504754752,-0.0351670979784338,
-0.0130610286924501));
#46843=CARTESIAN_POINT('Ctrl Pts',(-0.0114018404118615,-0.0351568504650813,
-0.0132171827805111));
#46844=CARTESIAN_POINT('Ctrl Pts',(-0.0117107302579797,-0.035135066377573,
-0.0134663970233921));
#46845=CARTESIAN_POINT('Ctrl Pts',(-0.0118860163787744,-0.0351240768597058,
-0.0135584151995339));
#46846=CARTESIAN_POINT('Ctrl Pts',(-0.0122125627321767,-0.0351056794412658,
-0.0136551273882549));
#46847=CARTESIAN_POINT('Ctrl Pts',(-0.0123560152331419,-0.0350982018601977,
-0.0136758532865583));
#46848=CARTESIAN_POINT('Ctrl Pts',(-0.0125000000000002,-0.0350912743898723,
-0.0136758532865582));
#46849=CARTESIAN_POINT('Origin',(-0.0125,-0.0332787743898722,-0.0121758532865583));
#46850=CARTESIAN_POINT('',(-0.0125000000000001,-0.0345287743898722,-0.0136758532865583));
#46851=CARTESIAN_POINT('',(-0.0125,-0.0345912743898723,-0.0136758532865583));
#46852=CARTESIAN_POINT('',(-0.0125,-0.0332787743898722,-0.0136758532865583));
#46853=CARTESIAN_POINT('Ctrl Pts',(-0.0125000000000001,-0.0345287743898722,
-0.0136758532865583));
#46854=CARTESIAN_POINT('Ctrl Pts',(-0.0123412969419184,-0.0345364099943143,
-0.0136758532865583));
#46855=CARTESIAN_POINT('Ctrl Pts',(-0.0121834096834421,-0.0345447058197249,
-0.0136506723253203));
#46856=CARTESIAN_POINT('Ctrl Pts',(-0.0118453588160428,-0.0345640523957705,
-0.0135397168655593));
#46857=CARTESIAN_POINT('Ctrl Pts',(-0.0116723716475794,-0.0345750832202484,
-0.0134422297491893));
#46858=CARTESIAN_POINT('Ctrl Pts',(-0.0113722808018559,-0.0345966750745294,
-0.0131846955867555));
#46859=CARTESIAN_POINT('Ctrl Pts',(-0.0112486976652099,-0.0346065120281936,
-0.0130265757967733));
#46860=CARTESIAN_POINT('Ctrl Pts',(-0.0110735036067596,-0.0346258940193351,
-0.0126776999562268));
#46861=CARTESIAN_POINT('Ctrl Pts',(-0.0110211232741819,-0.0346362374298867,
-0.0124915185662973));
#46862=CARTESIAN_POINT('Ctrl Pts',(-0.0109886368102513,-0.0346578717566075,
-0.0121021006853227));
#46863=CARTESIAN_POINT('Ctrl Pts',(-0.0110117654649977,-0.0346689712892342,
-0.0119023090980412));
#46864=CARTESIAN_POINT('Ctrl Pts',(-0.0111326365248452,-0.0346896646047389,
-0.0115298294189562));
#46865=CARTESIAN_POINT('Ctrl Pts',(-0.0112266804936695,-0.0346985088786647,
-0.0113599576107925));
#46866=CARTESIAN_POINT('Ctrl Pts',(-0.0114747926668439,-0.0347186712634827,
-0.0110638546472576));
#46867=CARTESIAN_POINT('Ctrl Pts',(-0.0116269447426416,-0.0347294098241466,
-0.0109408015891161));
#46868=CARTESIAN_POINT('Ctrl Pts',(-0.0119740175823262,-0.0347512113926894,
-0.0107570929138376));
#46869=CARTESIAN_POINT('Ctrl Pts',(-0.0121665380678273,-0.0347620620147946,
-0.0106999257804346));
#46870=CARTESIAN_POINT('Ctrl Pts',(-0.0125537975209007,-0.0347816688929276,
-0.0106648312160837));
#46871=CARTESIAN_POINT('Ctrl Pts',(-0.0127445094384567,-0.0347907582789375,
-0.0106837705225737));
#46872=CARTESIAN_POINT('Ctrl Pts',(-0.0131146557349637,-0.0348116174562792,
-0.01079358871509));
#46873=CARTESIAN_POINT('Ctrl Pts',(-0.0132899054570147,-0.0348226077289797,
-0.010885697109702));
#46874=CARTESIAN_POINT('Ctrl Pts',(-0.0135986514145666,-0.0348443887285896,
-0.0111350494105482));
#46875=CARTESIAN_POINT('Ctrl Pts',(-0.0137278919511177,-0.0348546289848604,
-0.0112912359963488));
#46876=CARTESIAN_POINT('Ctrl Pts',(-0.0139127670204282,-0.0348738236286432,
-0.011636739584438));
#46877=CARTESIAN_POINT('Ctrl Pts',(-0.0139698987575697,-0.0348840596689156,
-0.0118209883093416));
#46878=CARTESIAN_POINT('Ctrl Pts',(-0.0140127404949898,-0.0349055799791375,
-0.0122083538933346));
#46879=CARTESIAN_POINT('Ctrl Pts',(-0.0139951557924346,-0.0349166792024432,
-0.0124081399128387));
#46880=CARTESIAN_POINT('Ctrl Pts',(-0.013884617730595,-0.0349375802231589,
-0.0127843582857208));
#46881=CARTESIAN_POINT('Ctrl Pts',(-0.0137946774333669,-0.0349465348996107,
-0.0129576787311508));
#46882=CARTESIAN_POINT('Ctrl Pts',(-0.0135539567695427,-0.0349665297612131,
-0.0132605533286652));
#46883=CARTESIAN_POINT('Ctrl Pts',(-0.0134054928017999,-0.034977191917188,
-0.0133872438085349));
#46884=CARTESIAN_POINT('Ctrl Pts',(-0.0130638970009965,-0.0349989807021439,
-0.0135799787843043));
#46885=CARTESIAN_POINT('Ctrl Pts',(-0.0128729591856066,-0.0350098983650578,
-0.0136423006518634));
#46886=CARTESIAN_POINT('Ctrl Pts',(-0.0126170802693561,-0.0350230462712982,
-0.0136724299929882));
#46887=CARTESIAN_POINT('Ctrl Pts',(-0.0125585115005907,-0.0350259592539875,
-0.0136758532865582));
#46888=CARTESIAN_POINT('Ctrl Pts',(-0.0125000000000002,-0.0350287743898722,
-0.0136758532865582));
#46889=CARTESIAN_POINT('Ctrl Pts',(-0.0125000000000002,-0.0350912743898723,
-0.0136758532865582));
#46890=CARTESIAN_POINT('Ctrl Pts',(-0.0125453666337599,-0.0350890916866878,
-0.0136758532865582));
#46891=CARTESIAN_POINT('Ctrl Pts',(-0.0125907806026629,-0.0350868495387351,
-0.0136737952617678));
#46892=CARTESIAN_POINT('Ctrl Pts',(-0.0128341782074428,-0.0350745230540291,
-0.0136516188302729));
#46893=CARTESIAN_POINT('Ctrl Pts',(-0.0130266713454518,-0.0350636711485182,
-0.0135943581270203));
#46894=CARTESIAN_POINT('Ctrl Pts',(-0.0133736472785106,-0.0350418696700696,
-0.0134104848479301));
#46895=CARTESIAN_POINT('Ctrl Pts',(-0.013525733439843,-0.0350311324278077,
-0.0132873650850583));
#46896=CARTESIAN_POINT('Ctrl Pts',(-0.0137737125400177,-0.0350109730368056,
-0.0129911394096996));
#46897=CARTESIAN_POINT('Ctrl Pts',(-0.0138676827913623,-0.0350021273263903,
-0.0128212061438837));
#46898=CARTESIAN_POINT('Ctrl Pts',(-0.0139883688579959,-0.0349814302279859,
-0.0124486583726053));
#46899=CARTESIAN_POINT('Ctrl Pts',(-0.0140113978320624,-0.0349703306279255,
-0.012248865571518));
#46900=CARTESIAN_POINT('Ctrl Pts',(-0.0139787247326922,-0.034948698215745,
-0.0118594821522697));
#46901=CARTESIAN_POINT('Ctrl Pts',(-0.0139262585401305,-0.0349383566736314,
-0.0116733343942244));
#46902=CARTESIAN_POINT('Ctrl Pts',(-0.0137508910171738,-0.0349189780031595,
-0.0113245183257306));
#46903=CARTESIAN_POINT('Ctrl Pts',(-0.0136272076737551,-0.0349091344035578,
-0.011166432817616));
#46904=CARTESIAN_POINT('Ctrl Pts',(-0.0133269618621611,-0.0348875391053575,
-0.0109090430828455));
#46905=CARTESIAN_POINT('Ctrl Pts',(-0.0131539329313619,-0.034876508923537,
-0.0108116514366314));
#46906=CARTESIAN_POINT('Ctrl Pts',(-0.0127865458186418,-0.0348554892298485,
-0.010691275609122));
#46907=CARTESIAN_POINT('Ctrl Pts',(-0.0125964917176874,-0.0348461637623236,
-0.0106669644358509));
#46908=CARTESIAN_POINT('Ctrl Pts',(-0.0122084856345947,-0.0348268260914603,
-0.0106910743373682));
#46909=CARTESIAN_POINT('Ctrl Pts',(-0.0120144497898953,-0.0348160549330611,
-0.0107427560982287));
#46910=CARTESIAN_POINT('Ctrl Pts',(-0.0116618559123739,-0.0347942571221303,
-0.0109167667814345));
#46911=CARTESIAN_POINT('Ctrl Pts',(-0.0115059053870387,-0.0347834456367045,
-0.011035866023415));
#46912=CARTESIAN_POINT('Ctrl Pts',(-0.0112500562699438,-0.0347631105501135,
-0.0113247854708115));
#46913=CARTESIAN_POINT('Ctrl Pts',(-0.0111517355574426,-0.0347543150584318,
-0.0114911212524865));
#46914=CARTESIAN_POINT('Ctrl Pts',(-0.0110201746530845,-0.0347338441417561,
-0.0118595977526482));
#46915=CARTESIAN_POINT('Ctrl Pts',(-0.010991262683756,-0.0347227530855843,
-0.0120592367637407));
#46916=CARTESIAN_POINT('Ctrl Pts',(-0.011012892971429,-0.0347010161488557,
-0.0124505016248565));
#46917=CARTESIAN_POINT('Ctrl Pts',(-0.0110602650401685,-0.0346905682161076,
-0.012638564414322));
#46918=CARTESIAN_POINT('Ctrl Pts',(-0.0112254272227659,-0.0346709963974586,
-0.012990857150003));
#46919=CARTESIAN_POINT('Ctrl Pts',(-0.0113432864704596,-0.0346615076722981,
-0.0131509417221946));
#46920=CARTESIAN_POINT('Ctrl Pts',(-0.0116344264112255,-0.0346401181066647,
-0.0134166969154794));
#46921=CARTESIAN_POINT('Ctrl Pts',(-0.0118049253211228,-0.034629055265261,
-0.0135196464314357));
#46922=CARTESIAN_POINT('Ctrl Pts',(-0.0121540050125187,-0.0346087579314118,
-0.0136457266886208));
#46923=CARTESIAN_POINT('Ctrl Pts',(-0.0123264187636525,-0.0345996258209999,
-0.0136758532865583));
#46924=CARTESIAN_POINT('Ctrl Pts',(-0.0125,-0.0345912743898723,-0.0136758532865583));
#46925=CARTESIAN_POINT('Origin',(-0.0125,-0.0332787743898722,-0.0121758532865583));
#46926=CARTESIAN_POINT('',(-0.0124999999921269,-0.0340287743906298,-0.0136758532865583));
#46927=CARTESIAN_POINT('',(-0.0125,-0.0340912743898723,-0.0136758532865583));
#46928=CARTESIAN_POINT('',(-0.0125,-0.0332787743898722,-0.0136758532865583));
#46929=CARTESIAN_POINT('Ctrl Pts',(-0.0124999999842539,-0.0340287743906298,
-0.0136758532865583));
#46930=CARTESIAN_POINT('Ctrl Pts',(-0.0123110245217949,-0.0340378664768616,
-0.0136758532845745));
#46931=CARTESIAN_POINT('Ctrl Pts',(-0.0121236512499408,-0.0340478734955391,
-0.0136401406390158));
#46932=CARTESIAN_POINT('Ctrl Pts',(-0.0117638250240851,-0.0340691432052548,
-0.0134976683943288));
#46933=CARTESIAN_POINT('Ctrl Pts',(-0.0115960720806594,-0.0340802288666755,
-0.013389141204316));
#46934=CARTESIAN_POINT('Ctrl Pts',(-0.0113142518625794,-0.0341014011359788,
-0.0131150664457129));
#46935=CARTESIAN_POINT('Ctrl Pts',(-0.0112022250916371,-0.0341106019315912,
-0.0129529575356181));
#46936=CARTESIAN_POINT('Ctrl Pts',(-0.0110475431979664,-0.0341303674670227,
-0.0125971778978506));
#46937=CARTESIAN_POINT('Ctrl Pts',(-0.0110054879022801,-0.0341409169782053,
-0.0124072866965642));
#46938=CARTESIAN_POINT('Ctrl Pts',(-0.010995318766936,-0.0341627437959899,
-0.0120144039764405));
#46939=CARTESIAN_POINT('Ctrl Pts',(-0.0110303050087293,-0.034173816303497,
-0.0118150988413109));
#46940=CARTESIAN_POINT('Ctrl Pts',(-0.0111730157058391,-0.0341940474243758,
-0.0114509386654922));
#46941=CARTESIAN_POINT('Ctrl Pts',(-0.0112758407392223,-0.0342028657695953,
-0.0112882575802964));
#46942=CARTESIAN_POINT('Ctrl Pts',(-0.0115398596303183,-0.0342233802192822,
-0.011007031525106));
#46943=CARTESIAN_POINT('Ctrl Pts',(-0.0116997428790087,-0.0342342605120498,
-0.0108922668954815));
#46944=CARTESIAN_POINT('Ctrl Pts',(-0.0120579139564312,-0.0342560348160953,
-0.0107287624537415));
#46945=CARTESIAN_POINT('Ctrl Pts',(-0.012253386118002,-0.0342667116541822,
-0.0106829639979216));
#46946=CARTESIAN_POINT('Ctrl Pts',(-0.0126420686172139,-0.0342857569317473,
-0.0106705518422238));
#46947=CARTESIAN_POINT('Ctrl Pts',(-0.0128314895662413,-0.0342954115800285,
-0.0107006353612827));
#46948=CARTESIAN_POINT('Ctrl Pts',(-0.0131957868781216,-0.0343165997280838,
-0.0108324272380366));
#46949=CARTESIAN_POINT('Ctrl Pts',(-0.0133662400961577,-0.0343276630498013,
-0.0109354731859148));
#46950=CARTESIAN_POINT('Ctrl Pts',(-0.013657220492716,-0.0343490489513218,
-0.0112013728098045));
#46951=CARTESIAN_POINT('Ctrl Pts',(-0.01377497883035,-0.034358532105937,
-0.0113614921757279));
#46952=CARTESIAN_POINT('Ctrl Pts',(-0.0139399619394467,-0.0343781072737967,
-0.0117138451972016));
#46953=CARTESIAN_POINT('Ctrl Pts',(-0.0139872438660849,-0.0343885570083426,
-0.0119019404190269));
#46954=CARTESIAN_POINT('Ctrl Pts',(-0.0140086792973725,-0.0344102956305679,
-0.0122932356190815));
#46955=CARTESIAN_POINT('Ctrl Pts',(-0.0139796637894866,-0.0344213864533069,
-0.0124928704283847));
#46956=CARTESIAN_POINT('Ctrl Pts',(-0.0138479122117746,-0.034441853337423,
-0.0128612743424733));
#46957=CARTESIAN_POINT('Ctrl Pts',(-0.0137495149095708,-0.0344506485758436,
-0.0130275472897237));
#46958=CARTESIAN_POINT('Ctrl Pts',(-0.0134935269297074,-0.0344709867383029,
-0.013316336951008));
#46959=CARTESIAN_POINT('Ctrl Pts',(-0.0133375088719449,-0.0344817994644339,
-0.0134353638887793));
#46960=CARTESIAN_POINT('Ctrl Pts',(-0.0129848179956392,-0.0345035970449082,
-0.013609198268725));
#46961=CARTESIAN_POINT('Ctrl Pts',(-0.0127907563166154,-0.0345143666899402,
-0.0136607808020066));
#46962=CARTESIAN_POINT('Ctrl Pts',(-0.012561509598585,-0.0345257887586781,
-0.0136749083134762));
#46963=CARTESIAN_POINT('Ctrl Pts',(-0.0125307407466012,-0.0345272953750118,
-0.0136758532865583));
#46964=CARTESIAN_POINT('Ctrl Pts',(-0.0125000000000001,-0.0345287743898722,
-0.0136758532865583));
#46965=CARTESIAN_POINT('Ctrl Pts',(-0.0125,-0.0345912743898723,-0.0136758532865583));
#46966=CARTESIAN_POINT('Ctrl Pts',(-0.01251620762298,-0.0345904946002481,
-0.0136758532865583));
#46967=CARTESIAN_POINT('Ctrl Pts',(-0.0125324247338042,-0.034589707057313,
-0.0136755906007887));
#46968=CARTESIAN_POINT('Ctrl Pts',(-0.0127473797303576,-0.034579171289561,
-0.0136686159370902));
#46969=CARTESIAN_POINT('Ctrl Pts',(-0.0129428289865807,-0.0345684927632912,
-0.0136227170334578));
#46970=CARTESIAN_POINT('Ctrl Pts',(-0.0133009077920266,-0.0345467178909423,
-0.0134590323130444));
#46971=CARTESIAN_POINT('Ctrl Pts',(-0.0134607251051158,-0.0345358386922668,
-0.0133441928669241));
#46972=CARTESIAN_POINT('Ctrl Pts',(-0.0137246055465384,-0.0345153272546697,
-0.0130628354450979));
#46973=CARTESIAN_POINT('Ctrl Pts',(-0.0138273542447476,-0.0345065099366744,
-0.0129000931289942));
#46974=CARTESIAN_POINT('Ctrl Pts',(-0.0139698771363575,-0.0344862747102172,
-0.0125358590527656));
#46975=CARTESIAN_POINT('Ctrl Pts',(-0.0140047607596412,-0.0344752018073557,
-0.0123365468012601));
#46976=CARTESIAN_POINT('Ctrl Pts',(-0.0139943975013312,-0.0344533763559891,
-0.0119436886766608));
#46977=CARTESIAN_POINT('Ctrl Pts',(-0.0139522519045707,-0.034442828491156,
-0.0117538271096656));
#46978=CARTESIAN_POINT('Ctrl Pts',(-0.0137973933362267,-0.0344230661827964,
-0.0113981055591923));
#46979=CARTESIAN_POINT('Ctrl Pts',(-0.0136852694656437,-0.0344138611748065,
-0.0112360306090336));
#46980=CARTESIAN_POINT('Ctrl Pts',(-0.0134032924649268,-0.034392685196546,
-0.0109620938834637));
#46981=CARTESIAN_POINT('Ctrl Pts',(-0.0132354920479945,-0.0343815998314314,
-0.0108536595869972));
#46982=CARTESIAN_POINT('Ctrl Pts',(-0.0128742859884516,-0.034360254469438,
-0.0107108538023672));
#46983=CARTESIAN_POINT('Ctrl Pts',(-0.0126854032092023,-0.0343502120395477,
-0.0106752256764677));
#46984=CARTESIAN_POINT('Ctrl Pts',(-0.0122961866848581,-0.0343314497403325,
-0.0106765256529042));
#46985=CARTESIAN_POINT('Ctrl Pts',(-0.0120995215228156,-0.034320871585718,
-0.0107167051662914));
#46986=CARTESIAN_POINT('Ctrl Pts',(-0.0117363500058537,-0.0342991382017244,
-0.010870075470822));
#46987=CARTESIAN_POINT('Ctrl Pts',(-0.0115728444058113,-0.0342882011203275,
-0.0109806103945126));
#46988=CARTESIAN_POINT('Ctrl Pts',(-0.0113011329345216,-0.034267520847394,
-0.0112544821468481));
#46989=CARTESIAN_POINT('Ctrl Pts',(-0.0111940630273294,-0.0342586107963544,
-0.0114137979698795));
#46990=CARTESIAN_POINT('Ctrl Pts',(-0.011040978195299,-0.0342386099278618,
-0.0117738136027466));
#46991=CARTESIAN_POINT('Ctrl Pts',(-0.0110003103750975,-0.0342275637077669,
-0.0119726455644544));
#46992=CARTESIAN_POINT('Ctrl Pts',(-0.0109997050066188,-0.034205669388615,
-0.0123667433091882));
#46993=CARTESIAN_POINT('Ctrl Pts',(-0.0110367350121909,-0.034195032464366,
-0.0125582079456697));
#46994=CARTESIAN_POINT('Ctrl Pts',(-0.0111816501095527,-0.0341750905799763,
-0.0129171618646849));
#46995=CARTESIAN_POINT('Ctrl Pts',(-0.0112883728258302,-0.0341660885615832,
-0.013081142930457));
#46996=CARTESIAN_POINT('Ctrl Pts',(-0.0115615464491464,-0.0341451235360998,
-0.0133627332529875));
#46997=CARTESIAN_POINT('Ctrl Pts',(-0.0117266150624285,-0.0341340261166963,
-0.0134763331265757));
#46998=CARTESIAN_POINT('Ctrl Pts',(-0.0120845161041907,-0.0341125447318022,
-0.0136297601943475));
#46999=CARTESIAN_POINT('Ctrl Pts',(-0.0122728385334754,-0.0341023438157408,
-0.0136708091568324));
#47000=CARTESIAN_POINT('Ctrl Pts',(-0.0124758844978791,-0.0340924386841435,
-0.0136757079677189));
#47001=CARTESIAN_POINT('Ctrl Pts',(-0.0124879451577319,-0.0340918543787413,
-0.0136758532865583));
#47002=CARTESIAN_POINT('Ctrl Pts',(-0.0125,-0.0340912743898723,-0.0136758532865583));
#47003=CARTESIAN_POINT('Origin',(-0.0125,-0.0332787743898722,-0.0121758532865583));
#47004=CARTESIAN_POINT('',(-0.0125000000000001,-0.0335912743898723,-0.0110006128129775));
#47005=CARTESIAN_POINT('',(-0.0124999999999998,-0.0335287743898722,-0.0110006128129775));
#47006=CARTESIAN_POINT('',(-0.0125,-0.0332787743898722,-0.0110006128129775));
#47007=CARTESIAN_POINT('',(-0.0126906536866924,-0.033329014863453,-0.013335526232907));
#47008=CARTESIAN_POINT('Ctrl Pts',(-0.0125000000000001,-0.0335912743898723,
-0.0110006128129775));
#47009=CARTESIAN_POINT('Ctrl Pts',(-0.0123606182656347,-0.0335827152817934,
-0.0110006128129774));
#47010=CARTESIAN_POINT('Ctrl Pts',(-0.0122221996424511,-0.0335733364717449,
-0.011025401296828));
#47011=CARTESIAN_POINT('Ctrl Pts',(-0.0119468498475538,-0.0335528060058356,
-0.0111275590896844));
#47012=CARTESIAN_POINT('Ctrl Pts',(-0.0118144159874647,-0.0335417874032893,
-0.0112089650995605));
#47013=CARTESIAN_POINT('Ctrl Pts',(-0.0115921511920793,-0.033520840775346,
-0.0114148069798741));
#47014=CARTESIAN_POINT('Ctrl Pts',(-0.0115031316668629,-0.0335116561249178,
-0.0115358398651166));
#47015=CARTESIAN_POINT('Ctrl Pts',(-0.0113719732613067,-0.0334921407827157,
-0.011811062505257));
#47016=CARTESIAN_POINT('Ctrl Pts',(-0.011333585454047,-0.0334813115339317,
-0.0119637861628906));
#47017=CARTESIAN_POINT('Ctrl Pts',(-0.0113188148773676,-0.0334594912885804,
-0.0122715145886542));
#47018=CARTESIAN_POINT('Ctrl Pts',(-0.0113411116867082,-0.033448712895394,
-0.0124235210356094));
#47019=CARTESIAN_POINT('Ctrl Pts',(-0.0114419111410691,-0.0334284655664098,
-0.0127090668016587));
#47020=CARTESIAN_POINT('Ctrl Pts',(-0.0115188437531633,-0.0334196421390437,
-0.0128400834142289));
#47021=CARTESIAN_POINT('Ctrl Pts',(-0.0117218265531614,-0.0333990144974729,
-0.0130703254335343));
#47022=CARTESIAN_POINT('Ctrl Pts',(-0.0118475770209433,-0.0333879080103003,
-0.0131657862721312));
#47023=CARTESIAN_POINT('Ctrl Pts',(-0.0120986057939069,-0.0333681883958016,
-0.0132871986211697));
#47024=CARTESIAN_POINT('Ctrl Pts',(-0.0122166059982005,-0.0333596736347119,
-0.0133229816765623));
#47025=CARTESIAN_POINT('Ctrl Pts',(-0.0124551250412871,-0.0333438499456641,
-0.0133561739308117));
#47026=CARTESIAN_POINT('Ctrl Pts',(-0.0125739752653183,-0.0333368598974044,
-0.0133547085129306));
#47027=CARTESIAN_POINT('Ctrl Pts',(-0.0126906536866942,-0.0333290148634529,
-0.0133355262329067));
#47028=CARTESIAN_POINT('',(-0.0118107823295574,-0.033329014863453,-0.013127782471683));
#47029=CARTESIAN_POINT('Origin',(-0.0125,-0.0333290148634431,-0.0121758532865683));
#47030=CARTESIAN_POINT('Ctrl Pts',(-0.0118107823295574,-0.033329014863453,
-0.013127782471683));
#47031=CARTESIAN_POINT('Ctrl Pts',(-0.0117328566913963,-0.0333358003910761,
-0.0130713625954565));
#47032=CARTESIAN_POINT('Ctrl Pts',(-0.0116621427476965,-0.0333424750213042,
-0.0130055796445843));
#47033=CARTESIAN_POINT('Ctrl Pts',(-0.0115406222582317,-0.0333550646124425,
-0.0128609601772603));
#47034=CARTESIAN_POINT('Ctrl Pts',(-0.0114896421085979,-0.0333607045471329,
-0.0127832623550946));
#47035=CARTESIAN_POINT('Ctrl Pts',(-0.0113811872311915,-0.0333761238757399,
-0.0125658053264422));
#47036=CARTESIAN_POINT('Ctrl Pts',(-0.011340535452318,-0.033386489009944,
-0.012419627023673));
#47037=CARTESIAN_POINT('Ctrl Pts',(-0.0113160342671908,-0.0334081534624427,
-0.0121140957267005));
#47038=CARTESIAN_POINT('Ctrl Pts',(-0.0113347125284062,-0.0334192615619009,
-0.0119574394698863));
#47039=CARTESIAN_POINT('Ctrl Pts',(-0.0114305459831103,-0.0334399437325939,
-0.0116657611809258));
#47040=CARTESIAN_POINT('Ctrl Pts',(-0.0115047157059423,-0.0334487832102545,
-0.0115329427712829));
#47041=CARTESIAN_POINT('Ctrl Pts',(-0.0117001104984668,-0.0334689877424058,
-0.0113014920650536));
#47042=CARTESIAN_POINT('Ctrl Pts',(-0.0118198666538377,-0.0334797477308066,
-0.011205422037943));
#47043=CARTESIAN_POINT('Ctrl Pts',(-0.0120926769324657,-0.033501567971333,
-0.0110624865859171));
#47044=CARTESIAN_POINT('Ctrl Pts',(-0.0122438352623582,-0.0335124163458775,
-0.0110183137211824));
#47045=CARTESIAN_POINT('Ctrl Pts',(-0.0124327970500069,-0.0335245965763909,
-0.0110020523410354));
#47046=CARTESIAN_POINT('Ctrl Pts',(-0.0124664153270286,-0.0335267120332294,
-0.0110006128129775));
#47047=CARTESIAN_POINT('Ctrl Pts',(-0.0124999999999996,-0.0335287743898722,
-0.0110006128129775));
#47048=CARTESIAN_POINT('Origin',(-0.0125,-0.0332787743898722,-0.0121758532865583));
#47049=CARTESIAN_POINT('',(-0.0125,-0.0340912743898723,-0.0110006128129774));
#47050=CARTESIAN_POINT('',(-0.0124999999999999,-0.0340287743898722,-0.0110006128129774));
#47051=CARTESIAN_POINT('',(-0.0125,-0.0332787743898722,-0.0110006128129775));
#47052=CARTESIAN_POINT('Ctrl Pts',(-0.0125,-0.0340912743898723,-0.0110006128129774));
#47053=CARTESIAN_POINT('Ctrl Pts',(-0.0124960756575115,-0.0340910334051288,
-0.0110006128129774));
#47054=CARTESIAN_POINT('Ctrl Pts',(-0.0124921505656907,-0.034090791677487,
-0.0110006324691183));
#47055=CARTESIAN_POINT('Ctrl Pts',(-0.0123323264010234,-0.0340809204712669,
-0.0110022338813871));
#47056=CARTESIAN_POINT('Ctrl Pts',(-0.0121783321910986,-0.0340703094181835,
-0.0110348010229487));
#47057=CARTESIAN_POINT('Ctrl Pts',(-0.0118945028923491,-0.03404854722475,
-0.0111570137092445));
#47058=CARTESIAN_POINT('Ctrl Pts',(-0.0117669768468642,-0.0340376130145685,
-0.0112445399516225));
#47059=CARTESIAN_POINT('Ctrl Pts',(-0.0115554391496173,-0.0340169553720472,
-0.0114608106541898));
#47060=CARTESIAN_POINT('Ctrl Pts',(-0.0114723627009985,-0.0340080699165182,
-0.0115864157522107));
#47061=CARTESIAN_POINT('Ctrl Pts',(-0.0113544964578955,-0.0339879909906153,
-0.0118695865488572));
#47062=CARTESIAN_POINT('Ctrl Pts',(-0.0113238269325546,-0.0339769287177227,
-0.0120255965188557));
#47063=CARTESIAN_POINT('Ctrl Pts',(-0.0113256989701605,-0.0339550347126428,
-0.0123343651696396));
#47064=CARTESIAN_POINT('Ctrl Pts',(-0.0113558598489915,-0.0339444113894496,
-0.0124841846822066));
#47065=CARTESIAN_POINT('Ctrl Pts',(-0.0114717278904493,-0.0339245026676132,
-0.0127649551103596));
#47066=CARTESIAN_POINT('Ctrl Pts',(-0.0115566133573988,-0.0339154439189668,
-0.0128930785763459));
#47067=CARTESIAN_POINT('Ctrl Pts',(-0.0117728436441561,-0.0338943996582683,
-0.0131121263393762));
#47068=CARTESIAN_POINT('Ctrl Pts',(-0.0119029408615713,-0.0338832952199362,
-0.0132000005976338));
#47069=CARTESIAN_POINT('Ctrl Pts',(-0.0121843786053174,-0.0338618376170957,
-0.0133177643660779));
#47070=CARTESIAN_POINT('Ctrl Pts',(-0.0123322121926354,-0.0338516645398618,
-0.0133486485723279));
#47071=CARTESIAN_POINT('Ctrl Pts',(-0.0126376803750815,-0.0338327396235902,
-0.0133533540217116));
#47072=CARTESIAN_POINT('Ctrl Pts',(-0.0127924795143073,-0.0338223800324146,
-0.0133247532125323));
#47073=CARTESIAN_POINT('Ctrl Pts',(-0.0130798021287743,-0.0338006531586729,
-0.0132095873456977));
#47074=CARTESIAN_POINT('Ctrl Pts',(-0.013209789910203,-0.0337896738409785,
-0.0131250526628537));
#47075=CARTESIAN_POINT('Ctrl Pts',(-0.013426646557467,-0.0337688716315349,
-0.0129139170303992));
#47076=CARTESIAN_POINT('Ctrl Pts',(-0.0135126638660378,-0.033759864506462,
-0.012790599717729));
#47077=CARTESIAN_POINT('Ctrl Pts',(-0.0136368875227898,-0.0337401111985121,
-0.0125120210738503));
#47078=CARTESIAN_POINT('Ctrl Pts',(-0.0136714076205765,-0.033729215140356,
-0.0123583552112813));
#47079=CARTESIAN_POINT('Ctrl Pts',(-0.0136783772259481,-0.0337074000407905,
-0.0120506993559462));
#47080=CARTESIAN_POINT('Ctrl Pts',(-0.0136523764604824,-0.0336966907224385,
-0.0118996670634857));
#47081=CARTESIAN_POINT('Ctrl Pts',(-0.0135445189826161,-0.0336765999644974,
-0.0116163294009577));
#47082=CARTESIAN_POINT('Ctrl Pts',(-0.0134639062296177,-0.033667698154565,
-0.0114866694833925));
#47083=CARTESIAN_POINT('Ctrl Pts',(-0.0132547377211007,-0.0336468736678169,
-0.0112615892554586));
#47084=CARTESIAN_POINT('Ctrl Pts',(-0.0131269116311139,-0.0336357639483301,
-0.0111696323300625));
#47085=CARTESIAN_POINT('Ctrl Pts',(-0.0128482089187027,-0.0336141739931157,
-0.0110433982475888));
#47086=CARTESIAN_POINT('Ctrl Pts',(-0.0127008963514952,-0.0336038806845843,
-0.011008220391548));
#47087=CARTESIAN_POINT('Ctrl Pts',(-0.0125339405954373,-0.0335933716248387,
-0.0110009801072019));
#47088=CARTESIAN_POINT('Ctrl Pts',(-0.0125169639503397,-0.0335923161066012,
-0.0110006128129775));
#47089=CARTESIAN_POINT('Ctrl Pts',(-0.0125000000000001,-0.0335912743898723,
-0.0110006128129775));
#47090=CARTESIAN_POINT('Ctrl Pts',(-0.0124999999999996,-0.0335287743898722,
-0.0110006128129775));
#47091=CARTESIAN_POINT('Ctrl Pts',(-0.0126148986869939,-0.0335358300509642,
-0.0110006128129775));
#47092=CARTESIAN_POINT('Ctrl Pts',(-0.0127293308609662,-0.0335434541633367,
-0.011017454444084));
#47093=CARTESIAN_POINT('Ctrl Pts',(-0.012986994847461,-0.0335620348809274,
-0.0110952508003727));
#47094=CARTESIAN_POINT('Ctrl Pts',(-0.0131241327667588,-0.0335730432997486,
-0.0111682219008775));
#47095=CARTESIAN_POINT('Ctrl Pts',(-0.0133650044577329,-0.0335948077276303,
-0.0113649023707454));
#47096=CARTESIAN_POINT('Ctrl Pts',(-0.0134654911485693,-0.0336049736271007,
-0.0114876217079503));
#47097=CARTESIAN_POINT('Ctrl Pts',(-0.0136090293070465,-0.0336242176119487,
-0.0117590174263455));
#47098=CARTESIAN_POINT('Ctrl Pts',(-0.0136531133265856,-0.0336344847740661,
-0.0119038140399763));
#47099=CARTESIAN_POINT('Ctrl Pts',(-0.0136850907754152,-0.0336560467161619,
-0.0122078996444548));
#47100=CARTESIAN_POINT('Ctrl Pts',(-0.0136704101812334,-0.0336671560908242,
-0.012364573885327));
#47101=CARTESIAN_POINT('Ctrl Pts',(-0.0135820169627469,-0.0336880302264316,
-0.0126589594335283));
#47102=CARTESIAN_POINT('Ctrl Pts',(-0.0135108076846844,-0.0336969609151749,
-0.0127942518647259));
#47103=CARTESIAN_POINT('Ctrl Pts',(-0.0133207509146878,-0.0337170112452909,
-0.0130305989098306));
#47104=CARTESIAN_POINT('Ctrl Pts',(-0.0132036492230265,-0.0337277019725857,
-0.0131293130400358));
#47105=CARTESIAN_POINT('Ctrl Pts',(-0.0129347619976434,-0.0337495135035495,
-0.0132787977596712));
#47106=CARTESIAN_POINT('Ctrl Pts',(-0.0127847238389795,-0.033760425425484,
-0.0133267032210376));
#47107=CARTESIAN_POINT('Ctrl Pts',(-0.0124815104404345,-0.0337802385943466,
-0.0133603679201949));
#47108=CARTESIAN_POINT('Ctrl Pts',(-0.0123315782170086,-0.0337892093446016,
-0.0133484828980741));
#47109=CARTESIAN_POINT('Ctrl Pts',(-0.0120398348396179,-0.0338099745512868,
-0.0132680985783555));
#47110=CARTESIAN_POINT('Ctrl Pts',(-0.0119012718128719,-0.033820942856139,
-0.0131987272817984));
#47111=CARTESIAN_POINT('Ctrl Pts',(-0.0116567089731332,-0.0338426823272352,
-0.0130091439945126));
#47112=CARTESIAN_POINT('Ctrl Pts',(-0.0115537661659194,-0.0338531314367685,
-0.0128900650648286));
#47113=CARTESIAN_POINT('Ctrl Pts',(-0.0114034119906524,-0.0338719791266584,
-0.012624258248924));
#47114=CARTESIAN_POINT('Ctrl Pts',(-0.0113553126678132,-0.0338821227434151,
-0.0124812039813923));
#47115=CARTESIAN_POINT('Ctrl Pts',(-0.0113145406433663,-0.0339035466245377,
-0.0121790654350339));
#47116=CARTESIAN_POINT('Ctrl Pts',(-0.0113244949922415,-0.0339146484201904,
-0.0120224980800683));
#47117=CARTESIAN_POINT('Ctrl Pts',(-0.0114040081761379,-0.0339357434184588,
-0.0117249977310072));
#47118=CARTESIAN_POINT('Ctrl Pts',(-0.0114717055415038,-0.0339448493571179,
-0.0115867248514679));
#47119=CARTESIAN_POINT('Ctrl Pts',(-0.0116554621777097,-0.0339647148741365,
-0.0113446784505098));
#47120=CARTESIAN_POINT('Ctrl Pts',(-0.011769387434291,-0.0339753169567894,
-0.0112429628638632));
#47121=CARTESIAN_POINT('Ctrl Pts',(-0.0120346233421407,-0.0339971949315404,
-0.0110852797784763));
#47122=CARTESIAN_POINT('Ctrl Pts',(-0.0121846047606453,-0.034008263962634,
-0.0110328446552472));
#47123=CARTESIAN_POINT('Ctrl Pts',(-0.0123934552532009,-0.0340221034284428,
-0.0110042315111123));
#47124=CARTESIAN_POINT('Ctrl Pts',(-0.0124467484439296,-0.0340255043356872,
-0.0110006128129774));
#47125=CARTESIAN_POINT('Ctrl Pts',(-0.0124999999999998,-0.0340287743898722,
-0.0110006128129774));
#47126=CARTESIAN_POINT('Origin',(-0.0125,-0.0332787743898722,-0.0121758532865583));
#47127=CARTESIAN_POINT('',(-0.0124999999999998,-0.0345912743898723,-0.0110006128129774));
#47128=CARTESIAN_POINT('',(-0.0125000000423485,-0.0345287743950732,-0.0110006128129774));
#47129=CARTESIAN_POINT('',(-0.0125,-0.0332787743898722,-0.0110006128129775));
#47130=CARTESIAN_POINT('Ctrl Pts',(-0.0124999999999997,-0.0345912743898723,
-0.0110006128129774));
#47131=CARTESIAN_POINT('Ctrl Pts',(-0.0124750554773252,-0.0345897426047605,
-0.0110006128129774));
#47132=CARTESIAN_POINT('Ctrl Pts',(-0.0124500886290699,-0.0345881812931068,
-0.0110014069628304));
#47133=CARTESIAN_POINT('Ctrl Pts',(-0.012269495724329,-0.0345766828180498,
-0.0110129342348475));
#47134=CARTESIAN_POINT('Ctrl Pts',(-0.0121174170957439,-0.0345658970309991,
-0.0110537477669458));
#47135=CARTESIAN_POINT('Ctrl Pts',(-0.0118412360152098,-0.034544080492877,
-0.0111907403896408));
#47136=CARTESIAN_POINT('Ctrl Pts',(-0.0117191564965817,-0.0345332637431826,
-0.0112843872296165));
#47137=CARTESIAN_POINT('Ctrl Pts',(-0.0115190236604412,-0.0345129241353354,
-0.0115114413177684));
#47138=CARTESIAN_POINT('Ctrl Pts',(-0.0114422353637598,-0.0345041213979416,
-0.0116421012583143));
#47139=CARTESIAN_POINT('Ctrl Pts',(-0.0113398627879977,-0.0344836129238636,
-0.0119313299237687));
#47140=CARTESIAN_POINT('Ctrl Pts',(-0.0113176466556352,-0.0344725118019906,
-0.0120878877764957));
#47141=CARTESIAN_POINT('Ctrl Pts',(-0.0113355030581801,-0.0344507674845931,
-0.0123945453990058));
#47142=CARTESIAN_POINT('Ctrl Pts',(-0.0113730900707122,-0.0344403206155127,
-0.0125418763993926));
#47143=CARTESIAN_POINT('Ctrl Pts',(-0.0115035277113585,-0.0344207548638443,
-0.0128178099584733));
#47144=CARTESIAN_POINT('Ctrl Pts',(-0.0115964602246692,-0.0344112228445418,
-0.0129431204378604));
#47145=CARTESIAN_POINT('Ctrl Pts',(-0.0118256274042374,-0.0343897908260657,
-0.013150697852471));
#47146=CARTESIAN_POINT('Ctrl Pts',(-0.0119595985074006,-0.034378721487533,
-0.01323087232687));
#47147=CARTESIAN_POINT('Ctrl Pts',(-0.012245671537934,-0.034357537461157,
-0.0133328911078831));
#47148=CARTESIAN_POINT('Ctrl Pts',(-0.0123942878919688,-0.0343479318087532,
-0.0133557726528935));
#47149=CARTESIAN_POINT('Ctrl Pts',(-0.0126989942687216,-0.0343288234442705,
-0.0133445734190455));
#47150=CARTESIAN_POINT('Ctrl Pts',(-0.0128520930281185,-0.0343181215089025,
-0.0133078919067336));
#47151=CARTESIAN_POINT('Ctrl Pts',(-0.0131322163996732,-0.0342963242478649,
-0.0131782712574251));
#47152=CARTESIAN_POINT('Ctrl Pts',(-0.0132570700842285,-0.0342854447960889,
-0.0130876608532056));
#47153=CARTESIAN_POINT('Ctrl Pts',(-0.0134629554352069,-0.0342649434297038,
-0.0128660078886874));
#47154=CARTESIAN_POINT('Ctrl Pts',(-0.0135429143205125,-0.034256129396065,
-0.0127379238827873));
#47155=CARTESIAN_POINT('Ctrl Pts',(-0.013653144077261,-0.0342358355343372,
-0.0124517218707739));
#47156=CARTESIAN_POINT('Ctrl Pts',(-0.0136796361890583,-0.0342247501576865,
-0.0122953860711175));
#47157=CARTESIAN_POINT('Ctrl Pts',(-0.013669846293963,-0.0342029228794306,
-0.0119875584611037));
#47158=CARTESIAN_POINT('Ctrl Pts',(-0.013635997498135,-0.0341923834356137,
-0.0118389218897923));
#47159=CARTESIAN_POINT('Ctrl Pts',(-0.0135129416810887,-0.0341726419863371,
-0.0115605104874276));
#47160=CARTESIAN_POINT('Ctrl Pts',(-0.0134241318189287,-0.034163380193175,
-0.0114337693518147));
#47161=CARTESIAN_POINT('Ctrl Pts',(-0.0132015324683946,-0.034142142524701,
-0.0112202979153486));
#47162=CARTESIAN_POINT('Ctrl Pts',(-0.0130694805575508,-0.0341310512062501,
-0.011136179341794));
#47163=CARTESIAN_POINT('Ctrl Pts',(-0.0127893113962216,-0.0341099946665643,
-0.0110275306197938));
#47164=CARTESIAN_POINT('Ctrl Pts',(-0.01264522667166,-0.0341001924219539,
-0.0110006128129774));
#47165=CARTESIAN_POINT('Ctrl Pts',(-0.0125,-0.0340912743898723,-0.0110006128129774));
#47166=CARTESIAN_POINT('Ctrl Pts',(-0.0124999999999998,-0.0340287743898722,
-0.0110006128129774));
#47167=CARTESIAN_POINT('Ctrl Pts',(-0.0125955056067571,-0.0340346391670188,
-0.0110006128129774));
#47168=CARTESIAN_POINT('Ctrl Pts',(-0.0126908262120928,-0.0340409051371065,
-0.011012249201206));
#47169=CARTESIAN_POINT('Ctrl Pts',(-0.0129324829267262,-0.0340578775172794,
-0.011072406568164));
#47170=CARTESIAN_POINT('Ctrl Pts',(-0.0130724056305593,-0.0340687980883178,
-0.0111380764658867));
#47171=CARTESIAN_POINT('Ctrl Pts',(-0.0133213733388323,-0.0340905710059925,
-0.0113209736836162));
#47172=CARTESIAN_POINT('Ctrl Pts',(-0.013427397961506,-0.034101206621743,
-0.0114373193964856));
#47173=CARTESIAN_POINT('Ctrl Pts',(-0.0135843958313036,-0.0341201202909029,
-0.0116988657373322));
#47174=CARTESIAN_POINT('Ctrl Pts',(-0.0136361543301948,-0.0341299774445908,
-0.01184024768765));
#47175=CARTESIAN_POINT('Ctrl Pts',(-0.013684883456739,-0.0341512708602702,
-0.0121405462947768));
#47176=CARTESIAN_POINT('Ctrl Pts',(-0.0136792146875315,-0.0341623572145446,
-0.0122968958817491));
#47177=CARTESIAN_POINT('Ctrl Pts',(-0.0136078449982781,-0.034183646717213,
-0.0125971393041294));
#47178=CARTESIAN_POINT('Ctrl Pts',(-0.0135433557374113,-0.0341929738714508,
-0.0127381691020281));
#47179=CARTESIAN_POINT('Ctrl Pts',(-0.0133653109219861,-0.0342126692503355,
-0.0129853097894741));
#47180=CARTESIAN_POINT('Ctrl Pts',(-0.013254300345489,-0.0342231848416828,
-0.0130896341961224));
#47181=CARTESIAN_POINT('Ctrl Pts',(-0.0129939293247358,-0.0342449915957543,
-0.0132537346789326));
#47182=CARTESIAN_POINT('Ctrl Pts',(-0.0128457982073995,-0.0342560819201148,
-0.0133099752108118));
#47183=CARTESIAN_POINT('Ctrl Pts',(-0.0125431626361086,-0.0342764331401208,
-0.0133598168836629));
#47184=CARTESIAN_POINT('Ctrl Pts',(-0.0123920925090513,-0.0342852381394321,
-0.0133556799747317));
#47185=CARTESIAN_POINT('Ctrl Pts',(-0.0120967084097093,-0.0343056968533139,
-0.0132902464363481));
#47186=CARTESIAN_POINT('Ctrl Pts',(-0.0119554696453631,-0.0343165603444115,
-0.0132284660060567));
#47187=CARTESIAN_POINT('Ctrl Pts',(-0.0117019596409682,-0.0343383643191689,
-0.0130525602870196));
#47188=CARTESIAN_POINT('Ctrl Pts',(-0.011592818912802,-0.0343490893486699,
-0.0129390898433797));
#47189=CARTESIAN_POINT('Ctrl Pts',(-0.0114289320733949,-0.0343682679614312,
-0.0126820026092625));
#47190=CARTESIAN_POINT('Ctrl Pts',(-0.0113734465632184,-0.0343777906865557,
-0.0125422984840514));
#47191=CARTESIAN_POINT('Ctrl Pts',(-0.0113166127250521,-0.034398934582652,
-0.0122441085345134));
#47192=CARTESIAN_POINT('Ctrl Pts',(-0.0113178982285662,-0.0344099966351187,
-0.012088101673157));
#47193=CARTESIAN_POINT('Ctrl Pts',(-0.0113808354132985,-0.0344314792774952,
-0.0117851344235536));
#47194=CARTESIAN_POINT('Ctrl Pts',(-0.0114420075582455,-0.0344410932807145,
-0.0116412294678506));
#47195=CARTESIAN_POINT('Ctrl Pts',(-0.0116142017157204,-0.0344606118760316,
-0.0113889414604652));
#47196=CARTESIAN_POINT('Ctrl Pts',(-0.011722198372666,-0.0344710331859705,
-0.0112820560718705));
#47197=CARTESIAN_POINT('Ctrl Pts',(-0.0119774849513258,-0.0344927531395949,
-0.0111115973505905));
#47198=CARTESIAN_POINT('Ctrl Pts',(-0.0121236464354651,-0.0345038570820486,
-0.0110515612051203));
#47199=CARTESIAN_POINT('Ctrl Pts',(-0.0123508526918609,-0.0345193639805299,
-0.0110077099518364));
#47200=CARTESIAN_POINT('Ctrl Pts',(-0.012425419189096,-0.0345241945556681,
-0.0110006128102796));
#47201=CARTESIAN_POINT('Ctrl Pts',(-0.012500000042512,-0.0345287743924827,
-0.0110006128129774));
#47202=CARTESIAN_POINT('Origin',(-0.0125,-0.0332787743898722,-0.0121758532865583));
#47203=CARTESIAN_POINT('',(-0.0124999999999998,-0.0350912743898722,-0.0110006128129774));
#47204=CARTESIAN_POINT('',(-0.0125000000000001,-0.0350287743898722,-0.0110006128129774));
#47205=CARTESIAN_POINT('',(-0.0125,-0.0332787743898722,-0.0110006128129775));
#47206=CARTESIAN_POINT('Ctrl Pts',(-0.0124999999999996,-0.0350912743898722,
-0.0110006128129774));
#47207=CARTESIAN_POINT('Ctrl Pts',(-0.0124552876665998,-0.0350885287094876,
-0.0110006128129774));
#47208=CARTESIAN_POINT('Ctrl Pts',(-0.0124105325232473,-0.0350856899460719,
-0.011003164142657));
#47209=CARTESIAN_POINT('Ctrl Pts',(-0.0122109721925805,-0.0350726230844953,
-0.0110260764208655));
#47210=CARTESIAN_POINT('Ctrl Pts',(-0.0120611117066231,-0.0350617021504674,
-0.0110745438134338));
#47211=CARTESIAN_POINT('Ctrl Pts',(-0.0117928315208616,-0.0350398931158629,
-0.0112250095448001));
#47212=CARTESIAN_POINT('Ctrl Pts',(-0.0116761362008922,-0.0350292133877324,
-0.0113241172915062));
#47213=CARTESIAN_POINT('Ctrl Pts',(-0.0114868904033686,-0.0350091866776769,
-0.0115612027601145));
#47214=CARTESIAN_POINT('Ctrl Pts',(-0.0114161319308057,-0.0350002375159901,
-0.0116968752014844));
#47215=CARTESIAN_POINT('Ctrl Pts',(-0.0113288757678491,-0.0349793345953434,
-0.0119916667018041));
#47216=CARTESIAN_POINT('Ctrl Pts',(-0.0113148032167167,-0.0349682256427751,
-0.0121483349899323));
#47217=CARTESIAN_POINT('Ctrl Pts',(-0.011347914804051,-0.0349466804359757,
-0.0124521845784391));
#47218=CARTESIAN_POINT('Ctrl Pts',(-0.0113925179879937,-0.0349364286986426,
-0.0125967636580998));
#47219=CARTESIAN_POINT('Ctrl Pts',(-0.0115371196843806,-0.0349172114068112,
-0.0128677829279349));
#47220=CARTESIAN_POINT('Ctrl Pts',(-0.0116382332305663,-0.0349069854009331,
-0.0129902878348671));
#47221=CARTESIAN_POINT('Ctrl Pts',(-0.0118800569666037,-0.0348851947755575,
-0.0131860582348388));
#47222=CARTESIAN_POINT('Ctrl Pts',(-0.0120174377737695,-0.0348741925574974,
-0.0132584337439644));
#47223=CARTESIAN_POINT('Ctrl Pts',(-0.0123076663604168,-0.0348533088805891,
-0.0133447833022396));
#47224=CARTESIAN_POINT('Ctrl Pts',(-0.012457197589519,-0.0348442086648951,
-0.0133597213009138));
#47225=CARTESIAN_POINT('Ctrl Pts',(-0.0127608903301276,-0.0348245887360935,
-0.0133323373315443));
#47226=CARTESIAN_POINT('Ctrl Pts',(-0.0129118703237368,-0.0348137293994736,
-0.0132875463855168));
#47227=CARTESIAN_POINT('Ctrl Pts',(-0.0131840440009712,-0.0347919096621732,
-0.0131435225014095));
#47228=CARTESIAN_POINT('Ctrl Pts',(-0.0133033659481531,-0.0347811606893557,
-0.0130470111066754));
#47229=CARTESIAN_POINT('Ctrl Pts',(-0.0134978824727176,-0.0347609813752259,
-0.0128147504894661));
#47230=CARTESIAN_POINT('Ctrl Pts',(-0.0135715657997223,-0.0347521305278522,
-0.0126815283015197));
#47231=CARTESIAN_POINT('Ctrl Pts',(-0.01366618036253,-0.0347314164816825,
-0.0123894004763574));
#47232=CARTESIAN_POINT('Ctrl Pts',(-0.0136842015515831,-0.0347203076904613,
-0.0122327344636891));
#47233=CARTESIAN_POINT('Ctrl Pts',(-0.013658469194559,-0.0346986591920476,
-0.011927428165352));
#47234=CARTESIAN_POINT('Ctrl Pts',(-0.0136172510282482,-0.0346883097513367,
-0.0117814711861244));
#47235=CARTESIAN_POINT('Ctrl Pts',(-0.0134795375287987,-0.0346689211106175,
-0.0115080354025123));
#47236=CARTESIAN_POINT('Ctrl Pts',(-0.0133824475650228,-0.0346590613965485,
-0.0113841536072333));
#47237=CARTESIAN_POINT('Ctrl Pts',(-0.0131467858703251,-0.0346374426253905,
-0.0111825575193544));
#47238=CARTESIAN_POINT('Ctrl Pts',(-0.0130110166597482,-0.0346264036088737,
-0.0111063527141999));
#47239=CARTESIAN_POINT('Ctrl Pts',(-0.0127465686445372,-0.0346071066042064,
-0.0110201032108124));
#47240=CARTESIAN_POINT('Ctrl Pts',(-0.0126236004277015,-0.0345988644046192,
-0.0110006128129774));
#47241=CARTESIAN_POINT('Ctrl Pts',(-0.0124999999999997,-0.0345912743898723,
-0.0110006128129774));
#47242=CARTESIAN_POINT('Ctrl Pts',(-0.012500000042512,-0.0345287743924827,
-0.0110006128129774));
#47243=CARTESIAN_POINT('Ctrl Pts',(-0.0125751211765788,-0.034533387406676,
-0.0110006128156948));
#47244=CARTESIAN_POINT('Ctrl Pts',(-0.0126502252123126,-0.0345382546490307,
-0.0110078131349879));
#47245=CARTESIAN_POINT('Ctrl Pts',(-0.0128738424439069,-0.0345535279388742,
-0.011051291649753));
#47246=CARTESIAN_POINT('Ctrl Pts',(-0.013016290332032,-0.0345643270592042,
-0.0111091621890696));
#47247=CARTESIAN_POINT('Ctrl Pts',(-0.0132741421697673,-0.0345861459630291,
-0.0112779687180286));
#47248=CARTESIAN_POINT('Ctrl Pts',(-0.0133863167557866,-0.0345969523672073,
-0.0113884796012615));
#47249=CARTESIAN_POINT('Ctrl Pts',(-0.0135570436862805,-0.0346163907559161,
-0.0116410466310697));
#47250=CARTESIAN_POINT('Ctrl Pts',(-0.0136162397705058,-0.0346256438448179,
-0.0117791314254577));
#47251=CARTESIAN_POINT('Ctrl Pts',(-0.013681017378618,-0.0346466362775183,
-0.0120751853040379));
#47252=CARTESIAN_POINT('Ctrl Pts',(-0.0136840279483189,-0.0346576660579381,
-0.0122307370364074));
#47253=CARTESIAN_POINT('Ctrl Pts',(-0.0136294701515449,-0.0346793321314919,
-0.0125362911949342));
#47254=CARTESIAN_POINT('Ctrl Pts',(-0.0135715964158634,-0.0346892862043902,
-0.0126830698979639));
#47255=CARTESIAN_POINT('Ctrl Pts',(-0.0134051543343992,-0.0347086285387393,
-0.0129403492166821));
#47256=CARTESIAN_POINT('Ctrl Pts',(-0.0133001431436326,-0.0347189518902571,
-0.0130496425915515));
#47257=CARTESIAN_POINT('Ctrl Pts',(-0.0130499439073725,-0.0347405734590142,
-0.0132261378272708));
#47258=CARTESIAN_POINT('Ctrl Pts',(-0.0129057865875121,-0.0347516829744878,
-0.0132898024784227));
#47259=CARTESIAN_POINT('Ctrl Pts',(-0.0126058552783491,-0.0347724490275718,
-0.013356028757632));
#47260=CARTESIAN_POINT('Ctrl Pts',(-0.012453463099758,-0.0347813216172268,
-0.0133598515234103));
#47261=CARTESIAN_POINT('Ctrl Pts',(-0.0121546345135361,-0.0348014594615642,
-0.0133094343843143));
#47262=CARTESIAN_POINT('Ctrl Pts',(-0.0120111272940138,-0.0348121900505733,
-0.0132553316395669));
#47263=CARTESIAN_POINT('Ctrl Pts',(-0.0117493005129558,-0.0348340081668068,
-0.0130934321290248));
#47264=CARTESIAN_POINT('Ctrl Pts',(-0.0116342945808522,-0.0348448850404909,
-0.0129858376342885));
#47265=CARTESIAN_POINT('Ctrl Pts',(-0.0114570481241346,-0.0348645678180743,
-0.0127376695784204));
#47266=CARTESIAN_POINT('Ctrl Pts',(-0.0113942990939783,-0.0348736221129475,
-0.0126010874011101));
#47267=CARTESIAN_POINT('Ctrl Pts',(-0.0113220405410279,-0.0348944675692732,
-0.0123071063135395));
#47268=CARTESIAN_POINT('Ctrl Pts',(-0.0113149905895466,-0.0349054592775354,
-0.0121520915084571));
#47269=CARTESIAN_POINT('Ctrl Pts',(-0.0113612936472873,-0.0349271702020729,
-0.0118459048216325));
#47270=CARTESIAN_POINT('Ctrl Pts',(-0.0114150706796611,-0.0349374285204873,
-0.011697940814626));
#47271=CARTESIAN_POINT('Ctrl Pts',(-0.0115739795518052,-0.0349564432998835,
-0.0114368525347288));
#47272=CARTESIAN_POINT('Ctrl Pts',(-0.0116756081885004,-0.0349666504916691,
-0.0113249767791944));
#47273=CARTESIAN_POINT('Ctrl Pts',(-0.0119199856945809,-0.0349881465373255,
-0.0111419384868976));
#47274=CARTESIAN_POINT('Ctrl Pts',(-0.0120618120852735,-0.034999253402818,
-0.0110743112927582));
#47275=CARTESIAN_POINT('Ctrl Pts',(-0.01230684687214,-0.0350164906234034,
-0.0110125348904171));
#47276=CARTESIAN_POINT('Ctrl Pts',(-0.012403329223776,-0.035022838062379,
-0.0110006128129774));
#47277=CARTESIAN_POINT('Ctrl Pts',(-0.0125000000000002,-0.0350287743898722,
-0.0110006128129774));
#47278=CARTESIAN_POINT('Origin',(-0.0125,-0.0332787743898722,-0.0121758532865583));
#47279=CARTESIAN_POINT('',(-0.0125,-0.0355912743898722,-0.0110006128129774));
#47280=CARTESIAN_POINT('',(-0.0125000000000003,-0.0355287743898722,-0.0110006128129774));
#47281=CARTESIAN_POINT('',(-0.0125,-0.0332787743898722,-0.0110006128129775));
#47282=CARTESIAN_POINT('Ctrl Pts',(-0.0125,-0.0355912743898722,-0.0110006128129774));
#47283=CARTESIAN_POINT('Ctrl Pts',(-0.0124345292523923,-0.0355872539835591,
-0.0110006128129774));
#47284=CARTESIAN_POINT('Ctrl Pts',(-0.0123690379077626,-0.035583038398789,
-0.0110060822968235));
#47285=CARTESIAN_POINT('Ctrl Pts',(-0.0121495456404542,-0.0355682449724107,
-0.0110431705401221));
#47286=CARTESIAN_POINT('Ctrl Pts',(-0.0120017074749619,-0.0355571520648707,
-0.0110999913400475));
#47287=CARTESIAN_POINT('Ctrl Pts',(-0.0117420984906089,-0.0355353575437144,
-0.0112650666698114));
#47288=CARTESIAN_POINT('Ctrl Pts',(-0.0116315416578729,-0.0355248558389244,
-0.0113697853026487));
#47289=CARTESIAN_POINT('Ctrl Pts',(-0.0114543809551182,-0.0355051870121528,
-0.0116177083953289));
#47290=CARTESIAN_POINT('Ctrl Pts',(-0.0113903907715994,-0.035495820390194,
-0.0117591694216318));
#47291=CARTESIAN_POINT('Ctrl Pts',(-0.0113202894508321,-0.0354745012951279,
-0.0120598301822132));
#47292=CARTESIAN_POINT('Ctrl Pts',(-0.0113152836457058,-0.0354634180620672,
-0.0122161357510653));
#47293=CARTESIAN_POINT('Ctrl Pts',(-0.011365239104169,-0.0354421469389728,
-0.0125161199684137));
#47294=CARTESIAN_POINT('Ctrl Pts',(-0.0114175580229306,-0.0354323441161254,
-0.0126572463836102));
#47295=CARTESIAN_POINT('Ctrl Pts',(-0.0115755923960375,-0.035413390378229,
-0.0129181276176857));
#47296=CARTESIAN_POINT('Ctrl Pts',(-0.0116820895434152,-0.0354027408413695,
-0.0130340475493773));
#47297=CARTESIAN_POINT('Ctrl Pts',(-0.011931751210611,-0.0353809622357486,
-0.0132159032279045));
#47298=CARTESIAN_POINT('Ctrl Pts',(-0.0120718781108207,-0.0353700497578868,
-0.0132809911728404));
#47299=CARTESIAN_POINT('Ctrl Pts',(-0.0123657072097343,-0.0353494562066715,
-0.013352921241973));
#47300=CARTESIAN_POINT('Ctrl Pts',(-0.012516259401743,-0.0353406074290187,
-0.0133604437247109));
#47301=CARTESIAN_POINT('Ctrl Pts',(-0.0128199445188925,-0.0353204394393541,
-0.0133175880717269));
#47302=CARTESIAN_POINT('Ctrl Pts',(-0.0129696559249467,-0.0353093667370173,
-0.0132645817229708));
#47303=CARTESIAN_POINT('Ctrl Pts',(-0.0132341760342632,-0.0352874984708951,
-0.0131059326775182));
#47304=CARTESIAN_POINT('Ctrl Pts',(-0.0133476704264422,-0.0352769088719306,
-0.0130038229238963));
#47305=CARTESIAN_POINT('Ctrl Pts',(-0.0135305788875744,-0.0352570684653057,
-0.0127610156986414));
#47306=CARTESIAN_POINT('Ctrl Pts',(-0.0135978014977944,-0.0352479333985992,
-0.0126223366674694));
#47307=CARTESIAN_POINT('Ctrl Pts',(-0.0136761109873917,-0.0352268091623596,
-0.0123244239786432));
#47308=CARTESIAN_POINT('Ctrl Pts',(-0.0136854288183076,-0.0352157091431185,
-0.0121678816762062));
#47309=CARTESIAN_POINT('Ctrl Pts',(-0.013643476049991,-0.035194305258746,
-0.0118660251417291));
#47310=CARTESIAN_POINT('Ctrl Pts',(-0.0135948394926351,-0.0351841789224989,
-0.0117232145792489));
#47311=CARTESIAN_POINT('Ctrl Pts',(-0.0134435058323278,-0.0351653763725535,
-0.0114580443668216));
#47312=CARTESIAN_POINT('Ctrl Pts',(-0.013340116020403,-0.0351548738967728,
-0.0113393623320089));
#47313=CARTESIAN_POINT('Ctrl Pts',(-0.0130948822829875,-0.0351331275196624,
-0.011150746284128));
#47314=CARTESIAN_POINT('Ctrl Pts',(-0.0129561133062562,-0.0351221658043202,
-0.0110819175656211));
#47315=CARTESIAN_POINT('Ctrl Pts',(-0.0127074190161277,-0.0351044993361626,
-0.0110143723499798));
#47316=CARTESIAN_POINT('Ctrl Pts',(-0.0126038551037074,-0.0350976518902041,
-0.0110006128129774));
#47317=CARTESIAN_POINT('Ctrl Pts',(-0.0124999999999996,-0.0350912743898722,
-0.0110006128129774));
#47318=CARTESIAN_POINT('Ctrl Pts',(-0.0125000000000002,-0.0350287743898722,
-0.0110006128129774));
#47319=CARTESIAN_POINT('Ctrl Pts',(-0.0125546888212527,-0.0350321327031687,
-0.0110006128129774));
#47320=CARTESIAN_POINT('Ctrl Pts',(-0.012609421191665,-0.0350356290052212,
-0.0110044294629226));
#47321=CARTESIAN_POINT('Ctrl Pts',(-0.012813885449725,-0.0350492050309046,
-0.0110332092561165));
#47322=CARTESIAN_POINT('Ctrl Pts',(-0.0129584415239535,-0.0350598528762727,
-0.0110831614830011));
#47323=CARTESIAN_POINT('Ctrl Pts',(-0.0132257724025345,-0.0350817645774922,
-0.0112381672537046));
#47324=CARTESIAN_POINT('Ctrl Pts',(-0.0133447973984118,-0.0350928181986125,
-0.0113437858235582));
#47325=CARTESIAN_POINT('Ctrl Pts',(-0.0135291034215912,-0.0351128298789464,
-0.0115890033074171));
#47326=CARTESIAN_POINT('Ctrl Pts',(-0.0135952043657725,-0.0351217495110005,
-0.0117242100808198));
#47327=CARTESIAN_POINT('Ctrl Pts',(-0.0136744022935768,-0.035142454939962,
-0.01201621637848));
#47328=CARTESIAN_POINT('Ctrl Pts',(-0.0136851883990951,-0.0351534046726152,
-0.0121706392063467));
#47329=CARTESIAN_POINT('Ctrl Pts',(-0.0136465456508244,-0.0351751527339925,
-0.0124773496297772));
#47330=CARTESIAN_POINT('Ctrl Pts',(-0.0135965142476663,-0.0351857339679876,
-0.0126265755631941));
#47331=CARTESIAN_POINT('Ctrl Pts',(-0.0134443651452701,-0.0352044947311438,
-0.0128911564613117));
#47332=CARTESIAN_POINT('Ctrl Pts',(-0.0133458896582763,-0.0352145712368459,
-0.0130053181706356));
#47333=CARTESIAN_POINT('Ctrl Pts',(-0.0131068203572745,-0.0352359486738981,
-0.013194205096655));
#47334=CARTESIAN_POINT('Ctrl Pts',(-0.0129671948691386,-0.0352470451332583,
-0.0132653508528565));
#47335=CARTESIAN_POINT('Ctrl Pts',(-0.0126704764749306,-0.0352682204812501,
-0.0133486865425982));
#47336=CARTESIAN_POINT('Ctrl Pts',(-0.0125165627929197,-0.0352774099212503,
-0.013360892051278));
#47337=CARTESIAN_POINT('Ctrl Pts',(-0.0122144216837957,-0.0352972060465856,
-0.0133258508181941));
#47338=CARTESIAN_POINT('Ctrl Pts',(-0.0120690292452226,-0.0353077733883185,
-0.0132796178839744));
#47339=CARTESIAN_POINT('Ctrl Pts',(-0.0117985458588359,-0.0353296238447704,
-0.0131317998728765));
#47340=CARTESIAN_POINT('Ctrl Pts',(-0.0116771593965247,-0.0353407025688426,
-0.0130295634347428));
#47341=CARTESIAN_POINT('Ctrl Pts',(-0.0114864993883782,-0.0353609273379629,
-0.0127893410420865));
#47342=CARTESIAN_POINT('Ctrl Pts',(-0.0114167578880609,-0.0353697579334339,
-0.012655583483048));
#47343=CARTESIAN_POINT('Ctrl Pts',(-0.0113301579872456,-0.0353903101380483,
-0.0123657380908379));
#47344=CARTESIAN_POINT('Ctrl Pts',(-0.0113154036292189,-0.0354012080560016,
-0.0122120459997603));
#47345=CARTESIAN_POINT('Ctrl Pts',(-0.011345879036472,-0.0354229957397928,
-0.011904776785957));
#47346=CARTESIAN_POINT('Ctrl Pts',(-0.0113919595530775,-0.0354336692035811,
-0.0117542501463094));
#47347=CARTESIAN_POINT('Ctrl Pts',(-0.011536956117191,-0.0354526927734774,
-0.0114859629147793));
#47348=CARTESIAN_POINT('Ctrl Pts',(-0.0116321417068633,-0.0354624040789343,
-0.0113694639712957));
#47349=CARTESIAN_POINT('Ctrl Pts',(-0.0118654117781541,-0.0354836360779248,
-0.0111746346774902));
#47350=CARTESIAN_POINT('Ctrl Pts',(-0.0120026293927432,-0.0354947134002586,
-0.0110998581365557));
#47351=CARTESIAN_POINT('Ctrl Pts',(-0.0122637927405005,-0.0355136358715802,
-0.0110184834241725));
#47352=CARTESIAN_POINT('Ctrl Pts',(-0.0123816436139273,-0.035521506399523,
-0.0110006128129773));
#47353=CARTESIAN_POINT('Ctrl Pts',(-0.0125000000000005,-0.0355287743898722,
-0.0110006128129774));
#47354=CARTESIAN_POINT('Origin',(-0.0125,-0.0332787743898722,-0.0121758532865583));
#47355=CARTESIAN_POINT('',(-0.0125,-0.0360912743898722,-0.0110006128129774));
#47356=CARTESIAN_POINT('',(-0.0125000000000001,-0.0360287743898721,-0.0110006128129774));
#47357=CARTESIAN_POINT('',(-0.0125,-0.0332787743898722,-0.0110006128129775));
#47358=CARTESIAN_POINT('Ctrl Pts',(-0.0125,-0.0360912743898722,-0.0110006128129774));
#47359=CARTESIAN_POINT('Ctrl Pts',(-0.012413435300456,-0.0360859586530392,
-0.0110006128129774));
#47360=CARTESIAN_POINT('Ctrl Pts',(-0.0123269621105405,-0.036080309589048,
-0.0110101730619216));
#47361=CARTESIAN_POINT('Ctrl Pts',(-0.0120899200069141,-0.0360638632442838,
-0.0110634859351337));
#47362=CARTESIAN_POINT('Ctrl Pts',(-0.0119460639646851,-0.0360527535455263,
-0.0111276775841142));
#47363=CARTESIAN_POINT('Ctrl Pts',(-0.0116966226736852,-0.0360311475618236,
-0.011305046031054));
#47364=CARTESIAN_POINT('Ctrl Pts',(-0.0115920538498495,-0.0360208390958381,
-0.0114146857500023));
#47365=CARTESIAN_POINT('Ctrl Pts',(-0.0114264611124559,-0.0360015229937221,
-0.0116726962754399));
#47366=CARTESIAN_POINT('Ctrl Pts',(-0.01136907791787,-0.0359915139244068,
-0.0118199030163285));
#47367=CARTESIAN_POINT('Ctrl Pts',(-0.0113157648081405,-0.0359698213362853,
-0.0121258311067729));
#47368=CARTESIAN_POINT('Ctrl Pts',(-0.0113194081891567,-0.0359587970230021,
-0.0122813057367389));
#47369=CARTESIAN_POINT('Ctrl Pts',(-0.011385356716575,-0.0359378273196457,
-0.0125770390659802));
#47370=CARTESIAN_POINT('Ctrl Pts',(-0.0114451049974313,-0.0359286089360712,
-0.012714887258803));
#47371=CARTESIAN_POINT('Ctrl Pts',(-0.0116168474225842,-0.035909132270421,
-0.0129667750309259));
#47372=CARTESIAN_POINT('Ctrl Pts',(-0.0117294670069977,-0.0358983144293304,
-0.0130768377412685));
#47373=CARTESIAN_POINT('Ctrl Pts',(-0.0119879486539683,-0.0358764946783662,
-0.0132445773028502));
#47374=CARTESIAN_POINT('Ctrl Pts',(-0.0121305675837105,-0.0358657057712151,
-0.013301863518808));
#47375=CARTESIAN_POINT('Ctrl Pts',(-0.0124279931249051,-0.0358454335983883,
-0.0133584996418362));
#47376=CARTESIAN_POINT('Ctrl Pts',(-0.0125798203026902,-0.0358366175954246,
-0.0133579981003807));
#47377=CARTESIAN_POINT('Ctrl Pts',(-0.0128809190574449,-0.0358160218599593,
-0.0132985978360654));
#47378=CARTESIAN_POINT('Ctrl Pts',(-0.013026776606966,-0.0358049165633889,
-0.0132379970664895));
#47379=CARTESIAN_POINT('Ctrl Pts',(-0.0132812863836961,-0.0357832109116246,
-0.013066596279796));
#47380=CARTESIAN_POINT('Ctrl Pts',(-0.0133888252941528,-0.0357728043328982,
-0.0129593335562388));
#47381=CARTESIAN_POINT('Ctrl Pts',(-0.0135601350121641,-0.0357533126813555,
-0.0127062736247038));
#47382=CARTESIAN_POINT('Ctrl Pts',(-0.013620802551971,-0.0357436500957637,
-0.0125619297372353));
#47383=CARTESIAN_POINT('Ctrl Pts',(-0.0136824570305482,-0.0357221388215468,
-0.01225855869606));
#47384=CARTESIAN_POINT('Ctrl Pts',(-0.0136830809345521,-0.0357110811902516,
-0.0121026141859789));
#47385=CARTESIAN_POINT('Ctrl Pts',(-0.0136250240899294,-0.035689960300378,
-0.0118047486905688));
#47386=CARTESIAN_POINT('Ctrl Pts',(-0.0135689711989981,-0.0356804829095764,
-0.0116652954951538));
#47387=CARTESIAN_POINT('Ctrl Pts',(-0.0134040369024801,-0.0356612642993465,
-0.0114088943505184));
#47388=CARTESIAN_POINT('Ctrl Pts',(-0.0132944275724384,-0.0356505263238068,
-0.0112958703961299));
#47389=CARTESIAN_POINT('Ctrl Pts',(-0.0130402416050823,-0.0356287190275158,
-0.0111210417928692));
#47390=CARTESIAN_POINT('Ctrl Pts',(-0.0128988113017588,-0.035617864895353,
-0.0110598570937938));
#47391=CARTESIAN_POINT('Ctrl Pts',(-0.0126674192887738,-0.0356018724580381,
-0.0110095607862607));
#47392=CARTESIAN_POINT('Ctrl Pts',(-0.0125837461649245,-0.0355964170470507,
-0.0110006128129774));
#47393=CARTESIAN_POINT('Ctrl Pts',(-0.0125,-0.0355912743898722,-0.0110006128129774));
#47394=CARTESIAN_POINT('Ctrl Pts',(-0.0125000000000005,-0.0355287743898722,
-0.0110006128129774));
#47395=CARTESIAN_POINT('Ctrl Pts',(-0.0125352607803295,-0.0355309396723689,
-0.0110006128129774));
#47396=CARTESIAN_POINT('Ctrl Pts',(-0.0125705595312421,-0.0355331635441847,
-0.0110021996029348));
#47397=CARTESIAN_POINT('Ctrl Pts',(-0.0127559944899348,-0.0355451448907968,
-0.0110189599561776));
#47398=CARTESIAN_POINT('Ctrl Pts',(-0.0129021555048979,-0.0355556220749168,
-0.0110613187120238));
#47399=CARTESIAN_POINT('Ctrl Pts',(-0.0131757139460477,-0.0355773945099593,
-0.0112016099180018));
#47400=CARTESIAN_POINT('Ctrl Pts',(-0.0132994550792732,-0.0355884914708227,
-0.0113002823292377));
#47401=CARTESIAN_POINT('Ctrl Pts',(-0.0134966602349332,-0.0356089319691525,
-0.0115352530026169));
#47402=CARTESIAN_POINT('Ctrl Pts',(-0.0135701985822092,-0.0356177315824229,
-0.0116675456934071));
#47403=CARTESIAN_POINT('Ctrl Pts',(-0.013664364715511,-0.0356381230742689,
-0.0119551245718167));
#47404=CARTESIAN_POINT('Ctrl Pts',(-0.0136831514017129,-0.0356489605700093,
-0.0121079645353335));
#47405=CARTESIAN_POINT('Ctrl Pts',(-0.0136610422585882,-0.0356707727365856,
-0.0124155790270557));
#47406=CARTESIAN_POINT('Ctrl Pts',(-0.013619044184284,-0.0356815327234571,
-0.0125673258918548));
#47407=CARTESIAN_POINT('Ctrl Pts',(-0.0134814021934161,-0.0357008204286667,
-0.012839338193513));
#47408=CARTESIAN_POINT('Ctrl Pts',(-0.0133895245057508,-0.035710222753393,
-0.0129582436133824));
#47409=CARTESIAN_POINT('Ctrl Pts',(-0.0131621388582059,-0.0357313036319399,
-0.0131590025594084));
#47410=CARTESIAN_POINT('Ctrl Pts',(-0.0130274454060454,-0.0357423531566018,
-0.013237367023135));
#47411=CARTESIAN_POINT('Ctrl Pts',(-0.012734402148394,-0.0357639135612769,
-0.0133379290568871));
#47412=CARTESIAN_POINT('Ctrl Pts',(-0.0125788408017119,-0.035773663317448,
-0.0133586992261027));
#47413=CARTESIAN_POINT('Ctrl Pts',(-0.0122736417786934,-0.0357931082597812,
-0.0133388598427143));
#47414=CARTESIAN_POINT('Ctrl Pts',(-0.0121268166857713,-0.0358034890875824,
-0.0133003691079313));
#47415=CARTESIAN_POINT('Ctrl Pts',(-0.0118503981711957,-0.0358251693033963,
-0.0131676328089166));
#47416=CARTESIAN_POINT('Ctrl Pts',(-0.0117244118494424,-0.0358362765115161,
-0.013072560146511));
#47417=CARTESIAN_POINT('Ctrl Pts',(-0.011520737759579,-0.0358569263453031,
-0.0128428895278003));
#47418=CARTESIAN_POINT('Ctrl Pts',(-0.0114433966050415,-0.0358657557902617,
-0.0127120252506927));
#47419=CARTESIAN_POINT('Ctrl Pts',(-0.0113418062985382,-0.0358859857536244,
-0.0124267243900175));
#47420=CARTESIAN_POINT('Ctrl Pts',(-0.0113190928250837,-0.0358967567230716,
-0.0122748226392094));
#47421=CARTESIAN_POINT('Ctrl Pts',(-0.0113329888046075,-0.0359185770962935,
-0.0119670924101008));
#47422=CARTESIAN_POINT('Ctrl Pts',(-0.0113709445238759,-0.035929414185463,
-0.0118142581804075));
#47423=CARTESIAN_POINT('Ctrl Pts',(-0.0115013278036741,-0.0359489564107254,
-0.0115386564115406));
#47424=CARTESIAN_POINT('Ctrl Pts',(-0.0115900090416198,-0.0359581184087839,
-0.0114173686868488));
#47425=CARTESIAN_POINT('Ctrl Pts',(-0.011811665809368,-0.0359790489329139,
-0.0112109278922474));
#47426=CARTESIAN_POINT('Ctrl Pts',(-0.011943827653377,-0.0359900634554343,
-0.0111291658169776));
#47427=CARTESIAN_POINT('Ctrl Pts',(-0.0122199143932926,-0.0360106814687695,
-0.0110258151076541));
#47428=CARTESIAN_POINT('Ctrl Pts',(-0.0123594608525394,-0.0360201442077475,
-0.0110006128129774));
#47429=CARTESIAN_POINT('Ctrl Pts',(-0.0125000000000001,-0.0360287743898721,
-0.0110006128129774));
#47430=CARTESIAN_POINT('Origin',(-0.0125,-0.0332787743898722,-0.0121758532865583));
#47431=CARTESIAN_POINT('',(-0.0125000000000002,-0.0365912743898722,-0.0110006128129774));
#47432=CARTESIAN_POINT('',(-0.0125,-0.0365287743898721,-0.0110006128129774));
#47433=CARTESIAN_POINT('',(-0.0125,-0.0332787743898722,-0.0110006128129775));
#47434=CARTESIAN_POINT('Ctrl Pts',(-0.0125000000000005,-0.0365912743898722,
-0.0110006128129774));
#47435=CARTESIAN_POINT('Ctrl Pts',(-0.0123910159324724,-0.0365845819318031,
-0.0110006128129773));
#47436=CARTESIAN_POINT('Ctrl Pts',(-0.0122823814488855,-0.036577373740337,
-0.0110157649684074));
#47437=CARTESIAN_POINT('Ctrl Pts',(-0.0120280106007402,-0.0365591770328985,
-0.0110884339050792));
#47438=CARTESIAN_POINT('Ctrl Pts',(-0.0118887595288113,-0.0365480830408749,
-0.0111601585760449));
#47439=CARTESIAN_POINT('Ctrl Pts',(-0.0116506050560141,-0.0365267283069574,
-0.0113499896715688));
#47440=CARTESIAN_POINT('Ctrl Pts',(-0.0115526507348646,-0.036516713373673,
-0.011464518064052));
#47441=CARTESIAN_POINT('Ctrl Pts',(-0.0114016238544625,-0.0364979109941513,
-0.0117296858730143));
#47442=CARTESIAN_POINT('Ctrl Pts',(-0.0113522108068163,-0.0364873147643931,
-0.0118791232899648));
#47443=CARTESIAN_POINT('Ctrl Pts',(-0.0113148510144864,-0.0364655594486451,
-0.0121859360209553));
#47444=CARTESIAN_POINT('Ctrl Pts',(-0.0113262625624588,-0.0364546173849002,
-0.0123402506950854));
#47445=CARTESIAN_POINT('Ctrl Pts',(-0.011406624700875,-0.036433935792472,
-0.0126319208288421));
#47446=CARTESIAN_POINT('Ctrl Pts',(-0.0114732936437026,-0.0364250339442455,
-0.0127668984933356));
#47447=CARTESIAN_POINT('Ctrl Pts',(-0.0116585957038017,-0.0364049886306321,
-0.0130113394432357));
#47448=CARTESIAN_POINT('Ctrl Pts',(-0.0117779956413319,-0.0363939305998197,
-0.0131164329738666));
#47449=CARTESIAN_POINT('Ctrl Pts',(-0.0120458313213491,-0.0363720275650022,
-0.013270319960279));
#47450=CARTESIAN_POINT('Ctrl Pts',(-0.012190524267742,-0.0363613918846556,
-0.0133196919938076));
#47451=CARTESIAN_POINT('Ctrl Pts',(-0.0124913697293818,-0.0363414577344296,
-0.0133608704526666));
#47452=CARTESIAN_POINT('Ctrl Pts',(-0.0126446562435927,-0.0363324250092816,
-0.013352042118004));
#47453=CARTESIAN_POINT('Ctrl Pts',(-0.0129427148659104,-0.0363114108653244,
-0.0132755746555834));
#47454=CARTESIAN_POINT('Ctrl Pts',(-0.0130842049671664,-0.0363003051179879,
-0.0132073965295047));
#47455=CARTESIAN_POINT('Ctrl Pts',(-0.0133277502173527,-0.0362788280763752,
-0.0130234527514248));
#47456=CARTESIAN_POINT('Ctrl Pts',(-0.0134288980729769,-0.0362686378228613,
-0.0129112220156681));
#47457=CARTESIAN_POINT('Ctrl Pts',(-0.0135867608199831,-0.0362496677210636,
-0.0126495819600103));
#47458=CARTESIAN_POINT('Ctrl Pts',(-0.0136399664581206,-0.036239359446599,
-0.0125014192025588));
#47459=CARTESIAN_POINT('Ctrl Pts',(-0.0136850836135262,-0.0362176404152308,
-0.0121951181860278));
#47460=CARTESIAN_POINT('Ctrl Pts',(-0.0136774522781934,-0.0362066548093585,
-0.0120401894422534));
#47461=CARTESIAN_POINT('Ctrl Pts',(-0.0136041153929361,-0.0361858308806997,
-0.0117465119569074));
#47462=CARTESIAN_POINT('Ctrl Pts',(-0.0135408491767724,-0.0361768006977145,
-0.0116101446405585));
#47463=CARTESIAN_POINT('Ctrl Pts',(-0.0133626568531267,-0.036157082734181,
-0.0113626224274056));
#47464=CARTESIAN_POINT('Ctrl Pts',(-0.013247245286305,-0.036146196223676,
-0.0112554586986463));
#47465=CARTESIAN_POINT('Ctrl Pts',(-0.0129848554626663,-0.0361243794529055,
-0.0110945723562825));
#47466=CARTESIAN_POINT('Ctrl Pts',(-0.0128412022424354,-0.0361136593901614,
-0.011041019393603));
#47467=CARTESIAN_POINT('Ctrl Pts',(-0.012627932464109,-0.0360993154528448,
-0.0110058316689456));
#47468=CARTESIAN_POINT('Ctrl Pts',(-0.0125639527294939,-0.0360952015782241,
-0.0110006128129774));
#47469=CARTESIAN_POINT('Ctrl Pts',(-0.0125,-0.0360912743898722,-0.0110006128129774));
#47470=CARTESIAN_POINT('Ctrl Pts',(-0.0125000000000001,-0.0360287743898721,
-0.0110006128129774));
#47471=CARTESIAN_POINT('Ctrl Pts',(-0.0125159710528335,-0.0360297551350749,
-0.0110006128129774));
#47472=CARTESIAN_POINT('Ctrl Pts',(-0.0125319535331271,-0.0360307481242455,
-0.0110009383705918));
#47473=CARTESIAN_POINT('Ctrl Pts',(-0.0126978941423195,-0.0360411783251345,
-0.0110077126660084));
#47474=CARTESIAN_POINT('Ctrl Pts',(-0.0128452591868545,-0.0360514610293382,
-0.011042500525408));
#47475=CARTESIAN_POINT('Ctrl Pts',(-0.013124220810136,-0.0360730396778832,
-0.0111679672477668));
#47476=CARTESIAN_POINT('Ctrl Pts',(-0.0132522584585505,-0.036084149314727,
-0.011259555412206));
#47477=CARTESIAN_POINT('Ctrl Pts',(-0.0134620710591082,-0.0361049940698633,
-0.0114840917255256));
#47478=CARTESIAN_POINT('Ctrl Pts',(-0.0135430702704042,-0.0361139072157517,
-0.0116136110874333));
#47479=CARTESIAN_POINT('Ctrl Pts',(-0.0136516603585244,-0.036133981516931,
-0.011896716662131));
#47480=CARTESIAN_POINT('Ctrl Pts',(-0.0136780436136455,-0.0361446833036546,
-0.0120476427368969));
#47481=CARTESIAN_POINT('Ctrl Pts',(-0.0136718829591347,-0.036166497058621,
-0.0123552796295048));
#47482=CARTESIAN_POINT('Ctrl Pts',(-0.0136377657036639,-0.0361773996416091,
-0.0125090375110348));
#47483=CARTESIAN_POINT('Ctrl Pts',(-0.0135142640645741,-0.0361971773939341,
-0.0127879608911405));
#47484=CARTESIAN_POINT('Ctrl Pts',(-0.0134285562951811,-0.0362061692572171,
-0.0129115166694147));
#47485=CARTESIAN_POINT('Ctrl Pts',(-0.0132122586389499,-0.0362269563897444,
-0.0131231952466817));
#47486=CARTESIAN_POINT('Ctrl Pts',(-0.0130825270295917,-0.0362379312655106,
-0.0132080483445592));
#47487=CARTESIAN_POINT('Ctrl Pts',(-0.0127955530036067,-0.0362596633872245,
-0.0133239660074586));
#47488=CARTESIAN_POINT('Ctrl Pts',(-0.0126408357058475,-0.036270059136913,
-0.0133529795944559));
#47489=CARTESIAN_POINT('Ctrl Pts',(-0.0123354049479832,-0.0362889526234046,
-0.0133490958249835));
#47490=CARTESIAN_POINT('Ctrl Pts',(-0.0121875277880686,-0.0362991137265824,
-0.0133186248261753));
#47491=CARTESIAN_POINT('Ctrl Pts',(-0.0119058402015021,-0.0363205576805671,
-0.0132016787746938));
#47492=CARTESIAN_POINT('Ctrl Pts',(-0.0117755311350052,-0.0363316611044815,
-0.0131142000622447));
#47493=CARTESIAN_POINT('Ctrl Pts',(-0.0115586245092616,-0.0363527261250893,
-0.0128957382034486));
#47494=CARTESIAN_POINT('Ctrl Pts',(-0.0114733255896075,-0.0363618036710384,
-0.0127677615363021));
#47495=CARTESIAN_POINT('Ctrl Pts',(-0.011356692714163,-0.0363816947711399,
-0.0124872396254632));
#47496=CARTESIAN_POINT('Ctrl Pts',(-0.01132613730169,-0.036392309467934,
-0.0123375417700171));
#47497=CARTESIAN_POINT('Ctrl Pts',(-0.0113234200773491,-0.0364141970386679,
-0.0120288638620781));
#47498=CARTESIAN_POINT('Ctrl Pts',(-0.0113536446109233,-0.0364252621359081,
-0.011872814060629));
#47499=CARTESIAN_POINT('Ctrl Pts',(-0.0114706989202091,-0.0364453642075344,
-0.011589316842492));
#47500=CARTESIAN_POINT('Ctrl Pts',(-0.0115534420207808,-0.0364542391830359,
-0.0114634493033982));
#47501=CARTESIAN_POINT('Ctrl Pts',(-0.0117643758445707,-0.0364748802581914,
-0.0112465999566501));
#47502=CARTESIAN_POINT('Ctrl Pts',(-0.0118916190719469,-0.0364858089497747,
-0.0111587395152585));
#47503=CARTESIAN_POINT('Ctrl Pts',(-0.0121750606586413,-0.0365075756620527,
-0.011035727834487));
#47504=CARTESIAN_POINT('Ctrl Pts',(-0.0123289643669752,-0.0365181968274219,
-0.0110027187147509));
#47505=CARTESIAN_POINT('Ctrl Pts',(-0.0124899082346748,-0.0365281535261902,
-0.0110006453017553));
#47506=CARTESIAN_POINT('Ctrl Pts',(-0.0124949547290055,-0.0365284645715166,
-0.0110006128129774));
#47507=CARTESIAN_POINT('Ctrl Pts',(-0.0125,-0.0365287743898721,-0.0110006128129774));
#47508=CARTESIAN_POINT('Origin',(-0.0125,-0.0332787743898722,-0.0121758532865583));
#47509=CARTESIAN_POINT('',(-0.0125000000000002,-0.0370912743898722,-0.0110006128129773));
#47510=CARTESIAN_POINT('',(-0.0124999999999998,-0.0370287743898721,-0.0110006128129773));
#47511=CARTESIAN_POINT('',(-0.0125,-0.0332787743898722,-0.0110006128129775));
#47512=CARTESIAN_POINT('Ctrl Pts',(-0.0125000000000003,-0.0370912743898722,
-0.0110006128129773));
#47513=CARTESIAN_POINT('Ctrl Pts',(-0.0123685975923388,-0.0370832052736848,
-0.0110006128129773));
#47514=CARTESIAN_POINT('Ctrl Pts',(-0.0122379669078175,-0.0370744025225916,
-0.0110226422150859));
#47515=CARTESIAN_POINT('Ctrl Pts',(-0.0119678246142031,-0.0370544785569455,
-0.0111167128569917));
#47516=CARTESIAN_POINT('Ctrl Pts',(-0.011833539781003,-0.0370434342199873,
-0.0111956387463349));
#47517=CARTESIAN_POINT('Ctrl Pts',(-0.0116070898289398,-0.037022377685569,
-0.0113973317195526));
#47518=CARTESIAN_POINT('Ctrl Pts',(-0.0115157356944448,-0.0370130187127627,
-0.0115166234445081));
#47519=CARTESIAN_POINT('Ctrl Pts',(-0.0113792725155753,-0.0369936892534286,
-0.0117892245998102));
#47520=CARTESIAN_POINT('Ctrl Pts',(-0.0113379302073818,-0.0369829161845667,
-0.0119411559584241));
#47521=CARTESIAN_POINT('Ctrl Pts',(-0.0113171581777985,-0.0369611016134194,
-0.0122488043615369));
#47522=CARTESIAN_POINT('Ctrl Pts',(-0.011336586286407,-0.0369502744617805,
-0.0124014984433715));
#47523=CARTESIAN_POINT('Ctrl Pts',(-0.0114319609518788,-0.036929909022047,
-0.0126887099118166));
#47524=CARTESIAN_POINT('Ctrl Pts',(-0.0115061132334518,-0.0369211086252034,
-0.0128207699478459));
#47525=CARTESIAN_POINT('Ctrl Pts',(-0.0117043682898292,-0.0369006338935512,
-0.0130548877171049));
#47526=CARTESIAN_POINT('Ctrl Pts',(-0.0118284795125062,-0.0368895347393193,
-0.0131529809802588));
#47527=CARTESIAN_POINT('Ctrl Pts',(-0.0121025144857545,-0.0368677762466659,
-0.0132920535525929));
#47528=CARTESIAN_POINT('Ctrl Pts',(-0.0122487898210647,-0.0368573142119794,
-0.0133337869983317));
#47529=CARTESIAN_POINT('Ctrl Pts',(-0.0125527314161703,-0.036837720222863,
-0.0133600082902373));
#47530=CARTESIAN_POINT('Ctrl Pts',(-0.0127075865527121,-0.0368282354164281,
-0.0133428699125894));
#47531=CARTESIAN_POINT('Ctrl Pts',(-0.0130022365098488,-0.0368068340239882,
-0.0132495758267264));
#47532=CARTESIAN_POINT('Ctrl Pts',(-0.0131390542732378,-0.0367957606001123,
-0.0131742166822104));
#47533=CARTESIAN_POINT('Ctrl Pts',(-0.0133713796489952,-0.0367745526274465,
-0.0129784288087641));
#47534=CARTESIAN_POINT('Ctrl Pts',(-0.0134660322655738,-0.0367648951321246,
-0.0128615460563626));
#47535=CARTESIAN_POINT('Ctrl Pts',(-0.0136098548297126,-0.0367458289813388,
-0.0125926583114163));
#47536=CARTESIAN_POINT('Ctrl Pts',(-0.0136552848518729,-0.0367351411395208,
-0.01244192890006));
#47537=CARTESIAN_POINT('Ctrl Pts',(-0.0136844222710554,-0.0367133484465393,
-0.0121345890422173));
#47538=CARTESIAN_POINT('Ctrl Pts',(-0.013669020831319,-0.0367024596930923,
-0.0119810261971247));
#47539=CARTESIAN_POINT('Ctrl Pts',(-0.0135812101027114,-0.0366819329301478,
-0.011691539605877));
#47540=CARTESIAN_POINT('Ctrl Pts',(-0.0135108662789414,-0.0366731114162018,
-0.0115580175121104));
#47541=CARTESIAN_POINT('Ctrl Pts',(-0.0133191621693466,-0.0366528519710482,
-0.0113186254919463));
#47542=CARTESIAN_POINT('Ctrl Pts',(-0.0131973946833203,-0.0366417698145867,
-0.0112169521930585));
#47543=CARTESIAN_POINT('Ctrl Pts',(-0.012926408855032,-0.0366199307819255,
-0.0110703266536913));
#47544=CARTESIAN_POINT('Ctrl Pts',(-0.0127808874148052,-0.0366093773287217,
-0.0110247088935657));
#47545=CARTESIAN_POINT('Ctrl Pts',(-0.012587214336645,-0.0365967159688182,
-0.0110030370823802));
#47546=CARTESIAN_POINT('Ctrl Pts',(-0.0125435845119462,-0.0365939508133649,
-0.0110006128129774));
#47547=CARTESIAN_POINT('Ctrl Pts',(-0.0125000000000005,-0.0365912743898722,
-0.0110006128129774));
#47548=CARTESIAN_POINT('Ctrl Pts',(-0.0125,-0.0365287743898721,-0.0110006128129774));
#47549=CARTESIAN_POINT('Ctrl Pts',(-0.012644057324453,-0.0365376206150619,
-0.0110006128129774));
#47550=CARTESIAN_POINT('Ctrl Pts',(-0.0127870035996141,-0.0365473376160089,
-0.0110270981087197));
#47551=CARTESIAN_POINT('Ctrl Pts',(-0.0130663655501122,-0.0365682998844921,
-0.0111344859689061));
#47552=CARTESIAN_POINT('Ctrl Pts',(-0.0131986298923942,-0.0365793892413662,
-0.0112181812726274));
#47553=CARTESIAN_POINT('Ctrl Pts',(-0.0134219398439058,-0.0366006481927421,
-0.0114310222127636));
#47554=CARTESIAN_POINT('Ctrl Pts',(-0.0135111919474361,-0.0366099362468724,
-0.0115576089672795));
#47555=CARTESIAN_POINT('Ctrl Pts',(-0.013635047801415,-0.0366296588464219,
-0.0118357545340962));
#47556=CARTESIAN_POINT('Ctrl Pts',(-0.0136693042393584,-0.0366401885685552,
-0.0119842540016153));
#47557=CARTESIAN_POINT('Ctrl Pts',(-0.0136799717532264,-0.0366620075578438,
-0.0122919647132708));
#47558=CARTESIAN_POINT('Ctrl Pts',(-0.0136539438670768,-0.0366730950308132,
-0.0124483300770714));
#47559=CARTESIAN_POINT('Ctrl Pts',(-0.0135445649441898,-0.036693412455111,
-0.0127348643893149));
#47560=CARTESIAN_POINT('Ctrl Pts',(-0.0134649510895904,-0.0367022222555921,
-0.0128632260770478));
#47561=CARTESIAN_POINT('Ctrl Pts',(-0.013259691741225,-0.0367227061503151,
-0.0130854705081921));
#47562=CARTESIAN_POINT('Ctrl Pts',(-0.0131351373811488,-0.0367335791151055,
-0.0131764163871841));
#47563=CARTESIAN_POINT('Ctrl Pts',(-0.0128554348450942,-0.0367553792705709,
-0.0133068475845299));
#47564=CARTESIAN_POINT('Ctrl Pts',(-0.012702441844019,-0.0367660907526982,
-0.0133439815493386));
#47565=CARTESIAN_POINT('Ctrl Pts',(-0.0123977835902895,-0.0367852279905299,
-0.0133560785297924));
#47566=CARTESIAN_POINT('Ctrl Pts',(-0.0122491209316249,-0.0367947990505451,
-0.0133336411379627));
#47567=CARTESIAN_POINT('Ctrl Pts',(-0.0119628073437893,-0.0368159666251517,
-0.0132325030492665));
#47568=CARTESIAN_POINT('Ctrl Pts',(-0.0118286330905472,-0.0368270330427736,
-0.0131527628276649));
#47569=CARTESIAN_POINT('Ctrl Pts',(-0.0115987499446077,-0.0368484859204106,
-0.012945837154466));
#47570=CARTESIAN_POINT('Ctrl Pts',(-0.0115053631408727,-0.0368580511205173,
-0.012820683327321));
#47571=CARTESIAN_POINT('Ctrl Pts',(-0.0113741223718986,-0.0368775975153528,
-0.0125450227554419));
#47572=CARTESIAN_POINT('Ctrl Pts',(-0.0113361318600384,-0.0368880339276796,
-0.0123978392254569));
#47573=CARTESIAN_POINT('Ctrl Pts',(-0.0113174022638658,-0.0369097683479152,
-0.0120913211814888));
#47574=CARTESIAN_POINT('Ctrl Pts',(-0.0113391542897758,-0.0369208706975362,
-0.0119347460139715));
#47575=CARTESIAN_POINT('Ctrl Pts',(-0.0114406711066737,-0.0369414021390191,
-0.0116451934418326));
#47576=CARTESIAN_POINT('Ctrl Pts',(-0.0115171160639166,-0.0369502073678009,
-0.0115142513591822));
#47577=CARTESIAN_POINT('Ctrl Pts',(-0.0117166261953091,-0.0369705293043836,
-0.0112866171464137));
#47578=CARTESIAN_POINT('Ctrl Pts',(-0.0118384023485465,-0.0369813388560223,
-0.0111926478888798));
#47579=CARTESIAN_POINT('Ctrl Pts',(-0.0121141467720003,-0.037003156502872,
-0.0110548676814199));
#47580=CARTESIAN_POINT('Ctrl Pts',(-0.0122661085524211,-0.0370139508462579,
-0.0110136104243289));
#47581=CARTESIAN_POINT('Ctrl Pts',(-0.0124478103935037,-0.0370255387636812,
-0.0110014810954639));
#47582=CARTESIAN_POINT('Ctrl Pts',(-0.012473917137073,-0.0370271727019334,
-0.0110006128129773));
#47583=CARTESIAN_POINT('Ctrl Pts',(-0.0124999999999997,-0.0370287743898721,
-0.0110006128129773));
#47584=CARTESIAN_POINT('Origin',(-0.0125,-0.0332787743898722,-0.0121758532865583));
#47585=CARTESIAN_POINT('',(-0.0125,-0.0375912743898721,-0.0110006128129773));
#47586=CARTESIAN_POINT('',(-0.0124999999999998,-0.037528774389872,-0.0110006128129773));
#47587=CARTESIAN_POINT('',(-0.0125,-0.0332787743898722,-0.0110006128129775));
#47588=CARTESIAN_POINT('Ctrl Pts',(-0.0125,-0.0375912743898721,-0.0110006128129773));
#47589=CARTESIAN_POINT('Ctrl Pts',(-0.0124966408622287,-0.0375910681130356,
-0.0110006128129773));
#47590=CARTESIAN_POINT('Ctrl Pts',(-0.0124932811404291,-0.0375908612897337,
-0.0110006272148874));
#47591=CARTESIAN_POINT('Ctrl Pts',(-0.0123403235283202,-0.0375814220089463,
-0.0110019390550596));
#47592=CARTESIAN_POINT('Ctrl Pts',(-0.0121923815235324,-0.0375712794821269,
-0.0110317737787349));
#47593=CARTESIAN_POINT('Ctrl Pts',(-0.0119103137976082,-0.0375498568575994,
-0.0111474597957408));
#47594=CARTESIAN_POINT('Ctrl Pts',(-0.0117796808171522,-0.037538755169121,
-0.0112343285234444));
#47595=CARTESIAN_POINT('Ctrl Pts',(-0.0115617337990316,-0.0375176583154644,
-0.0114518862454815));
#47596=CARTESIAN_POINT('Ctrl Pts',(-0.0114757973806388,-0.0375085505706955,
-0.0115796371412965));
#47597=CARTESIAN_POINT('Ctrl Pts',(-0.0113579887363392,-0.0374886866424524,
-0.011859775850523));
#47598=CARTESIAN_POINT('Ctrl Pts',(-0.011326827768129,-0.0374780853466678,
-0.0120092847130642));
#47599=CARTESIAN_POINT('Ctrl Pts',(-0.0113228124329801,-0.0374562079777241,
-0.0123178187463206));
#47600=CARTESIAN_POINT('Ctrl Pts',(-0.0113523530815602,-0.0374451387087904,
-0.0124739273806864));
#47601=CARTESIAN_POINT('Ctrl Pts',(-0.0114681589190712,-0.0374250011824154,
-0.012757924613091));
#47602=CARTESIAN_POINT('Ctrl Pts',(-0.0115503903526256,-0.037416140972307,
-0.0128841962096427));
#47603=CARTESIAN_POINT('Ctrl Pts',(-0.0117603969781781,-0.0373955253953266,
-0.0131019323151485));
#47604=CARTESIAN_POINT('Ctrl Pts',(-0.0118872046835685,-0.0373846053327843,
-0.0131903037139901));
#47605=CARTESIAN_POINT('Ctrl Pts',(-0.0121700470964044,-0.0373628320434691,
-0.0133145387047329));
#47606=CARTESIAN_POINT('Ctrl Pts',(-0.012323809423536,-0.0373521955392449,
-0.0133482253481312));
#47607=CARTESIAN_POINT('Ctrl Pts',(-0.0126288105206927,-0.0373332793246859,
-0.0133534943744511));
#47608=CARTESIAN_POINT('Ctrl Pts',(-0.0127771338405923,-0.0373234256615799,
-0.0133276665041483));
#47609=CARTESIAN_POINT('Ctrl Pts',(-0.013060582622869,-0.0373022087885629,
-0.0132201759269938));
#47610=CARTESIAN_POINT('Ctrl Pts',(-0.0131923450799375,-0.0372912003904165,
-0.0131378948349357));
#47611=CARTESIAN_POINT('Ctrl Pts',(-0.013413112214115,-0.0372702934898366,
-0.0129305794702442));
#47612=CARTESIAN_POINT('Ctrl Pts',(-0.0135012988579798,-0.0372611634086988,
-0.0128089179874886));
#47613=CARTESIAN_POINT('Ctrl Pts',(-0.0136305459609977,-0.0372415819072085,
-0.0125327623104696));
#47614=CARTESIAN_POINT('Ctrl Pts',(-0.0136678681958573,-0.0372307334953414,
-0.0123797683980664));
#47615=CARTESIAN_POINT('Ctrl Pts',(-0.0136804833451595,-0.0372089132558917,
-0.0120720400555337));
#47616=CARTESIAN_POINT('Ctrl Pts',(-0.0136571603139226,-0.037198153304402,
-0.0119202936897192));
#47617=CARTESIAN_POINT('Ctrl Pts',(-0.0135544116682296,-0.0371779488572334,
-0.011635352681013));
#47618=CARTESIAN_POINT('Ctrl Pts',(-0.0134764704145116,-0.0371691093436274,
-0.0115047113528514));
#47619=CARTESIAN_POINT('Ctrl Pts',(-0.0132717829635454,-0.0371484270651985,
-0.0112758808009031));
#47620=CARTESIAN_POINT('Ctrl Pts',(-0.0131454526554889,-0.0371373189630884,
-0.0111813787245666));
#47621=CARTESIAN_POINT('Ctrl Pts',(-0.0128686027709003,-0.0371156545638149,
-0.0110498356980546));
#47622=CARTESIAN_POINT('Ctrl Pts',(-0.0127216824450164,-0.0371052894822773,
-0.0110119540471123));
#47623=CARTESIAN_POINT('Ctrl Pts',(-0.0125477199530562,-0.0370942304977055,
-0.0110013387314271));
#47624=CARTESIAN_POINT('Ctrl Pts',(-0.0125238488275897,-0.0370927388908975,
-0.0110006128129773));
#47625=CARTESIAN_POINT('Ctrl Pts',(-0.0125000000000003,-0.0370912743898722,
-0.0110006128129773));
#47626=CARTESIAN_POINT('Ctrl Pts',(-0.0124999999999997,-0.0370287743898721,
-0.0110006128129773));
#47627=CARTESIAN_POINT('Ctrl Pts',(-0.0126224476628745,-0.0370362936160126,
-0.0110006128129773));
#47628=CARTESIAN_POINT('Ctrl Pts',(-0.0127442864279888,-0.037044453621814,
-0.0110197411394502));
#47629=CARTESIAN_POINT('Ctrl Pts',(-0.0130078504536451,-0.0370636559755463,
-0.0111048520550244));
#47630=CARTESIAN_POINT('Ctrl Pts',(-0.0131438051915405,-0.0370746912530215,
-0.0111806300548851));
#47631=CARTESIAN_POINT('Ctrl Pts',(-0.013380158569642,-0.0370963295804707,
-0.0113815797122461));
#47632=CARTESIAN_POINT('Ctrl Pts',(-0.0134776962594941,-0.0371062277278314,
-0.0115053081471911));
#47633=CARTESIAN_POINT('Ctrl Pts',(-0.0136161835651565,-0.0371255972993,
-0.0117784749993407));
#47634=CARTESIAN_POINT('Ctrl Pts',(-0.0136577846176067,-0.0371359360257146,
-0.0119242808760732));
#47635=CARTESIAN_POINT('Ctrl Pts',(-0.0136843498331268,-0.0371575735251978,
-0.0122294320577491));
#47636=CARTESIAN_POINT('Ctrl Pts',(-0.0136667734166237,-0.0371686826771268,
-0.0123861031574389));
#47637=CARTESIAN_POINT('Ctrl Pts',(-0.0135729847832567,-0.0371894182276145,
-0.0126785342555404));
#47638=CARTESIAN_POINT('Ctrl Pts',(-0.0134996307059135,-0.037198277582668,
-0.0128120303918967));
#47639=CARTESIAN_POINT('Ctrl Pts',(-0.0133057084576302,-0.037218439798747,
-0.0130448380621064));
#47640=CARTESIAN_POINT('Ctrl Pts',(-0.0131866808977871,-0.0372291812321277,
-0.0131416466950343));
#47641=CARTESIAN_POINT('Ctrl Pts',(-0.0129149399853398,-0.0372510004198648,
-0.0132864046488839));
#47642=CARTESIAN_POINT('Ctrl Pts',(-0.0127640820083308,-0.0372618670604148,
-0.0133316129468484));
#47643=CARTESIAN_POINT('Ctrl Pts',(-0.0124604504641844,-0.0372815129854695,
-0.0133598361559728));
#47644=CARTESIAN_POINT('Ctrl Pts',(-0.0123108671398517,-0.0372905937650852,
-0.0133453068884122));
#47645=CARTESIAN_POINT('Ctrl Pts',(-0.012019245236608,-0.0373115470184224,
-0.0132594081683051));
#47646=CARTESIAN_POINT('Ctrl Pts',(-0.0118806865943221,-0.0373226359432046,
-0.0131866270995324));
#47647=CARTESIAN_POINT('Ctrl Pts',(-0.0116442109327482,-0.0373439487779304,
-0.012995070016698));
#47648=CARTESIAN_POINT('Ctrl Pts',(-0.0115472108189611,-0.037353854567675,
-0.0128798668323187));
#47649=CARTESIAN_POINT('Ctrl Pts',(-0.0113982492115195,-0.0373727331647398,
-0.0126136241360601));
#47650=CARTESIAN_POINT('Ctrl Pts',(-0.0113499757176555,-0.0373833564818653,
-0.0124638047090652));
#47651=CARTESIAN_POINT('Ctrl Pts',(-0.0113149756787381,-0.0374051241371581,
-0.0121568179548843));
#47652=CARTESIAN_POINT('Ctrl Pts',(-0.011327535565838,-0.0374160516372124,
-0.0120027086708183));
#47653=CARTESIAN_POINT('Ctrl Pts',(-0.0114100374733141,-0.0374366891624931,
-0.011711660011005));
#47654=CARTESIAN_POINT('Ctrl Pts',(-0.011477754783642,-0.037445561983475,
-0.0115771022701026));
#47655=CARTESIAN_POINT('Ctrl Pts',(-0.0116648908044211,-0.0374656690033175,
-0.011334097361487));
#47656=CARTESIAN_POINT('Ctrl Pts',(-0.0117849765197717,-0.0374767346940491,
-0.0112299755789547));
#47657=CARTESIAN_POINT('Ctrl Pts',(-0.0120537314192286,-0.0374986208661648,
-0.011078156352826));
#47658=CARTESIAN_POINT('Ctrl Pts',(-0.0121986708078293,-0.0375092337062857,
-0.0110298553959062));
#47659=CARTESIAN_POINT('Ctrl Pts',(-0.0123990475439641,-0.0375224599652766,
-0.0110038612464219));
#47660=CARTESIAN_POINT('Ctrl Pts',(-0.0124495468686633,-0.0375256761804403,
-0.0110006128129773));
#47661=CARTESIAN_POINT('Ctrl Pts',(-0.0124999999999997,-0.037528774389872,
-0.0110006128129773));
#47662=CARTESIAN_POINT('Origin',(-0.0125,-0.0332787743898722,-0.0121758532865583));
#47663=CARTESIAN_POINT('',(-0.0124999999999998,-0.0380912743898721,-0.0110006128129773));
#47664=CARTESIAN_POINT('',(-0.0125,-0.0380287743898721,-0.0110006128129773));
#47665=CARTESIAN_POINT('',(-0.0125,-0.0332787743898722,-0.0110006128129775));
#47666=CARTESIAN_POINT('Ctrl Pts',(-0.0124999999999997,-0.0380912743898721,
-0.0110006128129773));
#47667=CARTESIAN_POINT('Ctrl Pts',(-0.0124762424888991,-0.0380898154963799,
-0.0110006128129773));
#47668=CARTESIAN_POINT('Ctrl Pts',(-0.0124524628126795,-0.0380883297019628,
-0.0110013331832036));
#47669=CARTESIAN_POINT('Ctrl Pts',(-0.0122785928628455,-0.0380772780454556,
-0.011011902092839));
#47670=CARTESIAN_POINT('Ctrl Pts',(-0.0121316670101472,-0.0380669138956383,
-0.0110497478911719));
#47671=CARTESIAN_POINT('Ctrl Pts',(-0.0118547918942762,-0.0380452504383218,
-0.0111812206471982));
#47672=CARTESIAN_POINT('Ctrl Pts',(-0.0117284414188247,-0.0380341422896691,
-0.0112756891053517));
#47673=CARTESIAN_POINT('Ctrl Pts',(-0.0115236943642097,-0.0380134581061522,
-0.0115044701552302));
#47674=CARTESIAN_POINT('Ctrl Pts',(-0.0114457177685337,-0.0380046179541512,
-0.0116350983828561));
#47675=CARTESIAN_POINT('Ctrl Pts',(-0.0113429010274434,-0.0379844150100093,
-0.0119200181945472));
#47676=CARTESIAN_POINT('Ctrl Pts',(-0.0113195421890426,-0.0379736557115737,
-0.0120717553504145));
#47677=CARTESIAN_POINT('Ctrl Pts',(-0.0113320820491274,-0.0379518354918623,
-0.0123794834145812));
#47678=CARTESIAN_POINT('Ctrl Pts',(-0.0113693670208866,-0.0379409864203264,
-0.0125324866302184));
#47679=CARTESIAN_POINT('Ctrl Pts',(-0.0114985472991291,-0.0379214026135655,
-0.0128086748182053));
#47680=CARTESIAN_POINT('Ctrl Pts',(-0.0115867048996421,-0.0379122743621264,
-0.0129303582918763));
#47681=CARTESIAN_POINT('Ctrl Pts',(-0.0118074197690923,-0.0378913688516608,
-0.013137724972483));
#47682=CARTESIAN_POINT('Ctrl Pts',(-0.0119391587116199,-0.0378803608189864,
-0.0132200364834926));
#47683=CARTESIAN_POINT('Ctrl Pts',(-0.0122299052169146,-0.037858594732115,
-0.0133303780340251));
#47684=CARTESIAN_POINT('Ctrl Pts',(-0.0123864346840221,-0.0378484250732582,
-0.013356083403582));
#47685=CARTESIAN_POINT('Ctrl Pts',(-0.0126932523815696,-0.0378291827723794,
-0.0133447633052546));
#47686=CARTESIAN_POINT('Ctrl Pts',(-0.0128406964987416,-0.0378189165812173,
-0.0133105781667553));
#47687=CARTESIAN_POINT('Ctrl Pts',(-0.0131200541284824,-0.0377973556880612,
-0.0131862981521401));
#47688=CARTESIAN_POINT('Ctrl Pts',(-0.013248416655367,-0.0377862463352569,
-0.0130952807052713));
#47689=CARTESIAN_POINT('Ctrl Pts',(-0.0134592235887506,-0.0377653703768205,
-0.0128715865137773));
#47690=CARTESIAN_POINT('Ctrl Pts',(-0.0135408206552691,-0.0377564385561343,
-0.0127422839319029));
#47691=CARTESIAN_POINT('Ctrl Pts',(-0.0136505409160875,-0.037736389717793,
-0.0124595374567003));
#47692=CARTESIAN_POINT('Ctrl Pts',(-0.0136775134542161,-0.0377256996822031,
-0.0123087771068284));
#47693=CARTESIAN_POINT('Ctrl Pts',(-0.0136726003590957,-0.0377038882999825,
-0.0120011736767842));
#47694=CARTESIAN_POINT('Ctrl Pts',(-0.013639105015219,-0.0376929758033051,
-0.0118472759836266));
#47695=CARTESIAN_POINT('Ctrl Pts',(-0.0135167180201757,-0.0376731604377815,
-0.0115678221488813));
#47696=CARTESIAN_POINT('Ctrl Pts',(-0.0134314870394243,-0.0376641909579558,
-0.0114438979822576));
#47697=CARTESIAN_POINT('Ctrl Pts',(-0.0132160508428487,-0.0376434271143786,
-0.0112313841959012));
#47698=CARTESIAN_POINT('Ctrl Pts',(-0.0130867152099326,-0.0376324592223532,
-0.0111460422285071));
#47699=CARTESIAN_POINT('Ctrl Pts',(-0.0128033956951292,-0.0376109556656038,
-0.0110302416176938));
#47700=CARTESIAN_POINT('Ctrl Pts',(-0.0126523623669168,-0.0376006306084005,
-0.0110006128129773));
#47701=CARTESIAN_POINT('Ctrl Pts',(-0.0125,-0.0375912743898721,-0.0110006128129773));
#47702=CARTESIAN_POINT('Ctrl Pts',(-0.0124999999999997,-0.037528774389872,
-0.0110006128129773));
#47703=CARTESIAN_POINT('Ctrl Pts',(-0.0126013419560833,-0.0375349975636544,
-0.0110006128129773));
#47704=CARTESIAN_POINT('Ctrl Pts',(-0.012702440074249,-0.0375416702731698,
-0.0110137146547475));
#47705=CARTESIAN_POINT('Ctrl Pts',(-0.0129510701067612,-0.0375592721463527,
-0.0110795492167575));
#47706=CARTESIAN_POINT('Ctrl Pts',(-0.0130919325839813,-0.0375703753413148,
-0.0111487424278653));
#47707=CARTESIAN_POINT('Ctrl Pts',(-0.0133339294243193,-0.0375918163492662,
-0.0113343517732612));
#47708=CARTESIAN_POINT('Ctrl Pts',(-0.0134341845631314,-0.0376019748769485,
-0.0114472338883389));
#47709=CARTESIAN_POINT('Ctrl Pts',(-0.0135901067471434,-0.0376208616106867,
-0.0117098836372724));
#47710=CARTESIAN_POINT('Ctrl Pts',(-0.0136422534676913,-0.0376312651783639,
-0.0118584084498437));
#47711=CARTESIAN_POINT('Ctrl Pts',(-0.0136851759337633,-0.0376529984057797,
-0.0121649096716104));
#47712=CARTESIAN_POINT('Ctrl Pts',(-0.0136764702810102,-0.0376639723199725,
-0.0123196735289665));
#47713=CARTESIAN_POINT('Ctrl Pts',(-0.013601139433123,-0.0376847562163576,
-0.0126127864437316));
#47714=CARTESIAN_POINT('Ctrl Pts',(-0.013536913370896,-0.0376937448829899,
-0.0127487575711001));
#47715=CARTESIAN_POINT('Ctrl Pts',(-0.0133569680278647,-0.0377135278724449,
-0.0129950775718869));
#47716=CARTESIAN_POINT('Ctrl Pts',(-0.0132408082311493,-0.0377244318449745,
-0.013101437858328));
#47717=CARTESIAN_POINT('Ctrl Pts',(-0.0129773842082659,-0.0377462452916852,
-0.0132604391573848));
#47718=CARTESIAN_POINT('Ctrl Pts',(-0.012833465607223,-0.0377569454540161,
-0.0133129711605081));
#47719=CARTESIAN_POINT('Ctrl Pts',(-0.0125339585442544,-0.0377770162200712,
-0.0133603211487119));
#47720=CARTESIAN_POINT('Ctrl Pts',(-0.0123812764837934,-0.0377859318764176,
-0.0133548464932053));
#47721=CARTESIAN_POINT('Ctrl Pts',(-0.0120819481442601,-0.0378067809750571,
-0.0132852334760115));
#47722=CARTESIAN_POINT('Ctrl Pts',(-0.0119386576122462,-0.0378178905837921,
-0.0132200648737588));
#47723=CARTESIAN_POINT('Ctrl Pts',(-0.01169063449608,-0.0378394667862012,
-0.0130410800803158));
#47724=CARTESIAN_POINT('Ctrl Pts',(-0.0115868917499629,-0.0378497472054623,
-0.012930800632283));
#47725=CARTESIAN_POINT('Ctrl Pts',(-0.0114228833421882,-0.0378690142336669,
-0.0126714301349768));
#47726=CARTESIAN_POINT('Ctrl Pts',(-0.0113664177539262,-0.0378791291329928,
-0.0125234225269568));
#47727=CARTESIAN_POINT('Ctrl Pts',(-0.0113154314733675,-0.0379008707744343,
-0.0122168026431469));
#47728=CARTESIAN_POINT('Ctrl Pts',(-0.0113202540238054,-0.0379118844087942,
-0.0120614786168155));
#47729=CARTESIAN_POINT('Ctrl Pts',(-0.0113883853282242,-0.0379328114671998,
-0.011766346704439));
#47730=CARTESIAN_POINT('Ctrl Pts',(-0.0114491667925139,-0.0379419686853233,
-0.0116289381630961));
#47731=CARTESIAN_POINT('Ctrl Pts',(-0.0116228071807605,-0.0379615166845352,
-0.0113783257413523));
#47732=CARTESIAN_POINT('Ctrl Pts',(-0.0117362545785923,-0.0379723554481044,
-0.0112691067112621));
#47733=CARTESIAN_POINT('Ctrl Pts',(-0.0119959028700665,-0.0379941758255843,
-0.0111033701658758));
#47734=CARTESIAN_POINT('Ctrl Pts',(-0.0121388355308802,-0.0380049451881162,
-0.011047178619133));
#47735=CARTESIAN_POINT('Ctrl Pts',(-0.0123584576527009,-0.0380198560395445,
-0.0110070032263349));
#47736=CARTESIAN_POINT('Ctrl Pts',(-0.0124292306108147,-0.0380244286063054,
-0.0110006128129773));
#47737=CARTESIAN_POINT('Ctrl Pts',(-0.0125,-0.0380287743898721,-0.0110006128129773));
#47738=CARTESIAN_POINT('Origin',(-0.0125,-0.0332787743898722,-0.0121758532865583));
#47739=CARTESIAN_POINT('',(-0.0124999999999998,-0.0385912743898722,-0.0110006128129773));
#47740=CARTESIAN_POINT('',(-0.0125000000000001,-0.0385287743898722,-0.0110006128129773));
#47741=CARTESIAN_POINT('',(-0.0125,-0.0332787743898722,-0.0110006128129775));
#47742=CARTESIAN_POINT('Ctrl Pts',(-0.0124999999999995,-0.0385912743898722,
-0.0110006128129773));
#47743=CARTESIAN_POINT('Ctrl Pts',(-0.0124565087484192,-0.0385886036932816,
-0.0110006128129773));
#47744=CARTESIAN_POINT('Ctrl Pts',(-0.0124129722332789,-0.038585844635133,
-0.0110030267200982));
#47745=CARTESIAN_POINT('Ctrl Pts',(-0.0122193907855129,-0.0385731909235403,
-0.0110246415132767));
#47746=CARTESIAN_POINT('Ctrl Pts',(-0.0120738617796335,-0.0385626382988648,
-0.0110702228000275));
#47747=CARTESIAN_POINT('Ctrl Pts',(-0.0118028463302189,-0.0385407999549928,
-0.0112167776062675));
#47748=CARTESIAN_POINT('Ctrl Pts',(-0.0116810563382989,-0.0385297176014095,
-0.0113184174837754));
#47749=CARTESIAN_POINT('Ctrl Pts',(-0.0114892903831182,-0.038509456105351,
-0.0115577602315995));
#47750=CARTESIAN_POINT('Ctrl Pts',(-0.011418910843281,-0.0385006350800992,
-0.0116912684002995));
#47751=CARTESIAN_POINT('Ctrl Pts',(-0.0113310284402633,-0.0384801098264777,
-0.0119807337057369));
#47752=CARTESIAN_POINT('Ctrl Pts',(-0.011315588716793,-0.0384692216215687,
-0.012134288814862));
#47753=CARTESIAN_POINT('Ctrl Pts',(-0.0113446469210865,-0.0384474286450853,
-0.0124416326708999));
#47754=CARTESIAN_POINT('Ctrl Pts',(-0.0113900384024102,-0.0384367399584771,
-0.0125923739962358));
#47755=CARTESIAN_POINT('Ctrl Pts',(-0.0115337914369434,-0.0384176712908055,
-0.012861297236537));
#47756=CARTESIAN_POINT('Ctrl Pts',(-0.0116284125486714,-0.0384080169285458,
-0.0129782027228725));
#47757=CARTESIAN_POINT('Ctrl Pts',(-0.0118606820391104,-0.0383868103800675,
-0.013174047222225));
#47758=CARTESIAN_POINT('Ctrl Pts',(-0.0119974760830762,-0.0383757371936117,
-0.0132494407533667));
#47759=CARTESIAN_POINT('Ctrl Pts',(-0.012292108301633,-0.0383543339708812,
-0.0133428171881113));
#47760=CARTESIAN_POINT('Ctrl Pts',(-0.0124469713593605,-0.0383448463927707,
-0.013359996557367));
#47761=CARTESIAN_POINT('Ctrl Pts',(-0.0127509274661702,-0.0383252540851647,
-0.0133338478287654));
#47762=CARTESIAN_POINT('Ctrl Pts',(-0.0128972094706624,-0.0383147929505996,
-0.0132921513230074));
#47763=CARTESIAN_POINT('Ctrl Pts',(-0.0131712724234851,-0.0382930352932722,
-0.0131531507737321));
#47764=CARTESIAN_POINT('Ctrl Pts',(-0.013295405422814,-0.0382819360159618,
-0.0130550917573229));
#47765=CARTESIAN_POINT('Ctrl Pts',(-0.0134937224473557,-0.0382614592670485,
-0.0128210244216694));
#47766=CARTESIAN_POINT('Ctrl Pts',(-0.0135679110095299,-0.0382526587741834,
-0.0126889780991429));
#47767=CARTESIAN_POINT('Ctrl Pts',(-0.0136633569632183,-0.0382322948744837,
-0.0124017883496194));
#47768=CARTESIAN_POINT('Ctrl Pts',(-0.0136828228830148,-0.0382214683389497,
-0.0122491029566404));
#47769=CARTESIAN_POINT('Ctrl Pts',(-0.013662129729114,-0.0381996536389373,
-0.0119414527361572));
#47770=CARTESIAN_POINT('Ctrl Pts',(-0.0136208261326266,-0.038188879804804,
-0.0117895105850076));
#47771=CARTESIAN_POINT('Ctrl Pts',(-0.013484432524159,-0.0381695478863152,
-0.0115168747485271));
#47772=CARTESIAN_POINT('Ctrl Pts',(-0.0133931092330342,-0.0381601914192525,
-0.0113975602185732));
#47773=CARTESIAN_POINT('Ctrl Pts',(-0.0131667144387111,-0.0381391363225177,
-0.0111958122603209));
#47774=CARTESIAN_POINT('Ctrl Pts',(-0.0130324537532802,-0.0381280922978589,
-0.0111168533544608));
#47775=CARTESIAN_POINT('Ctrl Pts',(-0.0127622413096364,-0.0381081602964126,
-0.0110226775600301));
#47776=CARTESIAN_POINT('Ctrl Pts',(-0.0126315077083065,-0.0380993499723272,
-0.0110006128129773));
#47777=CARTESIAN_POINT('Ctrl Pts',(-0.0124999999999997,-0.0380912743898721,
-0.0110006128129773));
#47778=CARTESIAN_POINT('Ctrl Pts',(-0.0125,-0.0380287743898721,-0.0110006128129773));
#47779=CARTESIAN_POINT('Ctrl Pts',(-0.0125792245739267,-0.0380336393866655,
-0.0110006128129773));
#47780=CARTESIAN_POINT('Ctrl Pts',(-0.0126584094591171,-0.0380387858650269,
-0.0110086209606377));
#47781=CARTESIAN_POINT('Ctrl Pts',(-0.0128894712097824,-0.0380546568427985,
-0.0110560634391791));
#47782=CARTESIAN_POINT('Ctrl Pts',(-0.0130347525988559,-0.0380657641942526,
-0.0111177201075049));
#47783=CARTESIAN_POINT('Ctrl Pts',(-0.0132877951446664,-0.0380874421122772,
-0.0112908799611763));
#47784=CARTESIAN_POINT('Ctrl Pts',(-0.0133944713437147,-0.0380978206403427,
-0.0113988457541976));
#47785=CARTESIAN_POINT('Ctrl Pts',(-0.0135641167653714,-0.0381172614344754,
-0.0116533538590951));
#47786=CARTESIAN_POINT('Ctrl Pts',(-0.0136238323153567,-0.0381270191111541,
-0.0117985266493816));
#47787=CARTESIAN_POINT('Ctrl Pts',(-0.0136830674183474,-0.0381485838480861,
-0.0121026516691176));
#47788=CARTESIAN_POINT('Ctrl Pts',(-0.0136824472934211,-0.038159632625784,
-0.012258471317927));
#47789=CARTESIAN_POINT('Ctrl Pts',(-0.0136220906017364,-0.0381807099432772,
-0.012555722317037));
#47790=CARTESIAN_POINT('Ctrl Pts',(-0.0135649670083539,-0.0381901058174151,
-0.0126947052449274));
#47791=CARTESIAN_POINT('Ctrl Pts',(-0.0133980574140238,-0.0382093996438471,
-0.0129498066043904));
#47792=CARTESIAN_POINT('Ctrl Pts',(-0.013287568282305,-0.0382201615589701,
-0.0130619819319864));
#47793=CARTESIAN_POINT('Ctrl Pts',(-0.0130321183860904,-0.0382419741035772,
-0.0132347693790506));
#47794=CARTESIAN_POINT('Ctrl Pts',(-0.0128903331222531,-0.0382528100966197,
-0.0132948276405998));
#47795=CARTESIAN_POINT('Ctrl Pts',(-0.0125941574734224,-0.038273197780509,
-0.0133568867193244));
#47796=CARTESIAN_POINT('Ctrl Pts',(-0.012442804108133,-0.0382819974089869,
-0.0133592522105797));
#47797=CARTESIAN_POINT('Ctrl Pts',(-0.0121407420705348,-0.0383024429238496,
-0.0133057574890605));
#47798=CARTESIAN_POINT('Ctrl Pts',(-0.0119934648327149,-0.038313540218447,
-0.0132478413935696));
#47799=CARTESIAN_POINT('Ctrl Pts',(-0.0117353091325814,-0.0383353106378249,
-0.0130809287109513));
#47800=CARTESIAN_POINT('Ctrl Pts',(-0.0116256156192813,-0.0383457856167584,
-0.0129754685883863));
#47801=CARTESIAN_POINT('Ctrl Pts',(-0.0114501336999095,-0.0383654038662279,
-0.0127260643294132));
#47802=CARTESIAN_POINT('Ctrl Pts',(-0.0113870932397963,-0.0383748492484878,
-0.0125837812488675));
#47803=CARTESIAN_POINT('Ctrl Pts',(-0.01131940612733,-0.0383962241418599,
-0.0122823335711542));
#47804=CARTESIAN_POINT('Ctrl Pts',(-0.0113156586839864,-0.0384073009082556,
-0.0121261192009379));
#47805=CARTESIAN_POINT('Ctrl Pts',(-0.0113679411761218,-0.0384285294031837,
-0.0118267361637458));
#47806=CARTESIAN_POINT('Ctrl Pts',(-0.011421326884658,-0.0384382327481969,
-0.0116860930166371));
#47807=CARTESIAN_POINT('Ctrl Pts',(-0.0115813338519879,-0.0384572625424429,
-0.0114264831879714));
#47808=CARTESIAN_POINT('Ctrl Pts',(-0.0116887267330117,-0.0384679381180455,
-0.0113113802696304));
#47809=CARTESIAN_POINT('Ctrl Pts',(-0.0119396988863677,-0.038489726559083,
-0.0111315170042053));
#47810=CARTESIAN_POINT('Ctrl Pts',(-0.0120802083836475,-0.0385006231509987,
-0.0110675398121957));
#47811=CARTESIAN_POINT('Ctrl Pts',(-0.0123180275050788,-0.0385172248734522,
-0.0110111902257223));
#47812=CARTESIAN_POINT('Ctrl Pts',(-0.0124089449706238,-0.0385231829123296,
-0.0110006128129773));
#47813=CARTESIAN_POINT('Ctrl Pts',(-0.0125000000000001,-0.0385287743898722,
-0.0110006128129773));
#47814=CARTESIAN_POINT('Origin',(-0.0125,-0.0332787743898722,-0.0121758532865583));
#47815=CARTESIAN_POINT('',(-0.0125,-0.0390912743898723,-0.0110006128129773));
#47816=CARTESIAN_POINT('',(-0.0125000000000002,-0.0390287743898722,-0.0110006128129773));
#47817=CARTESIAN_POINT('',(-0.0125,-0.0332787743898722,-0.0110006128129775));
#47818=CARTESIAN_POINT('Ctrl Pts',(-0.0124999999999999,-0.0390912743898723,
-0.0110006128129773));
#47819=CARTESIAN_POINT('Ctrl Pts',(-0.0124361318042558,-0.0390873523925412,
-0.0110006128129773));
#47820=CARTESIAN_POINT('Ctrl Pts',(-0.0123722363768311,-0.0390832441837451,
-0.0110058178843355));
#47821=CARTESIAN_POINT('Ctrl Pts',(-0.01215904607225,-0.0390689072685523,
-0.0110409451971411));
#47822=CARTESIAN_POINT('Ctrl Pts',(-0.0120153842146561,-0.0390581878376882,
-0.0110944653768048));
#47823=CARTESIAN_POINT('Ctrl Pts',(-0.0117529609530406,-0.0390363711569898,
-0.0112552912623418));
#47824=CARTESIAN_POINT('Ctrl Pts',(-0.0116375252587077,-0.0390254840770212,
-0.0113624292631865));
#47825=CARTESIAN_POINT('Ctrl Pts',(-0.0114592765757163,-0.0390057640191463,
-0.0116099129316036));
#47826=CARTESIAN_POINT('Ctrl Pts',(-0.0113959795277,-0.0389967352350057,
-0.0117462674698344));
#47827=CARTESIAN_POINT('Ctrl Pts',(-0.0113225784449348,-0.0389759125906752,
-0.0120399268424449));
#47828=CARTESIAN_POINT('Ctrl Pts',(-0.0113149125058534,-0.0389649273529849,
-0.0121948503937928));
#47829=CARTESIAN_POINT('Ctrl Pts',(-0.0113599590372235,-0.0389432078485187,
-0.0125011580823699));
#47830=CARTESIAN_POINT('Ctrl Pts',(-0.0114131306293705,-0.0389328965650288,
-0.0126493326067472));
#47831=CARTESIAN_POINT('Ctrl Pts',(-0.0115709310215612,-0.0389139291321524,
-0.0129110053851285));
#47832=CARTESIAN_POINT('Ctrl Pts',(-0.0116720502096819,-0.0389037398919044,
-0.0130232571945109));
#47833=CARTESIAN_POINT('Ctrl Pts',(-0.0119155457982235,-0.0388822639923835,
-0.0132072547755021));
#47834=CARTESIAN_POINT('Ctrl Pts',(-0.01205701580927,-0.0388711583174186,
-0.0132754656575466));
#47835=CARTESIAN_POINT('Ctrl Pts',(-0.0123550601297221,-0.0388501423856107,
-0.0133520083192323));
#47836=CARTESIAN_POINT('Ctrl Pts',(-0.012508353399461,-0.0388411081565501,
-0.0133608735333428));
#47837=CARTESIAN_POINT('Ctrl Pts',(-0.0128092132906521,-0.0388211755114125,
-0.0133197625193752));
#47838=CARTESIAN_POINT('Ctrl Pts',(-0.0129539143058282,-0.0388105405594625,
-0.0132704250063773));
#47839=CARTESIAN_POINT('Ctrl Pts',(-0.0132217798683727,-0.0387886380506598,
-0.0131166046146733));
#47840=CARTESIAN_POINT('Ctrl Pts',(-0.0133412020375297,-0.0387775797632527,
-0.0130115423529003));
#47841=CARTESIAN_POINT('Ctrl Pts',(-0.0135265633021201,-0.0387575324531254,
-0.0127671476349733));
#47842=CARTESIAN_POINT('Ctrl Pts',(-0.0135932660368702,-0.0387486316172506,
-0.0126321835652931));
#47843=CARTESIAN_POINT('Ctrl Pts',(-0.0136736973294375,-0.0387279514438123,
-0.0123405334433879));
#47844=CARTESIAN_POINT('Ctrl Pts',(-0.0136851460146902,-0.038717009841257,
-0.0121862252733616));
#47845=CARTESIAN_POINT('Ctrl Pts',(-0.0136478624518023,-0.0386952541065763,
-0.0118794066342107));
#47846=CARTESIAN_POINT('Ctrl Pts',(-0.0135984861716224,-0.0386846569917755,
-0.0117299567356054));
#47847=CARTESIAN_POINT('Ctrl Pts',(-0.0134475259835041,-0.0386658521435036,
-0.0114647541101418));
#47848=CARTESIAN_POINT('Ctrl Pts',(-0.0133496025749925,-0.0386558408190745,
-0.0113502039268433));
#47849=CARTESIAN_POINT('Ctrl Pts',(-0.0131115024117913,-0.0386344874358246,
-0.0111603168609624));
#47850=CARTESIAN_POINT('Ctrl Pts',(-0.0129722736321817,-0.0386233935968088,
-0.01108855789427));
#47851=CARTESIAN_POINT('Ctrl Pts',(-0.012717825645211,-0.0386051887856272,
-0.0110157939936399));
#47852=CARTESIAN_POINT('Ctrl Pts',(-0.0126090884023289,-0.0385979732548987,
-0.0110006128129773));
#47853=CARTESIAN_POINT('Ctrl Pts',(-0.0124999999999995,-0.0385912743898722,
-0.0110006128129773));
#47854=CARTESIAN_POINT('Ctrl Pts',(-0.0125000000000001,-0.0385287743898722,
-0.0110006128129773));
#47855=CARTESIAN_POINT('Ctrl Pts',(-0.0125578492220588,-0.0385323267760305,
-0.0110006128129773));
#47856=CARTESIAN_POINT('Ctrl Pts',(-0.0126157352120663,-0.038536032821848,
-0.0110048832182397));
#47857=CARTESIAN_POINT('Ctrl Pts',(-0.0128286273097136,-0.0385502306554375,
-0.0110366041367009));
#47858=CARTESIAN_POINT('Ctrl Pts',(-0.0129778167006288,-0.0385613098926756,
-0.0110906989641319));
#47859=CARTESIAN_POINT('Ctrl Pts',(-0.0132409588145226,-0.0385831587061255,
-0.0112511860900441));
#47860=CARTESIAN_POINT('Ctrl Pts',(-0.0133536257320299,-0.0385937240327688,
-0.0113540444522945));
#47861=CARTESIAN_POINT('Ctrl Pts',(-0.0135349091409325,-0.0386135161787347,
-0.0115983051214637));
#47862=CARTESIAN_POINT('Ctrl Pts',(-0.0136012206378563,-0.0386227106913121,
-0.0117377654968751));
#47863=CARTESIAN_POINT('Ctrl Pts',(-0.013677218490762,-0.0386438906044774,
-0.0120364633910202));
#47864=CARTESIAN_POINT('Ctrl Pts',(-0.0136853168434272,-0.038654986717369,
-0.0121929506026564));
#47865=CARTESIAN_POINT('Ctrl Pts',(-0.0136410847413676,-0.0386763608530617,
-0.0124943875949039));
#47866=CARTESIAN_POINT('Ctrl Pts',(-0.0135913713404146,-0.0386864282979431,
-0.0126367116161759));
#47867=CARTESIAN_POINT('Ctrl Pts',(-0.0134381563641025,-0.0387051951268156,
-0.012900668377162));
#47868=CARTESIAN_POINT('Ctrl Pts',(-0.0133338668335931,-0.0387157785554355,
-0.0130185473795422));
#47869=CARTESIAN_POINT('Ctrl Pts',(-0.0130874626240551,-0.0387375276967032,
-0.0132052140754249));
#47870=CARTESIAN_POINT('Ctrl Pts',(-0.012948303434786,-0.0387484763239597,
-0.0132729977664375));
#47871=CARTESIAN_POINT('Ctrl Pts',(-0.0126557771581247,-0.0387691782884885,
-0.0133502422710352));
#47872=CARTESIAN_POINT('Ctrl Pts',(-0.0125056218009486,-0.0387780952443826,
-0.01336051233767));
#47873=CARTESIAN_POINT('Ctrl Pts',(-0.0122011294815262,-0.0387981118242208,
-0.0133233254309806));
#47874=CARTESIAN_POINT('Ctrl Pts',(-0.0120501873479036,-0.0388091660979174,
-0.0132729705589158));
#47875=CARTESIAN_POINT('Ctrl Pts',(-0.0117823869548519,-0.0388310765594811,
-0.0131188129765792));
#47876=CARTESIAN_POINT('Ctrl Pts',(-0.0116669120554339,-0.03884172264508,
-0.0130185403130255));
#47877=CARTESIAN_POINT('Ctrl Pts',(-0.0114800927087565,-0.0388616783828028,
-0.0127792539376614));
#47878=CARTESIAN_POINT('Ctrl Pts',(-0.0114106851287761,-0.0388706900440563,
-0.0126424380334966));
#47879=CARTESIAN_POINT('Ctrl Pts',(-0.0113268416643965,-0.0388916784719636,
-0.012346440634055));
#47880=CARTESIAN_POINT('Ctrl Pts',(-0.0113145891210247,-0.0389027851863762,
-0.0121898039103801));
#47881=CARTESIAN_POINT('Ctrl Pts',(-0.0113510906883082,-0.0389242784911866,
-0.0118866862896884));
#47882=CARTESIAN_POINT('Ctrl Pts',(-0.0113972432896594,-0.0389344832308502,
-0.011742770012788));
#47883=CARTESIAN_POINT('Ctrl Pts',(-0.0115440435453904,-0.0389534915350077,
-0.0114746980722283));
#47884=CARTESIAN_POINT('Ctrl Pts',(-0.011645362238405,-0.0389637570449468,
-0.0113542011536127));
#47885=CARTESIAN_POINT('Ctrl Pts',(-0.0118874769316534,-0.0389854691664807,
-0.011161148967723));
#47886=CARTESIAN_POINT('Ctrl Pts',(-0.0120252802075833,-0.0389964599974716,
-0.0110898263770345));
#47887=CARTESIAN_POINT('Ctrl Pts',(-0.012279411085358,-0.0390146763854293,
-0.0110161866952631));
#47888=CARTESIAN_POINT('Ctrl Pts',(-0.0123895096540082,-0.0390219894347465,
-0.0110006128129772));
#47889=CARTESIAN_POINT('Ctrl Pts',(-0.0125000000000005,-0.0390287743898722,
-0.0110006128129773));
#47890=CARTESIAN_POINT('Origin',(-0.0125,-0.0332787743898722,-0.0121758532865583));
#47891=CARTESIAN_POINT('',(-0.0125,-0.0395912743898723,-0.0110006128129773));
#47892=CARTESIAN_POINT('',(-0.0125000000000001,-0.0395287743898722,-0.0110006128129773));
#47893=CARTESIAN_POINT('',(-0.0125,-0.0332787743898722,-0.0110006128129775));
#47894=CARTESIAN_POINT('Ctrl Pts',(-0.0125,-0.0395912743898723,-0.0110006128129773));
#47895=CARTESIAN_POINT('Ctrl Pts',(-0.0124163471756474,-0.0395861374645212,
-0.0110006128129773));
#47896=CARTESIAN_POINT('Ctrl Pts',(-0.0123327666728288,-0.0395806884477098,
-0.0110095408579271));
#47897=CARTESIAN_POINT('Ctrl Pts',(-0.0121014577168271,-0.0395647037939129,
-0.0110597614842461));
#47898=CARTESIAN_POINT('Ctrl Pts',(-0.0119600159999679,-0.0395538502287097,
-0.0111209104229628));
#47899=CARTESIAN_POINT('Ctrl Pts',(-0.0117057896218844,-0.039532042745072,
-0.0112956743170487));
#47900=CARTESIAN_POINT('Ctrl Pts',(-0.011596152235659,-0.0395213039987005,
-0.011408671418606));
#47901=CARTESIAN_POINT('Ctrl Pts',(-0.0114311551249103,-0.0395020829923444,
-0.0116650313503914));
#47902=CARTESIAN_POINT('Ctrl Pts',(-0.0113750682010705,-0.0394926082737645,
-0.0118044695324368));
#47903=CARTESIAN_POINT('Ctrl Pts',(-0.0113169380912085,-0.0394714887657494,
-0.012102315539655));
#47904=CARTESIAN_POINT('Ctrl Pts',(-0.0113175223621992,-0.0394604314056039,
-0.0122582562257425));
#47905=CARTESIAN_POINT('Ctrl Pts',(-0.011379099913938,-0.0394389184205922,
-0.0125616513940631));
#47906=CARTESIAN_POINT('Ctrl Pts',(-0.0114397371892158,-0.0394292528808071,
-0.0127060216173676));
#47907=CARTESIAN_POINT('Ctrl Pts',(-0.0116109939109865,-0.0394097628455809,
-0.0129591277516267));
#47908=CARTESIAN_POINT('Ctrl Pts',(-0.0117185053767981,-0.0393993571534504,
-0.0130664130035824));
#47909=CARTESIAN_POINT('Ctrl Pts',(-0.0119729685420149,-0.0393776523683252,
-0.0132378700795595));
#47910=CARTESIAN_POINT('Ctrl Pts',(-0.0121188078296144,-0.0393665469964113,
-0.0132985046048348));
#47911=CARTESIAN_POINT('Ctrl Pts',(-0.0124198941510669,-0.0393459493763168,
-0.0133579795616833));
#47912=CARTESIAN_POINT('Ctrl Pts',(-0.0125717273653552,-0.0393371329748319,
-0.0133585173954677));
#47913=CARTESIAN_POINT('Ctrl Pts',(-0.0128691685211884,-0.0393168622654799,
-0.0133019495962233));
#47914=CARTESIAN_POINT('Ctrl Pts',(-0.0130117976041611,-0.0393060739741659,
-0.0132446983363376));
#47915=CARTESIAN_POINT('Ctrl Pts',(-0.013270316772168,-0.0392842541838535,
-0.0130770226532524));
#47916=CARTESIAN_POINT('Ctrl Pts',(-0.0133829629088728,-0.0392734356645072,
-0.0129669868021019));
#47917=CARTESIAN_POINT('Ctrl Pts',(-0.0135547660310336,-0.0392539567134342,
-0.0127151396981697));
#47918=CARTESIAN_POINT('Ctrl Pts',(-0.0136145473299957,-0.0392447403605457,
-0.0125773056168207));
#47919=CARTESIAN_POINT('Ctrl Pts',(-0.0136805657768665,-0.0392237720176859,
-0.0122815914745074));
#47920=CARTESIAN_POINT('Ctrl Pts',(-0.0136842469397555,-0.0392127480366382,
-0.0121261215300212));
#47921=CARTESIAN_POINT('Ctrl Pts',(-0.0136310082319303,-0.0391910538696436,
-0.0118201711729089));
#47922=CARTESIAN_POINT('Ctrl Pts',(-0.0135736543662515,-0.0391810414770292,
-0.0116729388373926));
#47923=CARTESIAN_POINT('Ctrl Pts',(-0.0134081123580706,-0.039161726943374,
-0.0114148846860343));
#47924=CARTESIAN_POINT('Ctrl Pts',(-0.013303569966771,-0.0391514193698006,
-0.0113052243557608));
#47925=CARTESIAN_POINT('Ctrl Pts',(-0.0130541739979964,-0.0391298143253974,
-0.0111278039020919));
#47926=CARTESIAN_POINT('Ctrl Pts',(-0.0129103359923623,-0.0391187046208255,
-0.0110635808488112));
#47927=CARTESIAN_POINT('Ctrl Pts',(-0.0126732202193077,-0.0391022511041286,
-0.0110101932849007));
#47928=CARTESIAN_POINT('Ctrl Pts',(-0.0125866562353605,-0.0390965957477068,
-0.0110006128129773));
#47929=CARTESIAN_POINT('Ctrl Pts',(-0.0124999999999999,-0.0390912743898723,
-0.0110006128129773));
#47930=CARTESIAN_POINT('Ctrl Pts',(-0.0125000000000005,-0.0390287743898722,
-0.0110006128129773));
#47931=CARTESIAN_POINT('Ctrl Pts',(-0.0125380043212259,-0.0390311081468334,
-0.0110006128129773));
#47932=CARTESIAN_POINT('Ctrl Pts',(-0.0125760469588011,-0.0390335096083526,
-0.0110024561063973));
#47933=CARTESIAN_POINT('Ctrl Pts',(-0.0127692440411077,-0.039046040941093,
-0.0110212848501554));
#47934=CARTESIAN_POINT('Ctrl Pts',(-0.0129199019936708,-0.0390569192236894,
-0.0110671679735217));
#47935=CARTESIAN_POINT('Ctrl Pts',(-0.0131909381848969,-0.0390787371639758,
-0.011213111355022));
#47936=CARTESIAN_POINT('Ctrl Pts',(-0.0133094877011632,-0.0390894662334035,
-0.011310399248883));
#47937=CARTESIAN_POINT('Ctrl Pts',(-0.0135024469069445,-0.0391096006828934,
-0.0115440917795719));
#47938=CARTESIAN_POINT('Ctrl Pts',(-0.0135752671756624,-0.0391184752188413,
-0.0116780331128062));
#47939=CARTESIAN_POINT('Ctrl Pts',(-0.0136677153550896,-0.0391392455068082,
-0.0119709541096058));
#47940=CARTESIAN_POINT('Ctrl Pts',(-0.013684570737312,-0.0391503550589178,
-0.0121276308529956));
#47941=CARTESIAN_POINT('Ctrl Pts',(-0.0136566562467006,-0.0391719743851289,
-0.0124325257390941));
#47942=CARTESIAN_POINT('Ctrl Pts',(-0.0136144353474513,-0.0391822955854814,
-0.0125780844477775));
#47943=CARTESIAN_POINT('Ctrl Pts',(-0.0134746925329525,-0.0392016341206397,
-0.0128508135983907));
#47944=CARTESIAN_POINT('Ctrl Pts',(-0.0133764261076692,-0.0392115960900017,
-0.0129742925408032));
#47945=CARTESIAN_POINT('Ctrl Pts',(-0.0131389501348909,-0.0392332660162748,
-0.0131741890763487));
#47946=CARTESIAN_POINT('Ctrl Pts',(-0.0130026967627076,-0.03924429501537,
-0.013249272739898));
#47947=CARTESIAN_POINT('Ctrl Pts',(-0.012713873067471,-0.0392652841591031,
-0.0133410304146222));
#47948=CARTESIAN_POINT('Ctrl Pts',(-0.0125646798355172,-0.0392745321348618,
-0.0133587210736983));
#47949=CARTESIAN_POINT('Ctrl Pts',(-0.012260598453781,-0.0392939760734432,
-0.0133369741904191));
#47950=CARTESIAN_POINT('Ctrl Pts',(-0.0121088297574482,-0.0393047841449024,
-0.0132949952909828));
#47951=CARTESIAN_POINT('Ctrl Pts',(-0.0118338010400032,-0.0393266031935076,
-0.0131559359067574));
#47952=CARTESIAN_POINT('Ctrl Pts',(-0.0117125205384294,-0.0393374008447962,
-0.0130614438139135));
#47953=CARTESIAN_POINT('Ctrl Pts',(-0.0115140252998137,-0.039357693913761,
-0.0128328659887244));
#47954=CARTESIAN_POINT('Ctrl Pts',(-0.0114381400426169,-0.0393665047562633,
-0.0127014626687907));
#47955=CARTESIAN_POINT('Ctrl Pts',(-0.0113380201532362,-0.0393870735158575,
-0.0124113838035935));
#47956=CARTESIAN_POINT('Ctrl Pts',(-0.0113170249850932,-0.0393981776653904,
-0.0122547832521241));
#47957=CARTESIAN_POINT('Ctrl Pts',(-0.0113371775917443,-0.0394198955701545,
-0.0119484981239624));
#47958=CARTESIAN_POINT('Ctrl Pts',(-0.0113758251818902,-0.0394303147579032,
-0.0118015575102327));
#47959=CARTESIAN_POINT('Ctrl Pts',(-0.011508376598657,-0.0394498294613337,
-0.011526343878615));
#47960=CARTESIAN_POINT('Ctrl Pts',(-0.0116025072219682,-0.039459450404398,
-0.0114014462064592));
#47961=CARTESIAN_POINT('Ctrl Pts',(-0.0118335592970148,-0.0394809371956775,
-0.0111955886174164));
#47962=CARTESIAN_POINT('Ctrl Pts',(-0.0119680626276684,-0.0394919986210786,
-0.0111165591840503));
#47963=CARTESIAN_POINT('Ctrl Pts',(-0.0122382704608941,-0.0395119227656996,
-0.0110225970119605));
#47964=CARTESIAN_POINT('Ctrl Pts',(-0.0123687365131833,-0.0395207138044907,
-0.0110006128129772));
#47965=CARTESIAN_POINT('Ctrl Pts',(-0.0125000000000001,-0.0395287743898722,
-0.0110006128129773));
#47966=CARTESIAN_POINT('Origin',(-0.0125,-0.0332787743898722,-0.0121758532865583));
#47967=CARTESIAN_POINT('',(-0.0125000000000002,-0.0400912743898723,-0.0110006128129772));
#47968=CARTESIAN_POINT('',(-0.0125,-0.0400287743898722,-0.0110006128129772));
#47969=CARTESIAN_POINT('',(-0.0125,-0.0332787743898722,-0.0110006128129775));
#47970=CARTESIAN_POINT('Ctrl Pts',(-0.0125000000000004,-0.0400912743898723,
-0.0110006128129772));
#47971=CARTESIAN_POINT('Ctrl Pts',(-0.0123962317877206,-0.0400849022253409,
-0.0110006128129772));
#47972=CARTESIAN_POINT('Ctrl Pts',(-0.0122927535448283,-0.0400780608560291,
-0.0110143493374508));
#47973=CARTESIAN_POINT('Ctrl Pts',(-0.0120441313791396,-0.0400604016002137,
-0.0110818160466131));
#47974=CARTESIAN_POINT('Ctrl Pts',(-0.0119053500422646,-0.0400494402872072,
-0.0111506120085336));
#47975=CARTESIAN_POINT('Ctrl Pts',(-0.0116600759365155,-0.0400276935027585,
-0.0113391696256987));
#47976=CARTESIAN_POINT('Ctrl Pts',(-0.0115566592011941,-0.0400171877730503,
-0.0114578276638657));
#47977=CARTESIAN_POINT('Ctrl Pts',(-0.0114052665283221,-0.0399983879548473,
-0.0117229593508435));
#47978=CARTESIAN_POINT('Ctrl Pts',(-0.0113565975937592,-0.0399882626657875,
-0.0118657551449614));
#47979=CARTESIAN_POINT('Ctrl Pts',(-0.0113145736351104,-0.039966859998235,
-0.0121675945187651));
#47980=CARTESIAN_POINT('Ctrl Pts',(-0.0113238530734446,-0.039955760091895,
-0.0123241352289692));
#47981=CARTESIAN_POINT('Ctrl Pts',(-0.0114020898978315,-0.0399346340959946,
-0.0126220727340926));
#47982=CARTESIAN_POINT('Ctrl Pts',(-0.0114692838554654,-0.0399254972306594,
-0.0127607762996261));
#47983=CARTESIAN_POINT('Ctrl Pts',(-0.0116521411573634,-0.0399056583403411,
-0.0130036293666762));
#47984=CARTESIAN_POINT('Ctrl Pts',(-0.0117656095383184,-0.0398950694984301,
-0.0131057628197797));
#47985=CARTESIAN_POINT('Ctrl Pts',(-0.0120300863970327,-0.0398732018276857,
-0.013264469984384));
#47986=CARTESIAN_POINT('Ctrl Pts',(-0.0121797814627849,-0.0398621289096384,
-0.0133175107196541));
#47987=CARTESIAN_POINT('Ctrl Pts',(-0.0124834558041281,-0.0398419589634149,
-0.0133604402231358));
#47988=CARTESIAN_POINT('Ctrl Pts',(-0.012634013305693,-0.0398331108801856,
-0.0133529535267219));
#47989=CARTESIAN_POINT('Ctrl Pts',(-0.0129278591315907,-0.0398125187473489,
-0.0132810924360404));
#47990=CARTESIAN_POINT('Ctrl Pts',(-0.0130679982489852,-0.0398016067620295,
-0.0132160395444263));
#47991=CARTESIAN_POINT('Ctrl Pts',(-0.0133177015541598,-0.0397798278255687,
-0.0130342466534));
#47992=CARTESIAN_POINT('Ctrl Pts',(-0.0134242270926281,-0.0397691774563157,
-0.0129183524182194));
#47993=CARTESIAN_POINT('Ctrl Pts',(-0.0135823238316769,-0.0397502213097931,
-0.0126575112679652));
#47994=CARTESIAN_POINT('Ctrl Pts',(-0.0136346764729176,-0.0397404217107833,
-0.0125164001929154));
#47995=CARTESIAN_POINT('Ctrl Pts',(-0.0136847056400201,-0.0397191519313817,
-0.0122164349255123));
#47996=CARTESIAN_POINT('Ctrl Pts',(-0.0136797396868606,-0.0397080688922195,
-0.0120601320911881));
#47997=CARTESIAN_POINT('Ctrl Pts',(-0.0136097146871464,-0.0396867480225824,
-0.0117594463040344));
#47998=CARTESIAN_POINT('Ctrl Pts',(-0.0135457545313975,-0.0396773789835379,
-0.0116179593148396));
#47999=CARTESIAN_POINT('Ctrl Pts',(-0.0133686469812788,-0.0396577117549183,
-0.0113699892362042));
#48000=CARTESIAN_POINT('Ctrl Pts',(-0.0132581174479979,-0.0396472108891491,
-0.0112652469845541));
#48001=CARTESIAN_POINT('Ctrl Pts',(-0.0129985543508686,-0.0396254171135893,
-0.0111001132059106));
#48002=CARTESIAN_POINT('Ctrl Pts',(-0.0128507338519276,-0.039614324056765,
-0.0110432575959414));
#48003=CARTESIAN_POINT('Ctrl Pts',(-0.0126311576369537,-0.0395995229692149,
-0.0110060986650045));
#48004=CARTESIAN_POINT('Ctrl Pts',(-0.0125655686602552,-0.0395953008087733,
-0.0110006128129773));
#48005=CARTESIAN_POINT('Ctrl Pts',(-0.0125,-0.0395912743898723,-0.0110006128129773));
#48006=CARTESIAN_POINT('Ctrl Pts',(-0.0125000000000001,-0.0395287743898722,
-0.0110006128129773));
#48007=CARTESIAN_POINT('Ctrl Pts',(-0.0125174245500157,-0.0395298443909558,
-0.0110006128129773));
#48008=CARTESIAN_POINT('Ctrl Pts',(-0.0125348614911154,-0.0395309288916245,
-0.0110010003229717));
#48009=CARTESIAN_POINT('Ctrl Pts',(-0.0127080845353512,-0.0395418396788189,
-0.0110087163783427));
#48010=CARTESIAN_POINT('Ctrl Pts',(-0.0128609013456591,-0.0395525665895324,
-0.0110465906896864));
#48011=CARTESIAN_POINT('Ctrl Pts',(-0.0131399095442775,-0.0395743710672021,
-0.0111783464258558));
#48012=CARTESIAN_POINT('Ctrl Pts',(-0.0132639717741701,-0.0395852332172042,
-0.0112698396598852));
#48013=CARTESIAN_POINT('Ctrl Pts',(-0.013468204796238,-0.0396056883974529,
-0.0114930518264234));
#48014=CARTESIAN_POINT('Ctrl Pts',(-0.0135472530135271,-0.0396144928452177,
-0.0116218701528459));
#48015=CARTESIAN_POINT('Ctrl Pts',(-0.0136552347883389,-0.0396348487923602,
-0.0119089477483654));
#48016=CARTESIAN_POINT('Ctrl Pts',(-0.0136805009641661,-0.0396459395008549,
-0.012065358742409));
#48017=CARTESIAN_POINT('Ctrl Pts',(-0.0136683944230493,-0.0396677445107659,
-0.0123728723045001));
#48018=CARTESIAN_POINT('Ctrl Pts',(-0.0136334700668644,-0.0396782581078943,
-0.0125211443629192));
#48019=CARTESIAN_POINT('Ctrl Pts',(-0.0135083008326579,-0.0396979496618003,
-0.0127988520965755));
#48020=CARTESIAN_POINT('Ctrl Pts',(-0.0134183203314263,-0.0397072824210437,
-0.0129251851045186));
#48021=CARTESIAN_POINT('Ctrl Pts',(-0.0131938431463073,-0.0397285761993604,
-0.0131369866574674));
#48022=CARTESIAN_POINT('Ctrl Pts',(-0.0130612323642198,-0.0397396621156901,
-0.0132199848666402));
#48023=CARTESIAN_POINT('Ctrl Pts',(-0.01277675232481,-0.0397609523237271,
-0.0133277577248656));
#48024=CARTESIAN_POINT('Ctrl Pts',(-0.0126284242873029,-0.0397708015612897,
-0.0133535361497418));
#48025=CARTESIAN_POINT('Ctrl Pts',(-0.0123234277900492,-0.03978972100852,
-0.0133481679761669));
#48026=CARTESIAN_POINT('Ctrl Pts',(-0.0121696760557943,-0.0398003586403142,
-0.013314431181386));
#48027=CARTESIAN_POINT('Ctrl Pts',(-0.0118868782278107,-0.0398221323996069,
-0.0131901057113366));
#48028=CARTESIAN_POINT('Ctrl Pts',(-0.0117601028558801,-0.0398330518152534,
-0.0131016965554965));
#48029=CARTESIAN_POINT('Ctrl Pts',(-0.0115501649361208,-0.0398536654999091,
-0.0128838948225458));
#48030=CARTESIAN_POINT('Ctrl Pts',(-0.0114679714101034,-0.0398625246798243,
-0.0127575932318192));
#48031=CARTESIAN_POINT('Ctrl Pts',(-0.0113522581725218,-0.0398826648293535,
-0.0124735590053716));
#48032=CARTESIAN_POINT('Ctrl Pts',(-0.011322768230276,-0.0398937343994475,
-0.012317446123776));
#48033=CARTESIAN_POINT('Ctrl Pts',(-0.0113268797739995,-0.0399156109968757,
-0.0120089229711124));
#48034=CARTESIAN_POINT('Ctrl Pts',(-0.0113580856030866,-0.0399262112921243,
-0.0118594282190164));
#48035=CARTESIAN_POINT('Ctrl Pts',(-0.0114759814413373,-0.0399460732013568,
-0.0115793179836641));
#48036=CARTESIAN_POINT('Ctrl Pts',(-0.0115619652282376,-0.0399551832485288,
-0.0114515838363079));
#48037=CARTESIAN_POINT('Ctrl Pts',(-0.0117799894325702,-0.0399762824589431,
-0.0112340933305413));
#48038=CARTESIAN_POINT('Ctrl Pts',(-0.0119106463487137,-0.0399873840102053,
-0.0111472699309539));
#48039=CARTESIAN_POINT('Ctrl Pts',(-0.0121927420742577,-0.0400088050361703,
-0.011031677499403));
#48040=CARTESIAN_POINT('Ctrl Pts',(-0.0123406887842786,-0.0400189461772311,
-0.0110018900118203));
#48041=CARTESIAN_POINT('Ctrl Pts',(-0.0124935218279313,-0.0400283761057175,
-0.0110006262016197));
#48042=CARTESIAN_POINT('Ctrl Pts',(-0.0124967611857696,-0.0400285755018244,
-0.0110006128129772));
#48043=CARTESIAN_POINT('Ctrl Pts',(-0.0125,-0.0400287743898722,-0.0110006128129772));
#48044=CARTESIAN_POINT('Origin',(-0.0125,-0.0332787743898722,-0.0121758532865583));
#48045=CARTESIAN_POINT('',(-0.0125000000000002,-0.0405912743898722,-0.0110006128129772));
#48046=CARTESIAN_POINT('',(-0.0124999999999998,-0.0405287743898722,-0.0110006128129772));
#48047=CARTESIAN_POINT('',(-0.0125,-0.0332787743898722,-0.0110006128129775));
#48048=CARTESIAN_POINT('Ctrl Pts',(-0.0125000000000003,-0.0405912743898722,
-0.0110006128129772));
#48049=CARTESIAN_POINT('Ctrl Pts',(-0.0123765027860332,-0.0405836907132406,
-0.0110006128129772));
#48050=CARTESIAN_POINT('Ctrl Pts',(-0.0122536356788734,-0.040575455876852,
-0.0110200706532127));
#48051=CARTESIAN_POINT('Ctrl Pts',(-0.0119892666271235,-0.0405561673436804,
-0.0111062179802573));
#48052=CARTESIAN_POINT('Ctrl Pts',(-0.0118534807529531,-0.0405451286580267,
-0.0111823845909718));
#48053=CARTESIAN_POINT('Ctrl Pts',(-0.0116177571092469,-0.0405235081326747,
-0.0113839228584159));
#48054=CARTESIAN_POINT('Ctrl Pts',(-0.0115206270855756,-0.0405136450041091,
-0.0115077909292436));
#48055=CARTESIAN_POINT('Ctrl Pts',(-0.0113828442745808,-0.0404942580696245,
-0.0117812026500237));
#48056=CARTESIAN_POINT('Ctrl Pts',(-0.0113415917858301,-0.0404839095858865,
-0.0119271461331726));
#48057=CARTESIAN_POINT('Ctrl Pts',(-0.0113157847889707,-0.0404622620663835,
-0.012232438626044));
#48058=CARTESIAN_POINT('Ctrl Pts',(-0.0113337661272027,-0.0404511532393016,
-0.0123891051444517));
#48059=CARTESIAN_POINT('Ctrl Pts',(-0.0114283067168395,-0.0404304372640064,
-0.0126812601758514));
#48060=CARTESIAN_POINT('Ctrl Pts',(-0.0115019605442114,-0.0404215856810574,
-0.0128145068882508));
#48061=CARTESIAN_POINT('Ctrl Pts',(-0.0116964238155177,-0.0404014078979584,
-0.0130468165589063));
#48062=CARTESIAN_POINT('Ctrl Pts',(-0.011815719401609,-0.0403906595979343,
-0.0131433546357287));
#48063=CARTESIAN_POINT('Ctrl Pts',(-0.0120878543646401,-0.0403688399030079,
-0.0132874443796119));
#48064=CARTESIAN_POINT('Ctrl Pts',(-0.0122388234685241,-0.0403579799081463,
-0.0133322727534152));
#48065=CARTESIAN_POINT('Ctrl Pts',(-0.0125425107587682,-0.0403383576467293,
-0.0133597319563076));
#48066=CARTESIAN_POINT('Ctrl Pts',(-0.0126920466391854,-0.040329259200383,
-0.0133448306089765));
#48067=CARTESIAN_POINT('Ctrl Pts',(-0.0129822936812903,-0.0403083769367371,
-0.0132585528786485));
#48068=CARTESIAN_POINT('Ctrl Pts',(-0.0131196891079668,-0.0402973750998214,
-0.0131862134417303));
#48069=CARTESIAN_POINT('Ctrl Pts',(-0.0133615704310672,-0.0402755828940664,
-0.01299049820966));
#48070=CARTESIAN_POINT('Ctrl Pts',(-0.013462721956479,-0.0402653532113436,
-0.0128680062952246));
#48071=CARTESIAN_POINT('Ctrl Pts',(-0.0136073879773797,-0.0402461375367459,
-0.012597009833051));
#48072=CARTESIAN_POINT('Ctrl Pts',(-0.0136520225196291,-0.0402358867362545,
-0.0124524439655626));
#48073=CARTESIAN_POINT('Ctrl Pts',(-0.0136852026385219,-0.0402143425507755,
-0.0121486087806181));
#48074=CARTESIAN_POINT('Ctrl Pts',(-0.0136711668426919,-0.0402032336289454,
-0.0119919409259875));
#48075=CARTESIAN_POINT('Ctrl Pts',(-0.0135839794615331,-0.040182328971783,
-0.0116971249357849));
#48076=CARTESIAN_POINT('Ctrl Pts',(-0.0135132482466612,-0.0401733786547133,
-0.0115614294913511));
#48077=CARTESIAN_POINT('Ctrl Pts',(-0.0133240514652581,-0.0401533533738992,
-0.0113242994371902));
#48078=CARTESIAN_POINT('Ctrl Pts',(-0.0132073807317541,-0.0401426743145306,
-0.0112251679684209));
#48079=CARTESIAN_POINT('Ctrl Pts',(-0.0129391373269841,-0.040120865440619,
-0.0110746430629777));
#48080=CARTESIAN_POINT('Ctrl Pts',(-0.0127892876420601,-0.0401099439672909,
-0.0110261417510927));
#48081=CARTESIAN_POINT('Ctrl Pts',(-0.0125896441023155,-0.0400968700373949,
-0.0110031742278326));
#48082=CARTESIAN_POINT('Ctrl Pts',(-0.0125448006302718,-0.0400940254923624,
-0.0110006128129773));
#48083=CARTESIAN_POINT('Ctrl Pts',(-0.0125000000000004,-0.0400912743898723,
-0.0110006128129772));
#48084=CARTESIAN_POINT('Ctrl Pts',(-0.0125,-0.0400287743898722,-0.0110006128129772));
#48085=CARTESIAN_POINT('Ctrl Pts',(-0.0126524836274197,-0.0400381380547259,
-0.0110006128129772));
#48086=CARTESIAN_POINT('Ctrl Pts',(-0.0128036345865955,-0.0400484720113026,
-0.0110302888885797));
#48087=CARTESIAN_POINT('Ctrl Pts',(-0.0130870257612733,-0.0400699845916909,
-0.0111462198995466));
#48088=CARTESIAN_POINT('Ctrl Pts',(-0.0132163319242825,-0.0400809519582966,
-0.0112315980904499));
#48089=CARTESIAN_POINT('Ctrl Pts',(-0.0134317041325933,-0.040101714069395,
-0.0114441738418315));
#48090=CARTESIAN_POINT('Ctrl Pts',(-0.0135168997092491,-0.0401106819416352,
-0.0115681254152743));
#48091=CARTESIAN_POINT('Ctrl Pts',(-0.0136392038154371,-0.0401305000981957,
-0.0118476186116939));
#48092=CARTESIAN_POINT('Ctrl Pts',(-0.0136726529119307,-0.0401414133243714,
-0.0120015265928821));
#48093=CARTESIAN_POINT('Ctrl Pts',(-0.0136774732976494,-0.0401632245157759,
-0.0123091273318683));
#48094=CARTESIAN_POINT('Ctrl Pts',(-0.0136504569969394,-0.0401739136715251,
-0.0124598752734477));
#48095=CARTESIAN_POINT('Ctrl Pts',(-0.0135406527323881,-0.0401939606135981,
-0.0127425950057959));
#48096=CARTESIAN_POINT('Ctrl Pts',(-0.01345901114667,-0.0402028938799324,
-0.0128718814767081));
#48097=CARTESIAN_POINT('Ctrl Pts',(-0.0132481302720589,-0.0402237721545124,
-0.0130955129268549));
#48098=CARTESIAN_POINT('Ctrl Pts',(-0.0131197436700429,-0.0402348814785963,
-0.0131864878642911));
#48099=CARTESIAN_POINT('Ctrl Pts',(-0.0128403567717934,-0.0402564410368315,
-0.0133106795318864));
#48100=CARTESIAN_POINT('Ctrl Pts',(-0.0126929068688548,-0.0402667059931346,
-0.0133448198189927));
#48101=CARTESIAN_POINT('Ctrl Pts',(-0.0123860726132381,-0.0402859461530712,
-0.0133560508509775));
#48102=CARTESIAN_POINT('Ctrl Pts',(-0.0122295329013218,-0.0402961205978299,
-0.0133302933411034));
#48103=CARTESIAN_POINT('Ctrl Pts',(-0.0119388113577665,-0.0403178887926647,
-0.0132198490988367));
#48104=CARTESIAN_POINT('Ctrl Pts',(-0.0118071040076832,-0.0403288963334232,
-0.0131374967429749));
#48105=CARTESIAN_POINT('Ctrl Pts',(-0.0115864593381179,-0.0403497999763606,
-0.0129300611476745));
#48106=CARTESIAN_POINT('Ctrl Pts',(-0.0114983407452764,-0.0403589257781446,
-0.0128083481307916));
#48107=CARTESIAN_POINT('Ctrl Pts',(-0.0113692502369099,-0.0403785126808822,
-0.0125321162805999));
#48108=CARTESIAN_POINT('Ctrl Pts',(-0.0113320153237119,-0.0403893626374941,
-0.0123791005828364));
#48109=CARTESIAN_POINT('Ctrl Pts',(-0.0113195765966316,-0.0404111828286165,
-0.0120713729218565));
#48110=CARTESIAN_POINT('Ctrl Pts',(-0.0113429835292453,-0.0404219412488868,
-0.0119196481506558));
#48111=CARTESIAN_POINT('Ctrl Pts',(-0.0114458917413749,-0.0404421421735211,
-0.0116347568198472));
#48112=CARTESIAN_POINT('Ctrl Pts',(-0.0115239158223177,-0.040450983191197,
-0.0115041461888807));
#48113=CARTESIAN_POINT('Ctrl Pts',(-0.0117287429465967,-0.0404716699333819,
-0.011275431654526));
#48114=CARTESIAN_POINT('Ctrl Pts',(-0.0118551205028745,-0.0404827781435009,
-0.0111810083680333));
#48115=CARTESIAN_POINT('Ctrl Pts',(-0.0121320294889581,-0.040504440333381,
-0.0110496300259603));
#48116=CARTESIAN_POINT('Ctrl Pts',(-0.0122789627531435,-0.0405148032305823,
-0.0110118323957042));
#48117=CARTESIAN_POINT('Ctrl Pts',(-0.0124527083563813,-0.040525845043314,
-0.0110013257627274));
#48118=CARTESIAN_POINT('Ctrl Pts',(-0.0124763651716116,-0.04052732303004,
-0.0110006128129772));
#48119=CARTESIAN_POINT('Ctrl Pts',(-0.0124999999999997,-0.0405287743898722,
-0.0110006128129772));
#48120=CARTESIAN_POINT('Origin',(-0.0125,-0.0332787743898722,-0.0121758532865583));
#48121=CARTESIAN_POINT('',(-0.0125,-0.0410912743898722,-0.0110006128129772));
#48122=CARTESIAN_POINT('',(-0.0124999999999998,-0.0410287743898722,-0.0110006128129772));
#48123=CARTESIAN_POINT('',(-0.0125,-0.0332787743898722,-0.0110006128129775));
#48124=CARTESIAN_POINT('Ctrl Pts',(-0.0125,-0.0410912743898722,-0.0110006128129772));
#48125=CARTESIAN_POINT('Ctrl Pts',(-0.0123548775896907,-0.0410823627602376,
-0.0110006128129772));
#48126=CARTESIAN_POINT('Ctrl Pts',(-0.0122108943568779,-0.041072568120321,
-0.0110274919124065));
#48127=CARTESIAN_POINT('Ctrl Pts',(-0.0119307969650165,-0.0410515199816448,
-0.0111360279858138));
#48128=CARTESIAN_POINT('Ctrl Pts',(-0.0117987260605142,-0.0410404288340674,
-0.0112201088417681));
#48129=CARTESIAN_POINT('Ctrl Pts',(-0.0115760633306248,-0.0410191892648834,
-0.011433524112961));
#48130=CARTESIAN_POINT('Ctrl Pts',(-0.0114872140610908,-0.0410099251588461,
-0.0115602514817448));
#48131=CARTESIAN_POINT('Ctrl Pts',(-0.011364086873253,-0.0409901853892517,
-0.0118386391957428));
#48132=CARTESIAN_POINT('Ctrl Pts',(-0.0113302016880243,-0.0409796468095926,
-0.0119872635799372));
#48133=CARTESIAN_POINT('Ctrl Pts',(-0.0113203334694503,-0.0409578202638131,
-0.0122950808599193));
#48134=CARTESIAN_POINT('Ctrl Pts',(-0.0113467841610049,-0.0409467346962911,
-0.0124514193514131));
#48135=CARTESIAN_POINT('Ctrl Pts',(-0.011456938022439,-0.0409264387295969,
-0.0127376510495263));
#48136=CARTESIAN_POINT('Ctrl Pts',(-0.011536866112814,-0.0409176251035845,
-0.0128657598126419));
#48137=CARTESIAN_POINT('Ctrl Pts',(-0.0117426955931429,-0.0408971252952279,
-0.0130874656025689));
#48138=CARTESIAN_POINT('Ctrl Pts',(-0.011867522589383,-0.0408862464190323,
-0.0131781059976171));
#48139=CARTESIAN_POINT('Ctrl Pts',(-0.01214760848416,-0.0408644488917028,
-0.0133077990695779));
#48140=CARTESIAN_POINT('Ctrl Pts',(-0.0123006978574228,-0.0408537461000921,
-0.0133445209901367));
#48141=CARTESIAN_POINT('Ctrl Pts',(-0.0126053999752747,-0.0408346351553067,
-0.0133558003800468));
#48142=CARTESIAN_POINT('Ctrl Pts',(-0.0127540204427141,-0.0408250326230259,
-0.0133329585108336));
#48143=CARTESIAN_POINT('Ctrl Pts',(-0.0130401150017559,-0.0408038500644697,
-0.0132310184192814));
#48144=CARTESIAN_POINT('Ctrl Pts',(-0.0131741043111917,-0.0407927809827804,
-0.0131508827235366));
#48145=CARTESIAN_POINT('Ctrl Pts',(-0.0134033354827007,-0.0407713470972686,
-0.0129433634850405));
#48146=CARTESIAN_POINT('Ctrl Pts',(-0.0134963085598998,-0.0407618121420599,
-0.0128180669999191));
#48147=CARTESIAN_POINT('Ctrl Pts',(-0.0136268179943227,-0.0407422481188121,
-0.0125421578165565));
#48148=CARTESIAN_POINT('Ctrl Pts',(-0.0136644411031342,-0.0407318021814487,
-0.0123948399560682));
#48149=CARTESIAN_POINT('Ctrl Pts',(-0.0136823755998282,-0.0407100587418727,
-0.0120881947133739));
#48150=CARTESIAN_POINT('Ctrl Pts',(-0.0136602009649822,-0.0406989575063841,
-0.011931635258338));
#48151=CARTESIAN_POINT('Ctrl Pts',(-0.0135579048804031,-0.0406784469761072,
-0.0116423775945446));
#48152=CARTESIAN_POINT('Ctrl Pts',(-0.013481147287524,-0.040669644045422,
-0.0115116924477378));
#48153=CARTESIAN_POINT('Ctrl Pts',(-0.0132810701416322,-0.0406493060166953,
-0.0112845864415585));
#48154=CARTESIAN_POINT('Ctrl Pts',(-0.0131590177303542,-0.0406384899075225,
-0.0111909107166815));
#48155=CARTESIAN_POINT('Ctrl Pts',(-0.012882875624152,-0.0406166732625263,
-0.0110538475739989));
#48156=CARTESIAN_POINT('Ctrl Pts',(-0.0127308073952225,-0.040605886706129,
-0.0110129943291534));
#48157=CARTESIAN_POINT('Ctrl Pts',(-0.0125501152010411,-0.0405943802337429,
-0.0110014134606557));
#48158=CARTESIAN_POINT('Ctrl Pts',(-0.0125250463681162,-0.0405928124290756,
-0.0110006128129772));
#48159=CARTESIAN_POINT('Ctrl Pts',(-0.0125000000000003,-0.0405912743898722,
-0.0110006128129772));
#48160=CARTESIAN_POINT('Ctrl Pts',(-0.0124999999999997,-0.0405287743898722,
-0.0110006128129772));
#48161=CARTESIAN_POINT('Ctrl Pts',(-0.0126316492011669,-0.0405368586610747,
-0.0110006128129772));
#48162=CARTESIAN_POINT('Ctrl Pts',(-0.01276252108623,-0.0405456791622419,
-0.0110227250980209));
#48163=CARTESIAN_POINT('Ctrl Pts',(-0.0130328277311265,-0.0405656219601255,
-0.0111170422529395));
#48164=CARTESIAN_POINT('Ctrl Pts',(-0.0131670559572858,-0.0405766655639931,
-0.0111960455111696));
#48165=CARTESIAN_POINT('Ctrl Pts',(-0.0133933766330118,-0.04059771872837,
-0.011397867342952));
#48166=CARTESIAN_POINT('Ctrl Pts',(-0.0134846584814694,-0.0406070718370568,
-0.0115172125231013));
#48167=CARTESIAN_POINT('Ctrl Pts',(-0.0136209585899284,-0.0406264070596672,
-0.01178989495723));
#48168=CARTESIAN_POINT('Ctrl Pts',(-0.0136622101576207,-0.040637181921104,
-0.0119418515963219));
#48169=CARTESIAN_POINT('Ctrl Pts',(-0.0136827973122141,-0.0406589967920181,
-0.0122495042270127));
#48170=CARTESIAN_POINT('Ctrl Pts',(-0.0136632805833491,-0.0406698224985453,
-0.0124021779286026));
#48171=CARTESIAN_POINT('Ctrl Pts',(-0.0135677388273238,-0.0406901843280577,
-0.0126893384825128));
#48172=CARTESIAN_POINT('Ctrl Pts',(-0.0134935014969514,-0.0406989849587138,
-0.0128213663775835));
#48173=CARTESIAN_POINT('Ctrl Pts',(-0.0132951011885483,-0.0407194644182024,
-0.0130553659152251));
#48174=CARTESIAN_POINT('Ctrl Pts',(-0.0131709389336876,-0.0407305638598057,
-0.013153378893578));
#48175=CARTESIAN_POINT('Ctrl Pts',(-0.0128968384027453,-0.0407523203922931,
-0.0132922826286567));
#48176=CARTESIAN_POINT('Ctrl Pts',(-0.0127505474487945,-0.040762780316068,
-0.0133339294822274));
#48177=CARTESIAN_POINT('Ctrl Pts',(-0.0124465718431961,-0.0407823703629212,
-0.0133599806716566));
#48178=CARTESIAN_POINT('Ctrl Pts',(-0.0122916981336773,-0.0407918616754559,
-0.0133427461909457));
#48179=CARTESIAN_POINT('Ctrl Pts',(-0.0119970897781494,-0.0408132673576658,
-0.0132492590527113));
#48180=CARTESIAN_POINT('Ctrl Pts',(-0.0118603276335144,-0.0408243402237439,
-0.0131738193068051));
#48181=CARTESIAN_POINT('Ctrl Pts',(-0.0116281332740182,-0.0408455448570753,
-0.0129778986950418));
#48182=CARTESIAN_POINT('Ctrl Pts',(-0.0115335545124742,-0.0408551950161598,
-0.0128609626405736));
#48183=CARTESIAN_POINT('Ctrl Pts',(-0.0113898949659606,-0.0408742670671095,
-0.0125919916862903));
#48184=CARTESIAN_POINT('Ctrl Pts',(-0.0113445553085114,-0.0408849568884158,
-0.0124412343584372));
#48185=CARTESIAN_POINT('Ctrl Pts',(-0.0113156036100202,-0.0409067502437709,
-0.0121338851592148));
#48186=CARTESIAN_POINT('Ctrl Pts',(-0.0113310948019909,-0.0409176377101116,
-0.0119803404660346));
#48187=CARTESIAN_POINT('Ctrl Pts',(-0.0114190735704893,-0.0409381609338805,
-0.0116909037873758));
#48188=CARTESIAN_POINT('Ctrl Pts',(-0.0114895011411379,-0.0409469813107143,
-0.0115574143384823));
#48189=CARTESIAN_POINT('Ctrl Pts',(-0.0116813502541496,-0.0409672455638847,
-0.0113181378577776));
#48190=CARTESIAN_POINT('Ctrl Pts',(-0.011803170496375,-0.0409783281814259,
-0.0112165429301995));
#48191=CARTESIAN_POINT('Ctrl Pts',(-0.0120742257497072,-0.0410001655970101,
-0.0110700832494386));
#48192=CARTESIAN_POINT('Ctrl Pts',(-0.0122197649150521,-0.0410107171066086,
-0.0110245510110078));
#48193=CARTESIAN_POINT('Ctrl Pts',(-0.012413223120115,-0.0410233605342975,
-0.0110030128206424));
#48194=CARTESIAN_POINT('Ctrl Pts',(-0.0124566341580664,-0.0410261113943963,
-0.0110006128129772));
#48195=CARTESIAN_POINT('Ctrl Pts',(-0.0124999999999995,-0.0410287743898722,
-0.0110006128129772));
#48196=CARTESIAN_POINT('Origin',(-0.0125,-0.0332787743898722,-0.0121758532865583));
#48197=CARTESIAN_POINT('',(-0.0125,-0.0412787743898722,-0.0133510937601389));
#48198=CARTESIAN_POINT('Ctrl Pts',(-0.0124999999999995,-0.0410287743898722,
-0.0110006128129772));
#48199=CARTESIAN_POINT('Ctrl Pts',(-0.0126092287281941,-0.0410354818719837,
-0.0110006128129772));
#48200=CARTESIAN_POINT('Ctrl Pts',(-0.0127181041723048,-0.041042707274917,
-0.0110158330752455));
#48201=CARTESIAN_POINT('Ctrl Pts',(-0.0129726558544088,-0.0410609229844915,
-0.0110887247682153));
#48202=CARTESIAN_POINT('Ctrl Pts',(-0.0131118546394638,-0.0410720166165589,
-0.011160529849858));
#48203=CARTESIAN_POINT('Ctrl Pts',(-0.0133498817563325,-0.0410933681826564,
-0.0113504921815146));
#48204=CARTESIAN_POINT('Ctrl Pts',(-0.01344776359209,-0.0411033746613979,
-0.0114650716774333));
#48205=CARTESIAN_POINT('Ctrl Pts',(-0.0135986340666582,-0.0411221828298088,
-0.0117303211264384));
#48206=CARTESIAN_POINT('Ctrl Pts',(-0.0136479608843726,-0.0411327811340702,
-0.0118797877998699));
#48207=CARTESIAN_POINT('Ctrl Pts',(-0.0136851419072229,-0.041154537430138,
-0.0121866143561989));
#48208=CARTESIAN_POINT('Ctrl Pts',(-0.0136736432711152,-0.0411654784113469,
-0.0123409137634469));
#48209=CARTESIAN_POINT('Ctrl Pts',(-0.0135931189592482,-0.0411861566755532,
-0.0126325369596714));
#48210=CARTESIAN_POINT('Ctrl Pts',(-0.0135263707615743,-0.0411950561575114,
-0.0127674827454629));
#48211=CARTESIAN_POINT('Ctrl Pts',(-0.0133409298539512,-0.0412151061529174,
-0.0130118152579657));
#48212=CARTESIAN_POINT('Ctrl Pts',(-0.0132214777881316,-0.0412261647845225,
-0.013116835445569));
#48213=CARTESIAN_POINT('Ctrl Pts',(-0.012994751607665,-0.0412447000772217,
-0.0132469364096699));
#48214=CARTESIAN_POINT('Ctrl Pts',(-0.0128981046712635,-0.0412520372742158,
-0.0132864903063074));
#48215=CARTESIAN_POINT('Ctrl Pts',(-0.0127003151194289,-0.0412660180234459,
-0.0133382465696333));
#48216=CARTESIAN_POINT('Ctrl Pts',(-0.0126003261699996,-0.0412726135931504,
-0.0133510937601389));
#48217=CARTESIAN_POINT('Ctrl Pts',(-0.0125,-0.0412787743898722,-0.0133510937601389));
#48218=CARTESIAN_POINT('',(-0.0133234078741649,-0.0412787743898722,-0.0130144173231741));
#48219=CARTESIAN_POINT('Origin',(-0.0125,-0.0412787743898622,-0.0121758532865681));
#48220=CARTESIAN_POINT('Ctrl Pts',(-0.0133234078741641,-0.0412787743898723,
-0.0130144173231748));
#48221=CARTESIAN_POINT('Ctrl Pts',(-0.0133804118658089,-0.0412732894303495,
-0.0129584436186877));
#48222=CARTESIAN_POINT('Ctrl Pts',(-0.0134315632959738,-0.0412679629049933,
-0.012896801738238));
#48223=CARTESIAN_POINT('Ctrl Pts',(-0.0135195542403086,-0.0412579077593073,
-0.0127655933841637));
#48224=CARTESIAN_POINT('Ctrl Pts',(-0.0135564571086821,-0.0412531998817753,
-0.0126966092776548));
#48225=CARTESIAN_POINT('Ctrl Pts',(-0.0136440663276741,-0.0412381566833437,
-0.0124844567698673));
#48226=CARTESIAN_POINT('Ctrl Pts',(-0.0136742623513739,-0.0412275341252433,
-0.0123346480473168));
#48227=CARTESIAN_POINT('Ctrl Pts',(-0.0136762096598467,-0.0412056406865503,
-0.0120258873842219));
#48228=CARTESIAN_POINT('Ctrl Pts',(-0.013645579755795,-0.0411945781586684,
-0.0118698738181379));
#48229=CARTESIAN_POINT('Ctrl Pts',(-0.0135277857927238,-0.0411744971694781,
-0.0115866739231869));
#48230=CARTESIAN_POINT('Ctrl Pts',(-0.0134447390385254,-0.041165612675012,
-0.0114610454727467));
#48231=CARTESIAN_POINT('Ctrl Pts',(-0.013233255127403,-0.0411449565068602,
-0.0112447231956079));
#48232=CARTESIAN_POINT('Ctrl Pts',(-0.0131057542452771,-0.041134022784958,
-0.0111571671413067));
#48233=CARTESIAN_POINT('Ctrl Pts',(-0.0128219593983773,-0.0411122601814962,
-0.0110348832174941));
#48234=CARTESIAN_POINT('Ctrl Pts',(-0.0126679731986536,-0.0411016482238126,
-0.0110022766869115));
#48235=CARTESIAN_POINT('Ctrl Pts',(-0.0125080492209149,-0.0410917694066109,
-0.0110006334823458));
#48236=CARTESIAN_POINT('Ctrl Pts',(-0.0125040242169056,-0.0410915215076713,
-0.0110006128129772));
#48237=CARTESIAN_POINT('Ctrl Pts',(-0.0125,-0.0410912743898722,-0.0110006128129772));
#48238=CARTESIAN_POINT('Origin',(-0.0125,-0.0332787743898722,-0.0121758532865583));
#48239=CARTESIAN_POINT('',(-0.0114490560961669,-0.0336537743898722,-0.0132461415239019));
#48240=CARTESIAN_POINT('Ctrl Pts',(-0.0125,-0.0340912743898723,-0.0136758532865583));
#48241=CARTESIAN_POINT('Ctrl Pts',(-0.0126865058990789,-0.034082301120619,
-0.0136758532865583));
#48242=CARTESIAN_POINT('Ctrl Pts',(-0.0128715278361501,-0.034072433085725,
-0.0136410714258962));
#48243=CARTESIAN_POINT('Ctrl Pts',(-0.0132281311189972,-0.0340514085142548,
-0.0135018418570036));
#48244=CARTESIAN_POINT('Ctrl Pts',(-0.0133949927443967,-0.0340404250085348,
-0.01339544846411));
#48245=CARTESIAN_POINT('Ctrl Pts',(-0.0136739994535825,-0.0340195903567862,
-0.0131286547971216));
#48246=CARTESIAN_POINT('Ctrl Pts',(-0.0137851071224222,-0.0340105306671531,
-0.0129724662776123));
#48247=CARTESIAN_POINT('Ctrl Pts',(-0.0139468394462665,-0.0339908834189933,
-0.0126188158107363));
#48248=CARTESIAN_POINT('Ctrl Pts',(-0.0139927523118229,-0.0339800215216224,
-0.0124233016580604));
#48249=CARTESIAN_POINT('Ctrl Pts',(-0.014005500907111,-0.0339582209318096,
-0.012030891041432));
#48250=CARTESIAN_POINT('Ctrl Pts',(-0.0139742069066131,-0.0339474941284978,
-0.0118378085818187));
#48251=CARTESIAN_POINT('Ctrl Pts',(-0.0138402998090658,-0.0339273583028217,
-0.0114753637196494));
#48252=CARTESIAN_POINT('Ctrl Pts',(-0.0137394094121885,-0.0339185005932602,
-0.0113092765352342));
#48253=CARTESIAN_POINT('Ctrl Pts',(-0.0134759260038074,-0.0338977738088027,
-0.0110194789450359));
#48254=CARTESIAN_POINT('Ctrl Pts',(-0.0133140161039499,-0.0338866737715003,
-0.0109003137749483));
#48255=CARTESIAN_POINT('Ctrl Pts',(-0.0129599674645763,-0.0338650565873608,
-0.0107353253776746));
#48256=CARTESIAN_POINT('Ctrl Pts',(-0.0127724186379477,-0.0338547298172228,
-0.0106884057493268));
#48257=CARTESIAN_POINT('Ctrl Pts',(-0.0123823768892991,-0.0338353773191225,
-0.0106672879434466));
#48258=CARTESIAN_POINT('Ctrl Pts',(-0.0121834681583582,-0.0338254806902787,
-0.0106961772399881));
#48259=CARTESIAN_POINT('Ctrl Pts',(-0.0118108159569984,-0.0338038583631424,
-0.0108291284705843));
#48260=CARTESIAN_POINT('Ctrl Pts',(-0.011640445856798,-0.03379283334398,
-0.0109309394907954));
#48261=CARTESIAN_POINT('Ctrl Pts',(-0.0113536108241396,-0.0337718363246642,
-0.011190019336208));
#48262=CARTESIAN_POINT('Ctrl Pts',(-0.0112381479744462,-0.0337625486841728,
-0.0113429159891473));
#48263=CARTESIAN_POINT('Ctrl Pts',(-0.0110664258426459,-0.0337431724471388,
-0.0116916882557595));
#48264=CARTESIAN_POINT('Ctrl Pts',(-0.0110149454443092,-0.0337323894588582,
-0.0118857820448108));
#48265=CARTESIAN_POINT('Ctrl Pts',(-0.0109909321084533,-0.0337105900329636,
-0.0122781717109137));
#48266=CARTESIAN_POINT('Ctrl Pts',(-0.0110168590975054,-0.0336997884198633,
-0.0124726007467192));
#48267=CARTESIAN_POINT('Ctrl Pts',(-0.0111164765646197,-0.0336834345323847,
-0.0127669707213344));
#48268=CARTESIAN_POINT('Ctrl Pts',(-0.0111664960347912,-0.0336777481173169,
-0.0128724957183858));
#48269=CARTESIAN_POINT('Ctrl Pts',(-0.0112907586203285,-0.0336662497993814,
-0.0130712060524302));
#48270=CARTESIAN_POINT('Ctrl Pts',(-0.0113648883876633,-0.0336601196457954,
-0.0131634950581508));
#48271=CARTESIAN_POINT('Ctrl Pts',(-0.0114490560961676,-0.0336537743898721,
-0.0132461415239026));
#48272=CARTESIAN_POINT('',(-0.011,-0.0336537743898722,-0.0121758532865583));
#48273=CARTESIAN_POINT('Origin',(-0.0125,-0.0336537743898622,-0.0121758532865683));
#48274=CARTESIAN_POINT('Ctrl Pts',(-0.011,-0.0336537743898722,-0.0121758532865583));
#48275=CARTESIAN_POINT('Ctrl Pts',(-0.011,-0.0336598131811276,-0.012067155043962));
#48276=CARTESIAN_POINT('Ctrl Pts',(-0.0110118138630113,-0.033665833784502,
-0.0119587841832224));
#48277=CARTESIAN_POINT('Ctrl Pts',(-0.0110581181358939,-0.033677491560012,
-0.0117489442240407));
#48278=CARTESIAN_POINT('Ctrl Pts',(-0.0110919458322686,-0.0336831013287107,
-0.0116479683874627));
#48279=CARTESIAN_POINT('Ctrl Pts',(-0.0112152450407584,-0.0336980621721267,
-0.0113786732059739));
#48280=CARTESIAN_POINT('Ctrl Pts',(-0.0113264197757561,-0.0337071248536072,
-0.0112225360169443));
#48281=CARTESIAN_POINT('Ctrl Pts',(-0.0116055473928061,-0.0337279620395113,
-0.0109558605389212));
#48282=CARTESIAN_POINT('Ctrl Pts',(-0.0117724639540535,-0.0337389462523888,
-0.010849536840037));
#48283=CARTESIAN_POINT('Ctrl Pts',(-0.0121403888485598,-0.0337606329661552,
-0.0107060797551005));
#48284=CARTESIAN_POINT('Ctrl Pts',(-0.0123381557525508,-0.0337708645442542,
-0.0106714213038118));
#48285=CARTESIAN_POINT('Ctrl Pts',(-0.0127278533839575,-0.033789880000058,
-0.0106810016155603));
#48286=CARTESIAN_POINT('Ctrl Pts',(-0.0129161653791794,-0.0338000829023891,
-0.0107221401560805));
#48287=CARTESIAN_POINT('Ctrl Pts',(-0.0132740104284418,-0.0338215665082543,
-0.0108757441606687));
#48288=CARTESIAN_POINT('Ctrl Pts',(-0.0134390322491703,-0.0338326640503305,
-0.0109894294975537));
#48289=CARTESIAN_POINT('Ctrl Pts',(-0.0137120587246422,-0.0338536255042462,
-0.0112711461111903));
#48290=CARTESIAN_POINT('Ctrl Pts',(-0.013818692018525,-0.0338626247106024,
-0.0114351590597035));
#48291=CARTESIAN_POINT('Ctrl Pts',(-0.0139634404810105,-0.0338825695688823,
-0.0117941665087412));
#48292=CARTESIAN_POINT('Ctrl Pts',(-0.014000384202204,-0.033893207922565,
-0.0119856568750299));
#48293=CARTESIAN_POINT('Ctrl Pts',(-0.0139995943191151,-0.0339151032556719,
-0.0123797728709541));
#48294=CARTESIAN_POINT('Ctrl Pts',(-0.0139588294412269,-0.0339261489516028,
-0.0125785953977098));
#48295=CARTESIAN_POINT('Ctrl Pts',(-0.0138055677454885,-0.0339461458362204,
-0.0129385393208265));
#48296=CARTESIAN_POINT('Ctrl Pts',(-0.0136984249594945,-0.033955058052392,
-0.0130977980561763));
#48297=CARTESIAN_POINT('Ctrl Pts',(-0.0134265815783181,-0.0339757411420657,
-0.0133715427365305));
#48298=CARTESIAN_POINT('Ctrl Pts',(-0.0132630145914569,-0.0339866791278434,
-0.0134820038928433));
#48299=CARTESIAN_POINT('Ctrl Pts',(-0.0128997595351416,-0.0340084116489645,
-0.0136351984395573));
#48300=CARTESIAN_POINT('Ctrl Pts',(-0.0127030752966334,-0.0340189880275693,
-0.0136752809751883));
#48301=CARTESIAN_POINT('Ctrl Pts',(-0.0125028480827704,-0.0340286373050992,
-0.0136758512587937));
#48302=CARTESIAN_POINT('Ctrl Pts',(-0.0125014239907197,-0.0340287058780863,
-0.0136758532865732));
#48303=CARTESIAN_POINT('Ctrl Pts',(-0.0124999999842539,-0.0340287743906298,
-0.0136758532865583));
#48304=CARTESIAN_POINT('Origin',(-0.0125,-0.0429287743898722,-0.012175853286558));
#48305=CARTESIAN_POINT('',(-0.0115,-0.0429287743898722,-0.0127532035557476));
#48306=CARTESIAN_POINT('',(-0.0115,-0.0429287743898722,-0.0115985030173684));
#48307=CARTESIAN_POINT('Ctrl Pts',(-0.01149999999999,-0.0429287743898622,
-0.0127532035557576));
#48308=CARTESIAN_POINT('Ctrl Pts',(-0.01149999999999,-0.0426400992552674,
-0.012175853286548));
#48309=CARTESIAN_POINT('Ctrl Pts',(-0.01149999999999,-0.0429287743898621,
-0.0115985030173584));
#48310=CARTESIAN_POINT('Origin',(-0.0125,-0.0429287743898722,-0.012175853286558));
#48311=CARTESIAN_POINT('Origin',(-0.0125,-0.0429287743898722,-0.012175853286558));
#48312=CARTESIAN_POINT('',(-0.01535,-0.0415262743898622,-0.0121758532865581));
#48313=CARTESIAN_POINT('Origin',(-0.0125,-0.0415262743898622,-0.012175853286558));
#48314=CARTESIAN_POINT('',(-0.01535,-0.0412787743898622,-0.0121758532865581));
#48315=CARTESIAN_POINT('',(-0.01535,-0.0429287743898722,-0.012175853286558));
#48316=CARTESIAN_POINT('Origin',(-0.0125,-0.0412787743898622,-0.0121758532865581));
#48317=CARTESIAN_POINT('Origin',(-0.0125,-0.0401339415021717,-0.0121758532865581));
#48318=CARTESIAN_POINT('',(-0.01099999999999,-0.0429287743898722,-0.012175853286558));
#48319=CARTESIAN_POINT('Origin',(-0.0125,-0.0429287743898722,-0.012175853286558));
#48320=CARTESIAN_POINT('Origin',(-0.0125,-0.0332787743898722,-0.0121758532865583));
#48321=CARTESIAN_POINT('',(-0.0125000000000002,-0.0334556573285548,-0.0108739703478756));
#48322=CARTESIAN_POINT('Ctrl Pts',(-0.0125000000000003,-0.0334556573285548,
-0.0108739703478756));
#48323=CARTESIAN_POINT('Ctrl Pts',(-0.0125169619654304,-0.0334562534372814,
-0.0108733742391491));
#48324=CARTESIAN_POINT('Ctrl Pts',(-0.0125342659303904,-0.0334568674696437,
-0.010873091500204));
#48325=CARTESIAN_POINT('Ctrl Pts',(-0.0127142374842031,-0.0334633195025884,
-0.0108738056395374));
#48326=CARTESIAN_POINT('Ctrl Pts',(-0.0128750636210282,-0.0334696175052002,
-0.0109042115888364));
#48327=CARTESIAN_POINT('Ctrl Pts',(-0.0131894625396203,-0.0334829915682975,
-0.0110260726974655));
#48328=CARTESIAN_POINT('Ctrl Pts',(-0.0133384354713308,-0.0334899589420527,
-0.0111208842865654));
#48329=CARTESIAN_POINT('Ctrl Pts',(-0.0136233142077324,-0.0335048715041686,
-0.0113937017075726));
#48330=CARTESIAN_POINT('Ctrl Pts',(-0.0137145126457393,-0.0335107921955676,
-0.0115560798170348));
#48331=CARTESIAN_POINT('Ctrl Pts',(-0.013836412057102,-0.0335218194362954,
-0.0118362950864762));
#48332=CARTESIAN_POINT('Ctrl Pts',(-0.0138749679863545,-0.0335284104154649,
-0.0120060666246319));
#48333=CARTESIAN_POINT('Ctrl Pts',(-0.0138878583928345,-0.0335419895541559,
-0.0123611092928754));
#48334=CARTESIAN_POINT('Ctrl Pts',(-0.013858168381701,-0.0335488446104762,
-0.012543202792378));
#48335=CARTESIAN_POINT('Ctrl Pts',(-0.0137239184314785,-0.0335621176892281,
-0.0129003899279641));
#48336=CARTESIAN_POINT('Ctrl Pts',(-0.0136197865853707,-0.0335679593652523,
-0.0130553133704129));
#48337=CARTESIAN_POINT('Ctrl Pts',(-0.0133828554998308,-0.0335804785640777,
-0.0133114304431047));
#48338=CARTESIAN_POINT('Ctrl Pts',(-0.0132339030198478,-0.0335872828023574,
-0.0134207688274427));
#48339=CARTESIAN_POINT('Ctrl Pts',(-0.0128973989337005,-0.0336008366112022,
-0.013580065947054));
#48340=CARTESIAN_POINT('Ctrl Pts',(-0.0127120297926521,-0.0336074446543075,
-0.013626361460001));
#48341=CARTESIAN_POINT('Ctrl Pts',(-0.0123890809311569,-0.0336176648068571,
-0.0136416742981176));
#48342=CARTESIAN_POINT('Ctrl Pts',(-0.0122064915470854,-0.0336235752447987,
-0.0136317811264738));
#48343=CARTESIAN_POINT('Ctrl Pts',(-0.0119011769375834,-0.033634839900917,
-0.0135346618859548));
#48344=CARTESIAN_POINT('Ctrl Pts',(-0.011803178818122,-0.0336386438976925,
-0.01349140338373));
#48345=CARTESIAN_POINT('Ctrl Pts',(-0.011616721475776,-0.0336462744782102,
-0.0133837962791914));
#48346=CARTESIAN_POINT('Ctrl Pts',(-0.0115290003612504,-0.0336500773154259,
-0.0133194594616579));
#48347=CARTESIAN_POINT('Ctrl Pts',(-0.0114490560961663,-0.0336537743898722,
-0.0132461415239012));
#48348=CARTESIAN_POINT('',(-0.0125,-0.0332787743898522,-0.0110508532865583));
#48349=CARTESIAN_POINT('',(-0.0125,-0.0332787743898722,-0.0110508532865583));
#48350=CARTESIAN_POINT('Origin',(-0.0125,-0.0332787743898622,-0.0121758532865683));
#48351=CARTESIAN_POINT('Ctrl Pts',(-0.0118107823295555,-0.0333290148634531,
-0.0131277824716817));
#48352=CARTESIAN_POINT('Ctrl Pts',(-0.0117098836135435,-0.0333344102607298,
-0.0130613906751724));
#48353=CARTESIAN_POINT('Ctrl Pts',(-0.0116198784781834,-0.0333396492883259,
-0.0129797529105212));
#48354=CARTESIAN_POINT('Ctrl Pts',(-0.0114414223014775,-0.0333512035863472,
-0.0127588129791921));
#48355=CARTESIAN_POINT('Ctrl Pts',(-0.0113846754137903,-0.0333562632427286,
-0.012634703796091));
#48356=CARTESIAN_POINT('Ctrl Pts',(-0.0112970495906885,-0.0333667457898664,
-0.0123985832942005));
#48357=CARTESIAN_POINT('Ctrl Pts',(-0.011271377129027,-0.0333736872268549,
-0.012239621846769));
#48358=CARTESIAN_POINT('Ctrl Pts',(-0.0112822066210525,-0.0333869145783074,
-0.0119314481530083));
#48359=CARTESIAN_POINT('Ctrl Pts',(-0.0113145866019927,-0.0333931041250635,
-0.0117848682419702));
#48360=CARTESIAN_POINT('Ctrl Pts',(-0.0114373374471298,-0.0334052173218674,
-0.0114942642325391));
#48361=CARTESIAN_POINT('Ctrl Pts',(-0.0115333961603035,-0.0334113688630093,
-0.0113542906673467));
#48362=CARTESIAN_POINT('Ctrl Pts',(-0.0117691046885344,-0.0334248437865918,
-0.0111232097728938));
#48363=CARTESIAN_POINT('Ctrl Pts',(-0.0119066804715653,-0.033431670970877,
-0.0110323315484945));
#48364=CARTESIAN_POINT('Ctrl Pts',(-0.0121561556995369,-0.03344260130431,
-0.0109291835302698));
#48365=CARTESIAN_POINT('Ctrl Pts',(-0.0123055738989379,-0.0334488244473071,
-0.0108808032291233));
#48366=CARTESIAN_POINT('Ctrl Pts',(-0.0125000000000003,-0.0334556573285548,
-0.0108739703478756));
#48367=CARTESIAN_POINT('Ctrl Pts',(-0.0126906536866924,-0.033329014863453,
-0.013335526232907));
#48368=CARTESIAN_POINT('Ctrl Pts',(-0.0125279740652511,-0.0333555799941742,
-0.0133891929900586));
#48369=CARTESIAN_POINT('Ctrl Pts',(-0.0123661654682192,-0.0333769910786535,
-0.0134004654915067));
#48370=CARTESIAN_POINT('Ctrl Pts',(-0.0120636132777685,-0.033422430336011,
-0.0133770070013701));
#48371=CARTESIAN_POINT('Ctrl Pts',(-0.0119118500123405,-0.033446157237979,
-0.0133369191787743));
#48372=CARTESIAN_POINT('Ctrl Pts',(-0.0116282619419881,-0.0334925065907822,
-0.0132037360390814));
#48373=CARTESIAN_POINT('Ctrl Pts',(-0.0114990164583931,-0.0335147508070644,
-0.0131111612382107));
#48374=CARTESIAN_POINT('Ctrl Pts',(-0.0112596605338127,-0.0335595060136002,
-0.0128628817337503));
#48375=CARTESIAN_POINT('Ctrl Pts',(-0.0111769727528737,-0.0335788237730028,
-0.0127188109969073));
#48376=CARTESIAN_POINT('Ctrl Pts',(-0.0110621505149206,-0.0336140810688488,
-0.0124717801731789));
#48377=CARTESIAN_POINT('Ctrl Pts',(-0.0110197071274521,-0.0336340672624201,
-0.012325779104587));
#48378=CARTESIAN_POINT('Ctrl Pts',(-0.011,-0.0336537743898722,-0.0121758532865583));
#48379=CARTESIAN_POINT('Origin',(-0.0125,-0.0332787743898722,-0.0136758532865583));
#48380=CARTESIAN_POINT('Ctrl Pts',(-0.0124879391534221,-0.033279517212585,
-0.0133510318715922));
#48381=CARTESIAN_POINT('Ctrl Pts',(-0.0118174660837529,-0.0333209333633904,
-0.0133441508128911));
#48382=CARTESIAN_POINT('Ctrl Pts',(-0.0114822118943233,-0.0333621077232055,
-0.0127634735233487));
#48383=CARTESIAN_POINT('Ctrl Pts',(-0.0111429491924311,-0.0334037743898722,
-0.0121758532865583));
#48384=CARTESIAN_POINT('Ctrl Pts',(-0.0114822118943233,-0.0334454410565388,
-0.0115882330497679));
#48385=CARTESIAN_POINT('Ctrl Pts',(-0.0118214745962156,-0.0334871077232055,
-0.0110006128129775));
#48386=CARTESIAN_POINT('Ctrl Pts',(-0.0125,-0.0335287743898722,-0.0110006128129775));
#48387=CARTESIAN_POINT('Ctrl Pts',(-0.0131785254037844,-0.0335704410565388,
-0.0110006128129775));
#48388=CARTESIAN_POINT('Ctrl Pts',(-0.0135177881056766,-0.0336121077232055,
-0.0115882330497679));
#48389=CARTESIAN_POINT('Ctrl Pts',(-0.0138570508075689,-0.0336537743898722,
-0.0121758532865583));
#48390=CARTESIAN_POINT('Ctrl Pts',(-0.0135177881056766,-0.0336954410565389,
-0.0127634735233487));
#48391=CARTESIAN_POINT('Ctrl Pts',(-0.0131785254037844,-0.0337371077232056,
-0.0133510937601391));
#48392=CARTESIAN_POINT('Ctrl Pts',(-0.0125,-0.0337787743898723,-0.0133510937601391));
#48393=CARTESIAN_POINT('Ctrl Pts',(-0.0118214745962156,-0.0338204410565389,
-0.0133510937601391));
#48394=CARTESIAN_POINT('Ctrl Pts',(-0.0114822118943233,-0.0338621077232055,
-0.0127634735233487));
#48395=CARTESIAN_POINT('Ctrl Pts',(-0.0111429491924311,-0.0339037743898722,
-0.0121758532865583));
#48396=CARTESIAN_POINT('Ctrl Pts',(-0.0114822118943233,-0.0339454410565388,
-0.0115882330497679));
#48397=CARTESIAN_POINT('Ctrl Pts',(-0.0118214745962156,-0.0339871077232055,
-0.0110006128129775));
#48398=CARTESIAN_POINT('Ctrl Pts',(-0.0125,-0.0340287743898722,-0.0110006128129775));
#48399=CARTESIAN_POINT('Ctrl Pts',(-0.0131785254037844,-0.0340704410565388,
-0.0110006128129775));
#48400=CARTESIAN_POINT('Ctrl Pts',(-0.0135177881056766,-0.0341121077232055,
-0.0115882330497679));
#48401=CARTESIAN_POINT('Ctrl Pts',(-0.0138570508075689,-0.0341537743898722,
-0.0121758532865583));
#48402=CARTESIAN_POINT('Ctrl Pts',(-0.0135177881056766,-0.0341954410565389,
-0.0127634735233487));
#48403=CARTESIAN_POINT('Ctrl Pts',(-0.0131785254037844,-0.0342371077232056,
-0.0133510937601391));
#48404=CARTESIAN_POINT('Ctrl Pts',(-0.0125,-0.0342787743898723,-0.0133510937601391));
#48405=CARTESIAN_POINT('Ctrl Pts',(-0.0118214745962156,-0.0343204410565389,
-0.0133510937601391));
#48406=CARTESIAN_POINT('Ctrl Pts',(-0.0114822118943233,-0.0343621077232055,
-0.0127634735233487));
#48407=CARTESIAN_POINT('Ctrl Pts',(-0.0111429491924311,-0.0344037743898722,
-0.0121758532865583));
#48408=CARTESIAN_POINT('Ctrl Pts',(-0.0114822118943233,-0.0344454410565389,
-0.0115882330497679));
#48409=CARTESIAN_POINT('Ctrl Pts',(-0.0118214745962156,-0.0344871077232055,
-0.0110006128129775));
#48410=CARTESIAN_POINT('Ctrl Pts',(-0.0125,-0.0345287743898722,-0.0110006128129775));
#48411=CARTESIAN_POINT('Ctrl Pts',(-0.0131785254037844,-0.0345704410565388,
-0.0110006128129775));
#48412=CARTESIAN_POINT('Ctrl Pts',(-0.0135177881056766,-0.0346121077232055,
-0.0115882330497679));
#48413=CARTESIAN_POINT('Ctrl Pts',(-0.0138570508075689,-0.0346537743898722,
-0.0121758532865583));
#48414=CARTESIAN_POINT('Ctrl Pts',(-0.0135177881056766,-0.0346954410565389,
-0.0127634735233487));
#48415=CARTESIAN_POINT('Ctrl Pts',(-0.0131785254037844,-0.0347371077232056,
-0.0133510937601391));
#48416=CARTESIAN_POINT('Ctrl Pts',(-0.0125,-0.0347787743898723,-0.0133510937601391));
#48417=CARTESIAN_POINT('Ctrl Pts',(-0.0118214745962156,-0.0348204410565389,
-0.0133510937601391));
#48418=CARTESIAN_POINT('Ctrl Pts',(-0.0114822118943233,-0.0348621077232055,
-0.0127634735233487));
#48419=CARTESIAN_POINT('Ctrl Pts',(-0.0111429491924311,-0.0349037743898722,
-0.0121758532865583));
#48420=CARTESIAN_POINT('Ctrl Pts',(-0.0114822118943233,-0.0349454410565389,
-0.0115882330497679));
#48421=CARTESIAN_POINT('Ctrl Pts',(-0.0118214745962156,-0.0349871077232055,
-0.0110006128129774));
#48422=CARTESIAN_POINT('Ctrl Pts',(-0.0125,-0.0350287743898722,-0.0110006128129774));
#48423=CARTESIAN_POINT('Ctrl Pts',(-0.0131785254037844,-0.0350704410565388,
-0.0110006128129774));
#48424=CARTESIAN_POINT('Ctrl Pts',(-0.0135177881056766,-0.0351121077232055,
-0.0115882330497678));
#48425=CARTESIAN_POINT('Ctrl Pts',(-0.0138570508075689,-0.0351537743898722,
-0.0121758532865583));
#48426=CARTESIAN_POINT('Ctrl Pts',(-0.0135177881056766,-0.0351954410565389,
-0.0127634735233487));
#48427=CARTESIAN_POINT('Ctrl Pts',(-0.0131785254037844,-0.0352371077232056,
-0.0133510937601391));
#48428=CARTESIAN_POINT('Ctrl Pts',(-0.0125,-0.0352787743898723,-0.0133510937601391));
#48429=CARTESIAN_POINT('Ctrl Pts',(-0.0118214745962156,-0.0353204410565389,
-0.0133510937601391));
#48430=CARTESIAN_POINT('Ctrl Pts',(-0.0114822118943233,-0.0353621077232055,
-0.0127634735233487));
#48431=CARTESIAN_POINT('Ctrl Pts',(-0.0111429491924311,-0.0354037743898722,
-0.0121758532865583));
#48432=CARTESIAN_POINT('Ctrl Pts',(-0.0114822118943233,-0.0354454410565389,
-0.0115882330497678));
#48433=CARTESIAN_POINT('Ctrl Pts',(-0.0118214745962156,-0.0354871077232055,
-0.0110006128129774));
#48434=CARTESIAN_POINT('Ctrl Pts',(-0.0125,-0.0355287743898722,-0.0110006128129774));
#48435=CARTESIAN_POINT('Ctrl Pts',(-0.0131785254037844,-0.0355704410565388,
-0.0110006128129774));
#48436=CARTESIAN_POINT('Ctrl Pts',(-0.0135177881056766,-0.0356121077232055,
-0.0115882330497678));
#48437=CARTESIAN_POINT('Ctrl Pts',(-0.0138570508075689,-0.0356537743898722,
-0.0121758532865583));
#48438=CARTESIAN_POINT('Ctrl Pts',(-0.0135177881056766,-0.0356954410565389,
-0.0127634735233487));
#48439=CARTESIAN_POINT('Ctrl Pts',(-0.0131785254037844,-0.0357371077232056,
-0.0133510937601391));
#48440=CARTESIAN_POINT('Ctrl Pts',(-0.0125,-0.0357787743898723,-0.0133510937601391));
#48441=CARTESIAN_POINT('Ctrl Pts',(-0.0118214745962156,-0.0358204410565389,
-0.0133510937601391));
#48442=CARTESIAN_POINT('Ctrl Pts',(-0.0114822118943233,-0.0358621077232055,
-0.0127634735233487));
#48443=CARTESIAN_POINT('Ctrl Pts',(-0.0111429491924311,-0.0359037743898722,
-0.0121758532865583));
#48444=CARTESIAN_POINT('Ctrl Pts',(-0.0114822118943233,-0.0359454410565389,
-0.0115882330497678));
#48445=CARTESIAN_POINT('Ctrl Pts',(-0.0118214745962156,-0.0359871077232055,
-0.0110006128129774));
#48446=CARTESIAN_POINT('Ctrl Pts',(-0.0125,-0.0360287743898721,-0.0110006128129774));
#48447=CARTESIAN_POINT('Ctrl Pts',(-0.0131785254037844,-0.0360704410565388,
-0.0110006128129774));
#48448=CARTESIAN_POINT('Ctrl Pts',(-0.0135177881056766,-0.0361121077232055,
-0.0115882330497678));
#48449=CARTESIAN_POINT('Ctrl Pts',(-0.0138570508075689,-0.0361537743898722,
-0.0121758532865582));
#48450=CARTESIAN_POINT('Ctrl Pts',(-0.0135177881056766,-0.0361954410565389,
-0.0127634735233486));
#48451=CARTESIAN_POINT('Ctrl Pts',(-0.0131785254037844,-0.0362371077232056,
-0.013351093760139));
#48452=CARTESIAN_POINT('Ctrl Pts',(-0.0125,-0.0362787743898722,-0.0133510937601391));
#48453=CARTESIAN_POINT('Ctrl Pts',(-0.0118214745962156,-0.0363204410565389,
-0.013351093760139));
#48454=CARTESIAN_POINT('Ctrl Pts',(-0.0114822118943233,-0.0363621077232055,
-0.0127634735233486));
#48455=CARTESIAN_POINT('Ctrl Pts',(-0.0111429491924311,-0.0364037743898722,
-0.0121758532865582));
#48456=CARTESIAN_POINT('Ctrl Pts',(-0.0114822118943233,-0.0364454410565389,
-0.0115882330497678));
#48457=CARTESIAN_POINT('Ctrl Pts',(-0.0118214745962156,-0.0364871077232055,
-0.0110006128129774));
#48458=CARTESIAN_POINT('Ctrl Pts',(-0.0125,-0.0365287743898721,-0.0110006128129774));
#48459=CARTESIAN_POINT('Ctrl Pts',(-0.0131785254037844,-0.0365704410565388,
-0.0110006128129774));
#48460=CARTESIAN_POINT('Ctrl Pts',(-0.0135177881056766,-0.0366121077232055,
-0.0115882330497678));
#48461=CARTESIAN_POINT('Ctrl Pts',(-0.0138570508075689,-0.0366537743898722,
-0.0121758532865582));
#48462=CARTESIAN_POINT('Ctrl Pts',(-0.0135177881056766,-0.0366954410565389,
-0.0127634735233486));
#48463=CARTESIAN_POINT('Ctrl Pts',(-0.0131785254037844,-0.0367371077232056,
-0.013351093760139));
#48464=CARTESIAN_POINT('Ctrl Pts',(-0.0125,-0.0367787743898722,-0.013351093760139));
#48465=CARTESIAN_POINT('Ctrl Pts',(-0.0118214745962156,-0.0368204410565389,
-0.013351093760139));
#48466=CARTESIAN_POINT('Ctrl Pts',(-0.0114822118943233,-0.0368621077232055,
-0.0127634735233486));
#48467=CARTESIAN_POINT('Ctrl Pts',(-0.0111429491924311,-0.0369037743898722,
-0.0121758532865582));
#48468=CARTESIAN_POINT('Ctrl Pts',(-0.0114822118943233,-0.0369454410565389,
-0.0115882330497678));
#48469=CARTESIAN_POINT('Ctrl Pts',(-0.0118214745962156,-0.0369871077232055,
-0.0110006128129774));
#48470=CARTESIAN_POINT('Ctrl Pts',(-0.0125,-0.0370287743898721,-0.0110006128129774));
#48471=CARTESIAN_POINT('Ctrl Pts',(-0.0131785254037844,-0.0370704410565389,
-0.0110006128129774));
#48472=CARTESIAN_POINT('Ctrl Pts',(-0.0135177881056766,-0.0371121077232055,
-0.0115882330497678));
#48473=CARTESIAN_POINT('Ctrl Pts',(-0.0138570508075689,-0.0371537743898722,
-0.0121758532865582));
#48474=CARTESIAN_POINT('Ctrl Pts',(-0.0135177881056766,-0.0371954410565389,
-0.0127634735233486));
#48475=CARTESIAN_POINT('Ctrl Pts',(-0.0131785254037844,-0.0372371077232056,
-0.013351093760139));
#48476=CARTESIAN_POINT('Ctrl Pts',(-0.0125,-0.0372787743898722,-0.013351093760139));
#48477=CARTESIAN_POINT('Ctrl Pts',(-0.0118214745962156,-0.0373204410565389,
-0.013351093760139));
#48478=CARTESIAN_POINT('Ctrl Pts',(-0.0114822118943233,-0.0373621077232055,
-0.0127634735233486));
#48479=CARTESIAN_POINT('Ctrl Pts',(-0.0111429491924311,-0.0374037743898722,
-0.0121758532865582));
#48480=CARTESIAN_POINT('Ctrl Pts',(-0.0114822118943233,-0.0374454410565389,
-0.0115882330497678));
#48481=CARTESIAN_POINT('Ctrl Pts',(-0.0118214745962156,-0.0374871077232055,
-0.0110006128129774));
#48482=CARTESIAN_POINT('Ctrl Pts',(-0.0125,-0.0375287743898721,-0.0110006128129774));
#48483=CARTESIAN_POINT('Ctrl Pts',(-0.0131785254037844,-0.0375704410565388,
-0.0110006128129773));
#48484=CARTESIAN_POINT('Ctrl Pts',(-0.0135177881056766,-0.0376121077232055,
-0.0115882330497678));
#48485=CARTESIAN_POINT('Ctrl Pts',(-0.0138570508075689,-0.0376537743898722,
-0.0121758532865582));
#48486=CARTESIAN_POINT('Ctrl Pts',(-0.0135177881056766,-0.0376954410565389,
-0.0127634735233486));
#48487=CARTESIAN_POINT('Ctrl Pts',(-0.0131785254037844,-0.0377371077232055,
-0.013351093760139));
#48488=CARTESIAN_POINT('Ctrl Pts',(-0.0125,-0.0377787743898722,-0.013351093760139));
#48489=CARTESIAN_POINT('Ctrl Pts',(-0.0118214745962156,-0.0378204410565389,
-0.013351093760139));
#48490=CARTESIAN_POINT('Ctrl Pts',(-0.0114822118943233,-0.0378621077232056,
-0.0127634735233486));
#48491=CARTESIAN_POINT('Ctrl Pts',(-0.0111429491924311,-0.0379037743898722,
-0.0121758532865582));
#48492=CARTESIAN_POINT('Ctrl Pts',(-0.0114822118943233,-0.0379454410565389,
-0.0115882330497678));
#48493=CARTESIAN_POINT('Ctrl Pts',(-0.0118214745962156,-0.0379871077232055,
-0.0110006128129773));
#48494=CARTESIAN_POINT('Ctrl Pts',(-0.0125,-0.0380287743898721,-0.0110006128129773));
#48495=CARTESIAN_POINT('Ctrl Pts',(-0.0131785254037844,-0.0380704410565388,
-0.0110006128129773));
#48496=CARTESIAN_POINT('Ctrl Pts',(-0.0135177881056766,-0.0381121077232055,
-0.0115882330497677));
#48497=CARTESIAN_POINT('Ctrl Pts',(-0.0138570508075689,-0.0381537743898722,
-0.0121758532865582));
#48498=CARTESIAN_POINT('Ctrl Pts',(-0.0135177881056766,-0.0381954410565388,
-0.0127634735233486));
#48499=CARTESIAN_POINT('Ctrl Pts',(-0.0131785254037844,-0.0382371077232056,
-0.013351093760139));
#48500=CARTESIAN_POINT('Ctrl Pts',(-0.0125,-0.0382787743898722,-0.013351093760139));
#48501=CARTESIAN_POINT('Ctrl Pts',(-0.0118214745962156,-0.0383204410565389,
-0.013351093760139));
#48502=CARTESIAN_POINT('Ctrl Pts',(-0.0114822118943233,-0.0383621077232056,
-0.0127634735233486));
#48503=CARTESIAN_POINT('Ctrl Pts',(-0.0111429491924311,-0.0384037743898722,
-0.0121758532865581));
#48504=CARTESIAN_POINT('Ctrl Pts',(-0.0114822118943233,-0.0384454410565388,
-0.0115882330497677));
#48505=CARTESIAN_POINT('Ctrl Pts',(-0.0118214745962156,-0.0384871077232055,
-0.0110006128129773));
#48506=CARTESIAN_POINT('Ctrl Pts',(-0.0125,-0.0385287743898722,-0.0110006128129773));
#48507=CARTESIAN_POINT('Ctrl Pts',(-0.0131785254037844,-0.0385704410565388,
-0.0110006128129773));
#48508=CARTESIAN_POINT('Ctrl Pts',(-0.0135177881056766,-0.0386121077232055,
-0.0115882330497677));
#48509=CARTESIAN_POINT('Ctrl Pts',(-0.0138570508075689,-0.0386537743898722,
-0.0121758532865581));
#48510=CARTESIAN_POINT('Ctrl Pts',(-0.0135177881056766,-0.0386954410565388,
-0.0127634735233486));
#48511=CARTESIAN_POINT('Ctrl Pts',(-0.0131785254037844,-0.0387371077232056,
-0.013351093760139));
#48512=CARTESIAN_POINT('Ctrl Pts',(-0.0125,-0.0387787743898722,-0.013351093760139));
#48513=CARTESIAN_POINT('Ctrl Pts',(-0.0118214745962156,-0.0388204410565389,
-0.013351093760139));
#48514=CARTESIAN_POINT('Ctrl Pts',(-0.0114822118943233,-0.0388621077232056,
-0.0127634735233486));
#48515=CARTESIAN_POINT('Ctrl Pts',(-0.0111429491924311,-0.0389037743898722,
-0.0121758532865581));
#48516=CARTESIAN_POINT('Ctrl Pts',(-0.0114822118943233,-0.0389454410565388,
-0.0115882330497677));
#48517=CARTESIAN_POINT('Ctrl Pts',(-0.0118214745962156,-0.0389871077232055,
-0.0110006128129773));
#48518=CARTESIAN_POINT('Ctrl Pts',(-0.0125,-0.0390287743898722,-0.0110006128129773));
#48519=CARTESIAN_POINT('Ctrl Pts',(-0.0131785254037844,-0.0390704410565388,
-0.0110006128129773));
#48520=CARTESIAN_POINT('Ctrl Pts',(-0.0135177881056766,-0.0391121077232055,
-0.0115882330497677));
#48521=CARTESIAN_POINT('Ctrl Pts',(-0.0138570508075689,-0.0391537743898722,
-0.0121758532865581));
#48522=CARTESIAN_POINT('Ctrl Pts',(-0.0135177881056766,-0.0391954410565388,
-0.0127634735233485));
#48523=CARTESIAN_POINT('Ctrl Pts',(-0.0131785254037844,-0.0392371077232056,
-0.013351093760139));
#48524=CARTESIAN_POINT('Ctrl Pts',(-0.0125,-0.0392787743898722,-0.013351093760139));
#48525=CARTESIAN_POINT('Ctrl Pts',(-0.0118214745962156,-0.0393204410565389,
-0.013351093760139));
#48526=CARTESIAN_POINT('Ctrl Pts',(-0.0114822118943233,-0.0393621077232056,
-0.0127634735233485));
#48527=CARTESIAN_POINT('Ctrl Pts',(-0.0111429491924311,-0.0394037743898722,
-0.0121758532865581));
#48528=CARTESIAN_POINT('Ctrl Pts',(-0.0114822118943233,-0.0394454410565388,
-0.0115882330497677));
#48529=CARTESIAN_POINT('Ctrl Pts',(-0.0118214745962156,-0.0394871077232055,
-0.0110006128129773));
#48530=CARTESIAN_POINT('Ctrl Pts',(-0.0125,-0.0395287743898722,-0.0110006128129773));
#48531=CARTESIAN_POINT('Ctrl Pts',(-0.0131785254037844,-0.0395704410565388,
-0.0110006128129773));
#48532=CARTESIAN_POINT('Ctrl Pts',(-0.0135177881056766,-0.0396121077232055,
-0.0115882330497677));
#48533=CARTESIAN_POINT('Ctrl Pts',(-0.0138570508075689,-0.0396537743898722,
-0.0121758532865581));
#48534=CARTESIAN_POINT('Ctrl Pts',(-0.0135177881056766,-0.0396954410565388,
-0.0127634735233485));
#48535=CARTESIAN_POINT('Ctrl Pts',(-0.0131785254037844,-0.0397371077232056,
-0.0133510937601389));
#48536=CARTESIAN_POINT('Ctrl Pts',(-0.0125,-0.0397787743898722,-0.0133510937601389));
#48537=CARTESIAN_POINT('Ctrl Pts',(-0.0118214745962156,-0.0398204410565389,
-0.0133510937601389));
#48538=CARTESIAN_POINT('Ctrl Pts',(-0.0114822118943233,-0.0398621077232056,
-0.0127634735233485));
#48539=CARTESIAN_POINT('Ctrl Pts',(-0.0111429491924311,-0.0399037743898722,
-0.0121758532865581));
#48540=CARTESIAN_POINT('Ctrl Pts',(-0.0114822118943233,-0.0399454410565388,
-0.0115882330497677));
#48541=CARTESIAN_POINT('Ctrl Pts',(-0.0118214745962156,-0.0399871077232055,
-0.0110006128129773));
#48542=CARTESIAN_POINT('Ctrl Pts',(-0.0125,-0.0400287743898722,-0.0110006128129773));
#48543=CARTESIAN_POINT('Ctrl Pts',(-0.0131785254037844,-0.0400704410565388,
-0.0110006128129773));
#48544=CARTESIAN_POINT('Ctrl Pts',(-0.0135177881056766,-0.0401121077232055,
-0.0115882330497677));
#48545=CARTESIAN_POINT('Ctrl Pts',(-0.0138570508075689,-0.0401537743898722,
-0.0121758532865581));
#48546=CARTESIAN_POINT('Ctrl Pts',(-0.0135177881056766,-0.0401954410565388,
-0.0127634735233485));
#48547=CARTESIAN_POINT('Ctrl Pts',(-0.0131785254037844,-0.0402371077232055,
-0.0133510937601389));
#48548=CARTESIAN_POINT('Ctrl Pts',(-0.0125,-0.0402787743898722,-0.0133510937601389));
#48549=CARTESIAN_POINT('Ctrl Pts',(-0.0118214745962156,-0.0403204410565389,
-0.0133510937601389));
#48550=CARTESIAN_POINT('Ctrl Pts',(-0.0114822118943233,-0.0403621077232055,
-0.0127634735233485));
#48551=CARTESIAN_POINT('Ctrl Pts',(-0.0111429491924311,-0.0404037743898722,
-0.0121758532865581));
#48552=CARTESIAN_POINT('Ctrl Pts',(-0.0114822118943233,-0.0404454410565388,
-0.0115882330497677));
#48553=CARTESIAN_POINT('Ctrl Pts',(-0.0118214745962156,-0.0404871077232055,
-0.0110006128129773));
#48554=CARTESIAN_POINT('Ctrl Pts',(-0.0125,-0.0405287743898722,-0.0110006128129772));
#48555=CARTESIAN_POINT('Ctrl Pts',(-0.0131785254037844,-0.0405704410565388,
-0.0110006128129773));
#48556=CARTESIAN_POINT('Ctrl Pts',(-0.0135177881056766,-0.0406121077232055,
-0.0115882330497677));
#48557=CARTESIAN_POINT('Ctrl Pts',(-0.0138570508075689,-0.0406537743898722,
-0.0121758532865581));
#48558=CARTESIAN_POINT('Ctrl Pts',(-0.0135177881056766,-0.0406954410565388,
-0.0127634735233485));
#48559=CARTESIAN_POINT('Ctrl Pts',(-0.0131785254037844,-0.0407371077232055,
-0.0133510937601389));
#48560=CARTESIAN_POINT('Ctrl Pts',(-0.0125,-0.0407787743898722,-0.0133510937601389));
#48561=CARTESIAN_POINT('Ctrl Pts',(-0.0118214745962156,-0.0408204410565389,
-0.0133510937601389));
#48562=CARTESIAN_POINT('Ctrl Pts',(-0.0114822118943233,-0.0408621077232055,
-0.0127634735233485));
#48563=CARTESIAN_POINT('Ctrl Pts',(-0.0111429491924311,-0.0409037743898722,
-0.0121758532865581));
#48564=CARTESIAN_POINT('Ctrl Pts',(-0.0114822118943233,-0.0409454410565388,
-0.0115882330497676));
#48565=CARTESIAN_POINT('Ctrl Pts',(-0.0118214745962156,-0.0409871077232055,
-0.0110006128129772));
#48566=CARTESIAN_POINT('Ctrl Pts',(-0.0125,-0.0410287743898722,-0.0110006128129772));
#48567=CARTESIAN_POINT('Ctrl Pts',(-0.0131785254037844,-0.0410704410565388,
-0.0110006128129772));
#48568=CARTESIAN_POINT('Ctrl Pts',(-0.0135177881056766,-0.0411121077232055,
-0.0115882330497676));
#48569=CARTESIAN_POINT('Ctrl Pts',(-0.0138570508075689,-0.0411537743898722,
-0.012175853286558));
#48570=CARTESIAN_POINT('Ctrl Pts',(-0.0135177881056766,-0.0411954410565388,
-0.0127634735233485));
#48571=CARTESIAN_POINT('Ctrl Pts',(-0.0131785254037844,-0.0412371077232056,
-0.0133510937601389));
#48572=CARTESIAN_POINT('Ctrl Pts',(-0.0125,-0.0412787743898722,-0.0133510937601389));
#48573=CARTESIAN_POINT('Ctrl Pts',(-0.0118214745962156,-0.0413204410565389,
-0.0133510937601389));
#48574=CARTESIAN_POINT('Ctrl Pts',(-0.0114822118943233,-0.0413621077232055,
-0.0127634735233485));
#48575=CARTESIAN_POINT('Ctrl Pts',(-0.0111429491924311,-0.0414037743898722,
-0.012175853286558));
#48576=CARTESIAN_POINT('Ctrl Pts',(-0.0114822118943233,-0.0414454410565388,
-0.0115882330497676));
#48577=CARTESIAN_POINT('Ctrl Pts',(-0.0117636651570184,-0.0414800078368349,
-0.0111007416988237));
#48578=CARTESIAN_POINT('Ctrl Pts',(-0.0123199245616647,-0.0415172243523708,
-0.0110144907216151));
#48579=CARTESIAN_POINT('Ctrl Pts',(-0.012484606188608,-0.033092009537925,
-0.0136757875882698));
#48580=CARTESIAN_POINT('Ctrl Pts',(-0.0116288506733376,-0.0331334256887305,
-0.0136670049776016));
#48581=CARTESIAN_POINT('Ctrl Pts',(-0.0112009503823333,-0.0331746000485455,
-0.0129258599330088));
#48582=CARTESIAN_POINT('Ctrl Pts',(-0.0107679338431112,-0.0332162667152122,
-0.0121758532865583));
#48583=CARTESIAN_POINT('Ctrl Pts',(-0.0112009503823333,-0.0332579333818788,
-0.0114258466401078));
#48584=CARTESIAN_POINT('Ctrl Pts',(-0.0116339669215556,-0.0332996000485455,
-0.0106758399936573));
#48585=CARTESIAN_POINT('Ctrl Pts',(-0.0125,-0.0333412667152122,-0.0106758399936573));
#48586=CARTESIAN_POINT('Ctrl Pts',(-0.0133660330784445,-0.0333829333818788,
-0.0106758399936573));
#48587=CARTESIAN_POINT('Ctrl Pts',(-0.0137990496176667,-0.0334246000485455,
-0.0114258466401078));
#48588=CARTESIAN_POINT('Ctrl Pts',(-0.0142320661568888,-0.0334662667152122,
-0.0121758532865583));
#48589=CARTESIAN_POINT('Ctrl Pts',(-0.0137990496176667,-0.0335079333818789,
-0.0129258599330088));
#48590=CARTESIAN_POINT('Ctrl Pts',(-0.0133660330784445,-0.0335496000485456,
-0.0136758665794593));
#48591=CARTESIAN_POINT('Ctrl Pts',(-0.0125,-0.0335912667152122,-0.0136758665794593));
#48592=CARTESIAN_POINT('Ctrl Pts',(-0.0116339669215556,-0.0336329333818789,
-0.0136758665794593));
#48593=CARTESIAN_POINT('Ctrl Pts',(-0.0112009503823333,-0.0336746000485455,
-0.0129258599330088));
#48594=CARTESIAN_POINT('Ctrl Pts',(-0.0107679338431112,-0.0337162667152122,
-0.0121758532865583));
#48595=CARTESIAN_POINT('Ctrl Pts',(-0.0112009503823333,-0.0337579333818788,
-0.0114258466401078));
#48596=CARTESIAN_POINT('Ctrl Pts',(-0.0116339669215556,-0.0337996000485455,
-0.0106758399936573));
#48597=CARTESIAN_POINT('Ctrl Pts',(-0.0125,-0.0338412667152122,-0.0106758399936573));
#48598=CARTESIAN_POINT('Ctrl Pts',(-0.0133660330784445,-0.0338829333818788,
-0.0106758399936573));
#48599=CARTESIAN_POINT('Ctrl Pts',(-0.0137990496176667,-0.0339246000485455,
-0.0114258466401078));
#48600=CARTESIAN_POINT('Ctrl Pts',(-0.0142320661568888,-0.0339662667152122,
-0.0121758532865583));
#48601=CARTESIAN_POINT('Ctrl Pts',(-0.0137990496176667,-0.0340079333818789,
-0.0129258599330088));
#48602=CARTESIAN_POINT('Ctrl Pts',(-0.0133660330784445,-0.0340496000485456,
-0.0136758665794593));
#48603=CARTESIAN_POINT('Ctrl Pts',(-0.0125,-0.0340912667152123,-0.0136758665794593));
#48604=CARTESIAN_POINT('Ctrl Pts',(-0.0116339669215556,-0.0341329333818789,
-0.0136758665794593));
#48605=CARTESIAN_POINT('Ctrl Pts',(-0.0112009503823333,-0.0341746000485455,
-0.0129258599330088));
#48606=CARTESIAN_POINT('Ctrl Pts',(-0.0107679338431112,-0.0342162667152122,
-0.0121758532865583));
#48607=CARTESIAN_POINT('Ctrl Pts',(-0.0112009503823333,-0.0342579333818789,
-0.0114258466401078));
#48608=CARTESIAN_POINT('Ctrl Pts',(-0.0116339669215556,-0.0342996000485455,
-0.0106758399936573));
#48609=CARTESIAN_POINT('Ctrl Pts',(-0.0125,-0.0343412667152122,-0.0106758399936573));
#48610=CARTESIAN_POINT('Ctrl Pts',(-0.0133660330784445,-0.0343829333818788,
-0.0106758399936573));
#48611=CARTESIAN_POINT('Ctrl Pts',(-0.0137990496176667,-0.0344246000485455,
-0.0114258466401078));
#48612=CARTESIAN_POINT('Ctrl Pts',(-0.0142320661568888,-0.0344662667152122,
-0.0121758532865583));
#48613=CARTESIAN_POINT('Ctrl Pts',(-0.0137990496176667,-0.0345079333818789,
-0.0129258599330088));
#48614=CARTESIAN_POINT('Ctrl Pts',(-0.0133660330784445,-0.0345496000485456,
-0.0136758665794593));
#48615=CARTESIAN_POINT('Ctrl Pts',(-0.0125,-0.0345912667152123,-0.0136758665794593));
#48616=CARTESIAN_POINT('Ctrl Pts',(-0.0116339669215556,-0.0346329333818789,
-0.0136758665794593));
#48617=CARTESIAN_POINT('Ctrl Pts',(-0.0112009503823333,-0.0346746000485455,
-0.0129258599330088));
#48618=CARTESIAN_POINT('Ctrl Pts',(-0.0107679338431112,-0.0347162667152122,
-0.0121758532865583));
#48619=CARTESIAN_POINT('Ctrl Pts',(-0.0112009503823333,-0.0347579333818789,
-0.0114258466401078));
#48620=CARTESIAN_POINT('Ctrl Pts',(-0.0116339669215556,-0.0347996000485455,
-0.0106758399936573));
#48621=CARTESIAN_POINT('Ctrl Pts',(-0.0125,-0.0348412667152122,-0.0106758399936573));
#48622=CARTESIAN_POINT('Ctrl Pts',(-0.0133660330784445,-0.0348829333818788,
-0.0106758399936573));
#48623=CARTESIAN_POINT('Ctrl Pts',(-0.0137990496176667,-0.0349246000485455,
-0.0114258466401078));
#48624=CARTESIAN_POINT('Ctrl Pts',(-0.0142320661568888,-0.0349662667152122,
-0.0121758532865583));
#48625=CARTESIAN_POINT('Ctrl Pts',(-0.0137990496176667,-0.0350079333818789,
-0.0129258599330088));
#48626=CARTESIAN_POINT('Ctrl Pts',(-0.0133660330784445,-0.0350496000485456,
-0.0136758665794593));
#48627=CARTESIAN_POINT('Ctrl Pts',(-0.0125,-0.0350912667152123,-0.0136758665794593));
#48628=CARTESIAN_POINT('Ctrl Pts',(-0.0116339669215556,-0.0351329333818789,
-0.0136758665794593));
#48629=CARTESIAN_POINT('Ctrl Pts',(-0.0112009503823333,-0.0351746000485455,
-0.0129258599330088));
#48630=CARTESIAN_POINT('Ctrl Pts',(-0.0107679338431112,-0.0352162667152122,
-0.0121758532865583));
#48631=CARTESIAN_POINT('Ctrl Pts',(-0.0112009503823333,-0.0352579333818789,
-0.0114258466401078));
#48632=CARTESIAN_POINT('Ctrl Pts',(-0.0116339669215556,-0.0352996000485455,
-0.0106758399936573));
#48633=CARTESIAN_POINT('Ctrl Pts',(-0.0125,-0.0353412667152122,-0.0106758399936573));
#48634=CARTESIAN_POINT('Ctrl Pts',(-0.0133660330784445,-0.0353829333818788,
-0.0106758399936573));
#48635=CARTESIAN_POINT('Ctrl Pts',(-0.0137990496176667,-0.0354246000485455,
-0.0114258466401078));
#48636=CARTESIAN_POINT('Ctrl Pts',(-0.0142320661568888,-0.0354662667152122,
-0.0121758532865583));
#48637=CARTESIAN_POINT('Ctrl Pts',(-0.0137990496176667,-0.0355079333818789,
-0.0129258599330088));
#48638=CARTESIAN_POINT('Ctrl Pts',(-0.0133660330784445,-0.0355496000485456,
-0.0136758665794593));
#48639=CARTESIAN_POINT('Ctrl Pts',(-0.0125,-0.0355912667152123,-0.0136758665794592));
#48640=CARTESIAN_POINT('Ctrl Pts',(-0.0116339669215556,-0.0356329333818789,
-0.0136758665794593));
#48641=CARTESIAN_POINT('Ctrl Pts',(-0.0112009503823333,-0.0356746000485455,
-0.0129258599330087));
#48642=CARTESIAN_POINT('Ctrl Pts',(-0.0107679338431112,-0.0357162667152122,
-0.0121758532865583));
#48643=CARTESIAN_POINT('Ctrl Pts',(-0.0112009503823333,-0.0357579333818789,
-0.0114258466401077));
#48644=CARTESIAN_POINT('Ctrl Pts',(-0.0116339669215556,-0.0357996000485455,
-0.0106758399936572));
#48645=CARTESIAN_POINT('Ctrl Pts',(-0.0125,-0.0358412667152122,-0.0106758399936572));
#48646=CARTESIAN_POINT('Ctrl Pts',(-0.0133660330784445,-0.0358829333818788,
-0.0106758399936572));
#48647=CARTESIAN_POINT('Ctrl Pts',(-0.0137990496176667,-0.0359246000485455,
-0.0114258466401077));
#48648=CARTESIAN_POINT('Ctrl Pts',(-0.0142320661568888,-0.0359662667152122,
-0.0121758532865582));
#48649=CARTESIAN_POINT('Ctrl Pts',(-0.0137990496176667,-0.0360079333818789,
-0.0129258599330087));
#48650=CARTESIAN_POINT('Ctrl Pts',(-0.0133660330784445,-0.0360496000485456,
-0.0136758665794592));
#48651=CARTESIAN_POINT('Ctrl Pts',(-0.0125,-0.0360912667152122,-0.0136758665794592));
#48652=CARTESIAN_POINT('Ctrl Pts',(-0.0116339669215556,-0.0361329333818789,
-0.0136758665794592));
#48653=CARTESIAN_POINT('Ctrl Pts',(-0.0112009503823333,-0.0361746000485455,
-0.0129258599330087));
#48654=CARTESIAN_POINT('Ctrl Pts',(-0.0107679338431112,-0.0362162667152122,
-0.0121758532865582));
#48655=CARTESIAN_POINT('Ctrl Pts',(-0.0112009503823333,-0.0362579333818789,
-0.0114258466401077));
#48656=CARTESIAN_POINT('Ctrl Pts',(-0.0116339669215556,-0.0362996000485455,
-0.0106758399936572));
#48657=CARTESIAN_POINT('Ctrl Pts',(-0.0125,-0.0363412667152121,-0.0106758399936572));
#48658=CARTESIAN_POINT('Ctrl Pts',(-0.0133660330784445,-0.0363829333818788,
-0.0106758399936572));
#48659=CARTESIAN_POINT('Ctrl Pts',(-0.0137990496176667,-0.0364246000485455,
-0.0114258466401077));
#48660=CARTESIAN_POINT('Ctrl Pts',(-0.0142320661568888,-0.0364662667152122,
-0.0121758532865582));
#48661=CARTESIAN_POINT('Ctrl Pts',(-0.0137990496176667,-0.0365079333818789,
-0.0129258599330087));
#48662=CARTESIAN_POINT('Ctrl Pts',(-0.0133660330784445,-0.0365496000485456,
-0.0136758665794592));
#48663=CARTESIAN_POINT('Ctrl Pts',(-0.0125,-0.0365912667152122,-0.0136758665794592));
#48664=CARTESIAN_POINT('Ctrl Pts',(-0.0116339669215556,-0.0366329333818789,
-0.0136758665794592));
#48665=CARTESIAN_POINT('Ctrl Pts',(-0.0112009503823333,-0.0366746000485455,
-0.0129258599330087));
#48666=CARTESIAN_POINT('Ctrl Pts',(-0.0107679338431112,-0.0367162667152122,
-0.0121758532865582));
#48667=CARTESIAN_POINT('Ctrl Pts',(-0.0112009503823333,-0.0367579333818789,
-0.0114258466401077));
#48668=CARTESIAN_POINT('Ctrl Pts',(-0.0116339669215556,-0.0367996000485454,
-0.0106758399936572));
#48669=CARTESIAN_POINT('Ctrl Pts',(-0.0125,-0.0368412667152121,-0.0106758399936572));
#48670=CARTESIAN_POINT('Ctrl Pts',(-0.0133660330784445,-0.0368829333818788,
-0.0106758399936572));
#48671=CARTESIAN_POINT('Ctrl Pts',(-0.0137990496176667,-0.0369246000485455,
-0.0114258466401077));
#48672=CARTESIAN_POINT('Ctrl Pts',(-0.0142320661568888,-0.0369662667152122,
-0.0121758532865582));
#48673=CARTESIAN_POINT('Ctrl Pts',(-0.0137990496176667,-0.0370079333818789,
-0.0129258599330087));
#48674=CARTESIAN_POINT('Ctrl Pts',(-0.0133660330784445,-0.0370496000485455,
-0.0136758665794592));
#48675=CARTESIAN_POINT('Ctrl Pts',(-0.0125,-0.0370912667152122,-0.0136758665794592));
#48676=CARTESIAN_POINT('Ctrl Pts',(-0.0116339669215556,-0.0371329333818789,
-0.0136758665794592));
#48677=CARTESIAN_POINT('Ctrl Pts',(-0.0112009503823333,-0.0371746000485455,
-0.0129258599330087));
#48678=CARTESIAN_POINT('Ctrl Pts',(-0.0107679338431112,-0.0372162667152122,
-0.0121758532865582));
#48679=CARTESIAN_POINT('Ctrl Pts',(-0.0112009503823333,-0.0372579333818789,
-0.0114258466401077));
#48680=CARTESIAN_POINT('Ctrl Pts',(-0.0116339669215556,-0.0372996000485455,
-0.0106758399936572));
#48681=CARTESIAN_POINT('Ctrl Pts',(-0.0125,-0.0373412667152121,-0.0106758399936572));
#48682=CARTESIAN_POINT('Ctrl Pts',(-0.0133660330784445,-0.0373829333818788,
-0.0106758399936572));
#48683=CARTESIAN_POINT('Ctrl Pts',(-0.0137990496176667,-0.0374246000485455,
-0.0114258466401077));
#48684=CARTESIAN_POINT('Ctrl Pts',(-0.0142320661568888,-0.0374662667152122,
-0.0121758532865582));
#48685=CARTESIAN_POINT('Ctrl Pts',(-0.0137990496176667,-0.0375079333818789,
-0.0129258599330087));
#48686=CARTESIAN_POINT('Ctrl Pts',(-0.0133660330784445,-0.0375496000485456,
-0.0136758665794592));
#48687=CARTESIAN_POINT('Ctrl Pts',(-0.0125,-0.0375912667152122,-0.0136758665794592));
#48688=CARTESIAN_POINT('Ctrl Pts',(-0.0116339669215556,-0.0376329333818789,
-0.0136758665794592));
#48689=CARTESIAN_POINT('Ctrl Pts',(-0.0112009503823333,-0.0376746000485455,
-0.0129258599330087));
#48690=CARTESIAN_POINT('Ctrl Pts',(-0.0107679338431112,-0.0377162667152122,
-0.0121758532865582));
#48691=CARTESIAN_POINT('Ctrl Pts',(-0.0112009503823333,-0.0377579333818789,
-0.0114258466401077));
#48692=CARTESIAN_POINT('Ctrl Pts',(-0.0116339669215556,-0.0377996000485455,
-0.0106758399936572));
#48693=CARTESIAN_POINT('Ctrl Pts',(-0.0125,-0.0378412667152121,-0.0106758399936572));
#48694=CARTESIAN_POINT('Ctrl Pts',(-0.0133660330784445,-0.0378829333818788,
-0.0106758399936572));
#48695=CARTESIAN_POINT('Ctrl Pts',(-0.0137990496176667,-0.0379246000485455,
-0.0114258466401077));
#48696=CARTESIAN_POINT('Ctrl Pts',(-0.0142320661568888,-0.0379662667152122,
-0.0121758532865582));
#48697=CARTESIAN_POINT('Ctrl Pts',(-0.0137990496176667,-0.0380079333818789,
-0.0129258599330087));
#48698=CARTESIAN_POINT('Ctrl Pts',(-0.0133660330784445,-0.0380496000485456,
-0.0136758665794592));
#48699=CARTESIAN_POINT('Ctrl Pts',(-0.0125,-0.0380912667152122,-0.0136758665794592));
#48700=CARTESIAN_POINT('Ctrl Pts',(-0.0116339669215556,-0.0381329333818789,
-0.0136758665794592));
#48701=CARTESIAN_POINT('Ctrl Pts',(-0.0112009503823333,-0.0381746000485456,
-0.0129258599330087));
#48702=CARTESIAN_POINT('Ctrl Pts',(-0.0107679338431112,-0.0382162667152122,
-0.0121758532865582));
#48703=CARTESIAN_POINT('Ctrl Pts',(-0.0112009503823333,-0.0382579333818788,
-0.0114258466401077));
#48704=CARTESIAN_POINT('Ctrl Pts',(-0.0116339669215556,-0.0382996000485455,
-0.0106758399936572));
#48705=CARTESIAN_POINT('Ctrl Pts',(-0.0125,-0.0383412667152122,-0.0106758399936572));
#48706=CARTESIAN_POINT('Ctrl Pts',(-0.0133660330784445,-0.0383829333818788,
-0.0106758399936572));
#48707=CARTESIAN_POINT('Ctrl Pts',(-0.0137990496176667,-0.0384246000485455,
-0.0114258466401076));
#48708=CARTESIAN_POINT('Ctrl Pts',(-0.0142320661568888,-0.0384662667152122,
-0.0121758532865581));
#48709=CARTESIAN_POINT('Ctrl Pts',(-0.0137990496176667,-0.0385079333818789,
-0.0129258599330086));
#48710=CARTESIAN_POINT('Ctrl Pts',(-0.0133660330784445,-0.0385496000485456,
-0.0136758665794591));
#48711=CARTESIAN_POINT('Ctrl Pts',(-0.0125,-0.0385912667152122,-0.0136758665794591));
#48712=CARTESIAN_POINT('Ctrl Pts',(-0.0116339669215556,-0.0386329333818789,
-0.0136758665794591));
#48713=CARTESIAN_POINT('Ctrl Pts',(-0.0112009503823333,-0.0386746000485456,
-0.0129258599330086));
#48714=CARTESIAN_POINT('Ctrl Pts',(-0.0107679338431112,-0.0387162667152122,
-0.0121758532865581));
#48715=CARTESIAN_POINT('Ctrl Pts',(-0.0112009503823333,-0.0387579333818788,
-0.0114258466401076));
#48716=CARTESIAN_POINT('Ctrl Pts',(-0.0116339669215556,-0.0387996000485455,
-0.0106758399936571));
#48717=CARTESIAN_POINT('Ctrl Pts',(-0.0125,-0.0388412667152122,-0.0106758399936571));
#48718=CARTESIAN_POINT('Ctrl Pts',(-0.0133660330784445,-0.0388829333818788,
-0.0106758399936571));
#48719=CARTESIAN_POINT('Ctrl Pts',(-0.0137990496176667,-0.0389246000485455,
-0.0114258466401076));
#48720=CARTESIAN_POINT('Ctrl Pts',(-0.0142320661568888,-0.0389662667152122,
-0.0121758532865581));
#48721=CARTESIAN_POINT('Ctrl Pts',(-0.0137990496176667,-0.0390079333818789,
-0.0129258599330086));
#48722=CARTESIAN_POINT('Ctrl Pts',(-0.0133660330784445,-0.0390496000485456,
-0.0136758665794591));
#48723=CARTESIAN_POINT('Ctrl Pts',(-0.0125,-0.0390912667152122,-0.0136758665794591));
#48724=CARTESIAN_POINT('Ctrl Pts',(-0.0116339669215556,-0.0391329333818789,
-0.0136758665794591));
#48725=CARTESIAN_POINT('Ctrl Pts',(-0.0112009503823333,-0.0391746000485456,
-0.0129258599330086));
#48726=CARTESIAN_POINT('Ctrl Pts',(-0.0107679338431112,-0.0392162667152122,
-0.0121758532865581));
#48727=CARTESIAN_POINT('Ctrl Pts',(-0.0112009503823333,-0.0392579333818788,
-0.0114258466401076));
#48728=CARTESIAN_POINT('Ctrl Pts',(-0.0116339669215556,-0.0392996000485454,
-0.0106758399936571));
#48729=CARTESIAN_POINT('Ctrl Pts',(-0.0125,-0.0393412667152122,-0.0106758399936571));
#48730=CARTESIAN_POINT('Ctrl Pts',(-0.0133660330784445,-0.0393829333818788,
-0.0106758399936571));
#48731=CARTESIAN_POINT('Ctrl Pts',(-0.0137990496176667,-0.0394246000485455,
-0.0114258466401076));
#48732=CARTESIAN_POINT('Ctrl Pts',(-0.0142320661568888,-0.0394662667152122,
-0.0121758532865581));
#48733=CARTESIAN_POINT('Ctrl Pts',(-0.0137990496176667,-0.0395079333818789,
-0.0129258599330086));
#48734=CARTESIAN_POINT('Ctrl Pts',(-0.0133660330784445,-0.0395496000485456,
-0.0136758665794591));
#48735=CARTESIAN_POINT('Ctrl Pts',(-0.0125,-0.0395912667152122,-0.0136758665794591));
#48736=CARTESIAN_POINT('Ctrl Pts',(-0.0116339669215556,-0.0396329333818789,
-0.0136758665794591));
#48737=CARTESIAN_POINT('Ctrl Pts',(-0.0112009503823333,-0.0396746000485456,
-0.0129258599330086));
#48738=CARTESIAN_POINT('Ctrl Pts',(-0.0107679338431112,-0.0397162667152122,
-0.0121758532865581));
#48739=CARTESIAN_POINT('Ctrl Pts',(-0.0112009503823333,-0.0397579333818788,
-0.0114258466401076));
#48740=CARTESIAN_POINT('Ctrl Pts',(-0.0116339669215556,-0.0397996000485455,
-0.0106758399936571));
#48741=CARTESIAN_POINT('Ctrl Pts',(-0.0125,-0.0398412667152122,-0.0106758399936571));
#48742=CARTESIAN_POINT('Ctrl Pts',(-0.0133660330784445,-0.0398829333818788,
-0.0106758399936571));
#48743=CARTESIAN_POINT('Ctrl Pts',(-0.0137990496176667,-0.0399246000485455,
-0.0114258466401076));
#48744=CARTESIAN_POINT('Ctrl Pts',(-0.0142320661568888,-0.0399662667152122,
-0.0121758532865581));
#48745=CARTESIAN_POINT('Ctrl Pts',(-0.0137990496176667,-0.0400079333818789,
-0.0129258599330086));
#48746=CARTESIAN_POINT('Ctrl Pts',(-0.0133660330784445,-0.0400496000485456,
-0.0136758665794591));
#48747=CARTESIAN_POINT('Ctrl Pts',(-0.0125,-0.0400912667152122,-0.0136758665794591));
#48748=CARTESIAN_POINT('Ctrl Pts',(-0.0116339669215556,-0.0401329333818789,
-0.0136758665794591));
#48749=CARTESIAN_POINT('Ctrl Pts',(-0.0112009503823333,-0.0401746000485455,
-0.0129258599330086));
#48750=CARTESIAN_POINT('Ctrl Pts',(-0.0107679338431112,-0.0402162667152122,
-0.0121758532865581));
#48751=CARTESIAN_POINT('Ctrl Pts',(-0.0112009503823333,-0.0402579333818788,
-0.0114258466401076));
#48752=CARTESIAN_POINT('Ctrl Pts',(-0.0116339669215556,-0.0402996000485455,
-0.0106758399936571));
#48753=CARTESIAN_POINT('Ctrl Pts',(-0.0125,-0.0403412667152122,-0.0106758399936571));
#48754=CARTESIAN_POINT('Ctrl Pts',(-0.0133660330784445,-0.0403829333818788,
-0.0106758399936571));
#48755=CARTESIAN_POINT('Ctrl Pts',(-0.0137990496176667,-0.0404246000485455,
-0.0114258466401076));
#48756=CARTESIAN_POINT('Ctrl Pts',(-0.0142320661568888,-0.0404662667152122,
-0.0121758532865581));
#48757=CARTESIAN_POINT('Ctrl Pts',(-0.0137990496176667,-0.0405079333818789,
-0.0129258599330086));
#48758=CARTESIAN_POINT('Ctrl Pts',(-0.0133660330784445,-0.0405496000485456,
-0.0136758665794591));
#48759=CARTESIAN_POINT('Ctrl Pts',(-0.0125,-0.0405912667152122,-0.0136758665794591));
#48760=CARTESIAN_POINT('Ctrl Pts',(-0.0116339669215556,-0.0406329333818789,
-0.0136758665794591));
#48761=CARTESIAN_POINT('Ctrl Pts',(-0.0112009503823333,-0.0406746000485455,
-0.0129258599330086));
#48762=CARTESIAN_POINT('Ctrl Pts',(-0.0107679338431112,-0.0407162667152122,
-0.0121758532865581));
#48763=CARTESIAN_POINT('Ctrl Pts',(-0.0112009503823333,-0.0407579333818788,
-0.0114258466401076));
#48764=CARTESIAN_POINT('Ctrl Pts',(-0.0116339669215556,-0.0407996000485454,
-0.0106758399936571));
#48765=CARTESIAN_POINT('Ctrl Pts',(-0.0125,-0.0408412667152122,-0.0106758399936571));
#48766=CARTESIAN_POINT('Ctrl Pts',(-0.0133660330784445,-0.0408829333818788,
-0.0106758399936571));
#48767=CARTESIAN_POINT('Ctrl Pts',(-0.0137990496176667,-0.0409246000485455,
-0.0114258466401076));
#48768=CARTESIAN_POINT('Ctrl Pts',(-0.0142320661568888,-0.0409662667152122,
-0.0121758532865581));
#48769=CARTESIAN_POINT('Ctrl Pts',(-0.0137990496176667,-0.0410079333818789,
-0.0129258599330086));
#48770=CARTESIAN_POINT('Ctrl Pts',(-0.0133660330784445,-0.0410496000485455,
-0.0136758665794591));
#48771=CARTESIAN_POINT('Ctrl Pts',(-0.0125,-0.0410912667152122,-0.0136758665794591));
#48772=CARTESIAN_POINT('Ctrl Pts',(-0.0116339669215556,-0.0411329333818789,
-0.0136758665794591));
#48773=CARTESIAN_POINT('Ctrl Pts',(-0.0112009503823333,-0.0411746000485455,
-0.0129258599330086));
#48774=CARTESIAN_POINT('Ctrl Pts',(-0.0107679338431112,-0.0412162667152122,
-0.012175853286558));
#48775=CARTESIAN_POINT('Ctrl Pts',(-0.0112009503823333,-0.0412579333818788,
-0.0114258466401076));
#48776=CARTESIAN_POINT('Ctrl Pts',(-0.011560182084154,-0.0412925001621749,
-0.0108036390808646));
#48777=CARTESIAN_POINT('Ctrl Pts',(-0.0122701614628665,-0.0413297166777108,
-0.0106935530046557));
#48778=CARTESIAN_POINT('Ctrl Pts',(-0.0124999999999993,-0.0412787743898722,
-0.0133510937601389));
#48779=CARTESIAN_POINT('Ctrl Pts',(-0.012358363960416,-0.0412787743898722,
-0.0133661583408318));
#48780=CARTESIAN_POINT('Ctrl Pts',(-0.0122152415795414,-0.0412787743898722,
-0.0133567697507035));
#48781=CARTESIAN_POINT('Ctrl Pts',(-0.0119414505804856,-0.0412787743898722,
-0.013290480504866));
#48782=CARTESIAN_POINT('Ctrl Pts',(-0.0118126101483348,-0.0412787743898715,
-0.0132351257070212));
#48783=CARTESIAN_POINT('Ctrl Pts',(-0.011583418002351,-0.0412787743898715,
-0.0130869866720988));
#48784=CARTESIAN_POINT('Ctrl Pts',(-0.0114581988285637,-0.0412787743898735,
-0.0129841339295786));
#48785=CARTESIAN_POINT('Ctrl Pts',(-0.0112456182130333,-0.0412787743898735,
-0.0126725262993937));
#48786=CARTESIAN_POINT('Ctrl Pts',(-0.0111762705577612,-0.0412787743898722,
-0.0125149575896434));
#48787=CARTESIAN_POINT('Ctrl Pts',(-0.0110953627121927,-0.0412787743898722,
-0.0121694782739801));
#48788=CARTESIAN_POINT('Ctrl Pts',(-0.0110895688642527,-0.0412787743898722,
-0.0119837162050846));
#48789=CARTESIAN_POINT('Ctrl Pts',(-0.0111490989927533,-0.0412787743898722,
-0.0116312177889278));
#48790=CARTESIAN_POINT('Ctrl Pts',(-0.0112035576011838,-0.0412787743898722,
-0.0115039539015553));
#48791=CARTESIAN_POINT('Ctrl Pts',(-0.0112928253083772,-0.0412787743898722,
-0.0113166320658545));
#48792=CARTESIAN_POINT('Ctrl Pts',(-0.0113643003226613,-0.0412787743898722,
-0.0112058612590309));
#48793=CARTESIAN_POINT('Ctrl Pts',(-0.0114490560961843,-0.0412787743898722,
-0.011105565049194));
#48794=CARTESIAN_POINT('Ctrl Pts',(-0.0135456685377107,-0.033466680519734,
-0.0132513163635058));
#48795=CARTESIAN_POINT('Ctrl Pts',(-0.0131090202398857,-0.0334994815488067,
-0.0136758677933666));
#48796=CARTESIAN_POINT('Ctrl Pts',(-0.0125,-0.0335287827653819,-0.0136758677933666));
#48797=CARTESIAN_POINT('Ctrl Pts',(-0.0116339662207059,-0.0335704494320486,
-0.0136758677933666));
#48798=CARTESIAN_POINT('Ctrl Pts',(-0.0112009493310588,-0.0336121160987153,
-0.0129258605399625));
#48799=CARTESIAN_POINT('Ctrl Pts',(-0.0107679324414118,-0.0336537827653819,
-0.0121758532865583));
#48800=CARTESIAN_POINT('Ctrl Pts',(-0.0112009493310588,-0.0336954494320485,
-0.0114258460331541));
#48801=CARTESIAN_POINT('Ctrl Pts',(-0.0116339662207059,-0.0337371160987151,
-0.01067583877975));
#48802=CARTESIAN_POINT('Ctrl Pts',(-0.0125,-0.0337787827653818,-0.01067583877975));
#48803=CARTESIAN_POINT('Ctrl Pts',(-0.0133660337792941,-0.0338204494320485,
-0.01067583877975));
#48804=CARTESIAN_POINT('Ctrl Pts',(-0.0137990506689412,-0.0338621160987152,
-0.0114258460331541));
#48805=CARTESIAN_POINT('Ctrl Pts',(-0.0142320675585882,-0.0339037827653818,
-0.0121758532865583));
#48806=CARTESIAN_POINT('Ctrl Pts',(-0.0137990506689412,-0.0339454494320486,
-0.0129258605399625));
#48807=CARTESIAN_POINT('Ctrl Pts',(-0.0133660337792941,-0.0339871160987152,
-0.0136758677933666));
#48808=CARTESIAN_POINT('Ctrl Pts',(-0.0125,-0.0340287827653819,-0.0136758677933666));
#48809=CARTESIAN_POINT('Ctrl Pts',(-0.0116339662207059,-0.0340704494320486,
-0.0136758677933666));
#48810=CARTESIAN_POINT('Ctrl Pts',(-0.0112009493310588,-0.0341121160987153,
-0.0129258605399625));
#48811=CARTESIAN_POINT('Ctrl Pts',(-0.0107679324414118,-0.0341537827653819,
-0.0121758532865583));
#48812=CARTESIAN_POINT('Ctrl Pts',(-0.0112009493310588,-0.0341954494320485,
-0.0114258460331541));
#48813=CARTESIAN_POINT('Ctrl Pts',(-0.0116339662207059,-0.0342371160987152,
-0.01067583877975));
#48814=CARTESIAN_POINT('Ctrl Pts',(-0.0125,-0.0342787827653818,-0.01067583877975));
#48815=CARTESIAN_POINT('Ctrl Pts',(-0.0133660337792941,-0.0343204494320485,
-0.01067583877975));
#48816=CARTESIAN_POINT('Ctrl Pts',(-0.0137990506689412,-0.0343621160987152,
-0.0114258460331541));
#48817=CARTESIAN_POINT('Ctrl Pts',(-0.0142320675585882,-0.0344037827653819,
-0.0121758532865583));
#48818=CARTESIAN_POINT('Ctrl Pts',(-0.0137990506689412,-0.0344454494320486,
-0.0129258605399625));
#48819=CARTESIAN_POINT('Ctrl Pts',(-0.0133660337792941,-0.0344871160987153,
-0.0136758677933666));
#48820=CARTESIAN_POINT('Ctrl Pts',(-0.0125,-0.0345287827653819,-0.0136758677933666));
#48821=CARTESIAN_POINT('Ctrl Pts',(-0.0116339662207059,-0.0345704494320486,
-0.0136758677933666));
#48822=CARTESIAN_POINT('Ctrl Pts',(-0.0112009493310588,-0.0346121160987153,
-0.0129258605399625));
#48823=CARTESIAN_POINT('Ctrl Pts',(-0.0107679324414118,-0.0346537827653819,
-0.0121758532865583));
#48824=CARTESIAN_POINT('Ctrl Pts',(-0.0112009493310588,-0.0346954494320485,
-0.0114258460331541));
#48825=CARTESIAN_POINT('Ctrl Pts',(-0.0116339662207059,-0.0347371160987151,
-0.01067583877975));
#48826=CARTESIAN_POINT('Ctrl Pts',(-0.0125,-0.0347787827653818,-0.01067583877975));
#48827=CARTESIAN_POINT('Ctrl Pts',(-0.0133660337792941,-0.0348204494320485,
-0.01067583877975));
#48828=CARTESIAN_POINT('Ctrl Pts',(-0.0137990506689412,-0.0348621160987152,
-0.0114258460331541));
#48829=CARTESIAN_POINT('Ctrl Pts',(-0.0142320675585882,-0.0349037827653819,
-0.0121758532865583));
#48830=CARTESIAN_POINT('Ctrl Pts',(-0.0137990506689412,-0.0349454494320486,
-0.0129258605399625));
#48831=CARTESIAN_POINT('Ctrl Pts',(-0.0133660337792941,-0.0349871160987152,
-0.0136758677933666));
#48832=CARTESIAN_POINT('Ctrl Pts',(-0.0125,-0.0350287827653819,-0.0136758677933666));
#48833=CARTESIAN_POINT('Ctrl Pts',(-0.0116339662207059,-0.0350704494320486,
-0.0136758677933666));
#48834=CARTESIAN_POINT('Ctrl Pts',(-0.0112009493310588,-0.0351121160987153,
-0.0129258605399625));
#48835=CARTESIAN_POINT('Ctrl Pts',(-0.0107679324414118,-0.0351537827653818,
-0.0121758532865583));
#48836=CARTESIAN_POINT('Ctrl Pts',(-0.0112009493310588,-0.0351954494320485,
-0.0114258460331541));
#48837=CARTESIAN_POINT('Ctrl Pts',(-0.0116339662207059,-0.0352371160987152,
-0.0106758387797499));
#48838=CARTESIAN_POINT('Ctrl Pts',(-0.0125,-0.0352787827653818,-0.01067583877975));
#48839=CARTESIAN_POINT('Ctrl Pts',(-0.0133660337792941,-0.0353204494320485,
-0.0106758387797499));
#48840=CARTESIAN_POINT('Ctrl Pts',(-0.0137990506689412,-0.0353621160987152,
-0.011425846033154));
#48841=CARTESIAN_POINT('Ctrl Pts',(-0.0142320675585882,-0.0354037827653818,
-0.0121758532865583));
#48842=CARTESIAN_POINT('Ctrl Pts',(-0.0137990506689412,-0.0354454494320486,
-0.0129258605399625));
#48843=CARTESIAN_POINT('Ctrl Pts',(-0.0133660337792941,-0.0354871160987153,
-0.0136758677933666));
#48844=CARTESIAN_POINT('Ctrl Pts',(-0.0125,-0.0355287827653819,-0.0136758677933666));
#48845=CARTESIAN_POINT('Ctrl Pts',(-0.0116339662207059,-0.0355704494320486,
-0.0136758677933666));
#48846=CARTESIAN_POINT('Ctrl Pts',(-0.0112009493310588,-0.0356121160987152,
-0.0129258605399625));
#48847=CARTESIAN_POINT('Ctrl Pts',(-0.0107679324414118,-0.0356537827653819,
-0.0121758532865583));
#48848=CARTESIAN_POINT('Ctrl Pts',(-0.0112009493310588,-0.0356954494320485,
-0.011425846033154));
#48849=CARTESIAN_POINT('Ctrl Pts',(-0.0116339662207059,-0.0357371160987152,
-0.0106758387797499));
#48850=CARTESIAN_POINT('Ctrl Pts',(-0.0125,-0.0357787827653818,-0.0106758387797499));
#48851=CARTESIAN_POINT('Ctrl Pts',(-0.0133660337792941,-0.0358204494320485,
-0.0106758387797499));
#48852=CARTESIAN_POINT('Ctrl Pts',(-0.0137990506689412,-0.0358621160987152,
-0.011425846033154));
#48853=CARTESIAN_POINT('Ctrl Pts',(-0.0142320675585882,-0.0359037827653819,
-0.0121758532865583));
#48854=CARTESIAN_POINT('Ctrl Pts',(-0.0137990506689412,-0.0359454494320486,
-0.0129258605399624));
#48855=CARTESIAN_POINT('Ctrl Pts',(-0.0133660337792941,-0.0359871160987153,
-0.0136758677933665));
#48856=CARTESIAN_POINT('Ctrl Pts',(-0.0125,-0.0360287827653819,-0.0136758677933665));
#48857=CARTESIAN_POINT('Ctrl Pts',(-0.0116339662207059,-0.0360704494320486,
-0.0136758677933665));
#48858=CARTESIAN_POINT('Ctrl Pts',(-0.0112009493310588,-0.0361121160987152,
-0.0129258605399624));
#48859=CARTESIAN_POINT('Ctrl Pts',(-0.0107679324414118,-0.0361537827653819,
-0.0121758532865582));
#48860=CARTESIAN_POINT('Ctrl Pts',(-0.0112009493310588,-0.0361954494320485,
-0.011425846033154));
#48861=CARTESIAN_POINT('Ctrl Pts',(-0.0116339662207059,-0.0362371160987151,
-0.0106758387797499));
#48862=CARTESIAN_POINT('Ctrl Pts',(-0.0125,-0.0362787827653818,-0.0106758387797499));
#48863=CARTESIAN_POINT('Ctrl Pts',(-0.0133660337792941,-0.0363204494320485,
-0.0106758387797499));
#48864=CARTESIAN_POINT('Ctrl Pts',(-0.0137990506689412,-0.0363621160987152,
-0.011425846033154));
#48865=CARTESIAN_POINT('Ctrl Pts',(-0.0142320675585882,-0.0364037827653818,
-0.0121758532865582));
#48866=CARTESIAN_POINT('Ctrl Pts',(-0.0137990506689412,-0.0364454494320486,
-0.0129258605399624));
#48867=CARTESIAN_POINT('Ctrl Pts',(-0.0133660337792941,-0.0364871160987152,
-0.0136758677933665));
#48868=CARTESIAN_POINT('Ctrl Pts',(-0.0125,-0.0365287827653819,-0.0136758677933665));
#48869=CARTESIAN_POINT('Ctrl Pts',(-0.0116339662207059,-0.0365704494320486,
-0.0136758677933665));
#48870=CARTESIAN_POINT('Ctrl Pts',(-0.0112009493310588,-0.0366121160987152,
-0.0129258605399624));
#48871=CARTESIAN_POINT('Ctrl Pts',(-0.0107679324414118,-0.0366537827653819,
-0.0121758532865582));
#48872=CARTESIAN_POINT('Ctrl Pts',(-0.0112009493310588,-0.0366954494320485,
-0.011425846033154));
#48873=CARTESIAN_POINT('Ctrl Pts',(-0.0116339662207059,-0.0367371160987152,
-0.0106758387797499));
#48874=CARTESIAN_POINT('Ctrl Pts',(-0.0125,-0.0367787827653818,-0.0106758387797499));
#48875=CARTESIAN_POINT('Ctrl Pts',(-0.0133660337792941,-0.0368204494320485,
-0.0106758387797499));
#48876=CARTESIAN_POINT('Ctrl Pts',(-0.0137990506689412,-0.0368621160987152,
-0.011425846033154));
#48877=CARTESIAN_POINT('Ctrl Pts',(-0.0142320675585882,-0.0369037827653819,
-0.0121758532865582));
#48878=CARTESIAN_POINT('Ctrl Pts',(-0.0137990506689412,-0.0369454494320486,
-0.0129258605399624));
#48879=CARTESIAN_POINT('Ctrl Pts',(-0.0133660337792941,-0.0369871160987153,
-0.0136758677933665));
#48880=CARTESIAN_POINT('Ctrl Pts',(-0.0125,-0.0370287827653819,-0.0136758677933665));
#48881=CARTESIAN_POINT('Ctrl Pts',(-0.0116339662207059,-0.0370704494320486,
-0.0136758677933665));
#48882=CARTESIAN_POINT('Ctrl Pts',(-0.0112009493310588,-0.0371121160987152,
-0.0129258605399624));
#48883=CARTESIAN_POINT('Ctrl Pts',(-0.0107679324414118,-0.0371537827653819,
-0.0121758532865582));
#48884=CARTESIAN_POINT('Ctrl Pts',(-0.0112009493310588,-0.0371954494320485,
-0.011425846033154));
#48885=CARTESIAN_POINT('Ctrl Pts',(-0.0116339662207059,-0.0372371160987152,
-0.0106758387797499));
#48886=CARTESIAN_POINT('Ctrl Pts',(-0.0125,-0.0372787827653818,-0.0106758387797499));
#48887=CARTESIAN_POINT('Ctrl Pts',(-0.0133660337792941,-0.0373204494320485,
-0.0106758387797499));
#48888=CARTESIAN_POINT('Ctrl Pts',(-0.0137990506689412,-0.0373621160987152,
-0.011425846033154));
#48889=CARTESIAN_POINT('Ctrl Pts',(-0.0142320675585882,-0.0374037827653819,
-0.0121758532865582));
#48890=CARTESIAN_POINT('Ctrl Pts',(-0.0137990506689412,-0.0374454494320486,
-0.0129258605399624));
#48891=CARTESIAN_POINT('Ctrl Pts',(-0.0133660337792941,-0.0374871160987152,
-0.0136758677933665));
#48892=CARTESIAN_POINT('Ctrl Pts',(-0.0125,-0.0375287827653819,-0.0136758677933665));
#48893=CARTESIAN_POINT('Ctrl Pts',(-0.0116339662207059,-0.0375704494320486,
-0.0136758677933665));
#48894=CARTESIAN_POINT('Ctrl Pts',(-0.0112009493310588,-0.0376121160987152,
-0.0129258605399624));
#48895=CARTESIAN_POINT('Ctrl Pts',(-0.0107679324414118,-0.0376537827653818,
-0.0121758532865582));
#48896=CARTESIAN_POINT('Ctrl Pts',(-0.0112009493310588,-0.0376954494320485,
-0.011425846033154));
#48897=CARTESIAN_POINT('Ctrl Pts',(-0.0116339662207059,-0.0377371160987151,
-0.0106758387797499));
#48898=CARTESIAN_POINT('Ctrl Pts',(-0.0125,-0.0377787827653818,-0.0106758387797499));
#48899=CARTESIAN_POINT('Ctrl Pts',(-0.0133660337792941,-0.0378204494320485,
-0.0106758387797499));
#48900=CARTESIAN_POINT('Ctrl Pts',(-0.0137990506689412,-0.0378621160987152,
-0.011425846033154));
#48901=CARTESIAN_POINT('Ctrl Pts',(-0.0142320675585882,-0.0379037827653818,
-0.0121758532865582));
#48902=CARTESIAN_POINT('Ctrl Pts',(-0.0137990506689412,-0.0379454494320486,
-0.0129258605399624));
#48903=CARTESIAN_POINT('Ctrl Pts',(-0.0133660337792941,-0.0379871160987152,
-0.0136758677933665));
#48904=CARTESIAN_POINT('Ctrl Pts',(-0.0125,-0.0380287827653819,-0.0136758677933665));
#48905=CARTESIAN_POINT('Ctrl Pts',(-0.0116339662207059,-0.0380704494320486,
-0.0136758677933665));
#48906=CARTESIAN_POINT('Ctrl Pts',(-0.0112009493310588,-0.0381121160987152,
-0.0129258605399624));
#48907=CARTESIAN_POINT('Ctrl Pts',(-0.0107679324414118,-0.0381537827653819,
-0.0121758532865582));
#48908=CARTESIAN_POINT('Ctrl Pts',(-0.0112009493310588,-0.0381954494320485,
-0.011425846033154));
#48909=CARTESIAN_POINT('Ctrl Pts',(-0.0116339662207059,-0.0382371160987152,
-0.0106758387797498));
#48910=CARTESIAN_POINT('Ctrl Pts',(-0.0125,-0.0382787827653818,-0.0106758387797499));
#48911=CARTESIAN_POINT('Ctrl Pts',(-0.0133660337792941,-0.0383204494320485,
-0.0106758387797498));
#48912=CARTESIAN_POINT('Ctrl Pts',(-0.0137990506689412,-0.0383621160987152,
-0.0114258460331539));
#48913=CARTESIAN_POINT('Ctrl Pts',(-0.0142320675585882,-0.0384037827653819,
-0.0121758532865581));
#48914=CARTESIAN_POINT('Ctrl Pts',(-0.0137990506689412,-0.0384454494320486,
-0.0129258605399624));
#48915=CARTESIAN_POINT('Ctrl Pts',(-0.0133660337792941,-0.0384871160987153,
-0.0136758677933665));
#48916=CARTESIAN_POINT('Ctrl Pts',(-0.0125,-0.0385287827653819,-0.0136758677933665));
#48917=CARTESIAN_POINT('Ctrl Pts',(-0.0116339662207059,-0.0385704494320486,
-0.0136758677933665));
#48918=CARTESIAN_POINT('Ctrl Pts',(-0.0112009493310588,-0.0386121160987152,
-0.0129258605399623));
#48919=CARTESIAN_POINT('Ctrl Pts',(-0.0107679324414118,-0.0386537827653819,
-0.0121758532865581));
#48920=CARTESIAN_POINT('Ctrl Pts',(-0.0112009493310588,-0.0386954494320485,
-0.0114258460331539));
#48921=CARTESIAN_POINT('Ctrl Pts',(-0.0116339662207059,-0.0387371160987151,
-0.0106758387797498));
#48922=CARTESIAN_POINT('Ctrl Pts',(-0.0125,-0.0387787827653818,-0.0106758387797498));
#48923=CARTESIAN_POINT('Ctrl Pts',(-0.0133660337792941,-0.0388204494320485,
-0.0106758387797498));
#48924=CARTESIAN_POINT('Ctrl Pts',(-0.0137990506689412,-0.0388621160987152,
-0.0114258460331539));
#48925=CARTESIAN_POINT('Ctrl Pts',(-0.0142320675585882,-0.0389037827653818,
-0.0121758532865581));
#48926=CARTESIAN_POINT('Ctrl Pts',(-0.0137990506689412,-0.0389454494320486,
-0.0129258605399623));
#48927=CARTESIAN_POINT('Ctrl Pts',(-0.0133660337792941,-0.0389871160987152,
-0.0136758677933665));
#48928=CARTESIAN_POINT('Ctrl Pts',(-0.0125,-0.0390287827653819,-0.0136758677933664));
#48929=CARTESIAN_POINT('Ctrl Pts',(-0.0116339662207059,-0.0390704494320486,
-0.0136758677933665));
#48930=CARTESIAN_POINT('Ctrl Pts',(-0.0112009493310588,-0.0391121160987152,
-0.0129258605399623));
#48931=CARTESIAN_POINT('Ctrl Pts',(-0.0107679324414118,-0.0391537827653818,
-0.0121758532865581));
#48932=CARTESIAN_POINT('Ctrl Pts',(-0.0112009493310588,-0.0391954494320485,
-0.0114258460331539));
#48933=CARTESIAN_POINT('Ctrl Pts',(-0.0116339662207059,-0.0392371160987152,
-0.0106758387797498));
#48934=CARTESIAN_POINT('Ctrl Pts',(-0.0125,-0.0392787827653818,-0.0106758387797498));
#48935=CARTESIAN_POINT('Ctrl Pts',(-0.0133660337792941,-0.0393204494320485,
-0.0106758387797498));
#48936=CARTESIAN_POINT('Ctrl Pts',(-0.0137990506689412,-0.0393621160987152,
-0.0114258460331539));
#48937=CARTESIAN_POINT('Ctrl Pts',(-0.0142320675585882,-0.0394037827653818,
-0.0121758532865581));
#48938=CARTESIAN_POINT('Ctrl Pts',(-0.0137990506689412,-0.0394454494320486,
-0.0129258605399623));
#48939=CARTESIAN_POINT('Ctrl Pts',(-0.0133660337792941,-0.0394871160987153,
-0.0136758677933664));
#48940=CARTESIAN_POINT('Ctrl Pts',(-0.0125,-0.0395287827653819,-0.0136758677933664));
#48941=CARTESIAN_POINT('Ctrl Pts',(-0.0116339662207059,-0.0395704494320486,
-0.0136758677933664));
#48942=CARTESIAN_POINT('Ctrl Pts',(-0.0112009493310588,-0.0396121160987152,
-0.0129258605399623));
#48943=CARTESIAN_POINT('Ctrl Pts',(-0.0107679324414118,-0.0396537827653819,
-0.0121758532865581));
#48944=CARTESIAN_POINT('Ctrl Pts',(-0.0112009493310588,-0.0396954494320485,
-0.0114258460331539));
#48945=CARTESIAN_POINT('Ctrl Pts',(-0.0116339662207059,-0.0397371160987151,
-0.0106758387797498));
#48946=CARTESIAN_POINT('Ctrl Pts',(-0.0125,-0.0397787827653818,-0.0106758387797498));
#48947=CARTESIAN_POINT('Ctrl Pts',(-0.0133660337792941,-0.0398204494320485,
-0.0106758387797498));
#48948=CARTESIAN_POINT('Ctrl Pts',(-0.0137990506689412,-0.0398621160987152,
-0.0114258460331539));
#48949=CARTESIAN_POINT('Ctrl Pts',(-0.0142320675585882,-0.0399037827653819,
-0.0121758532865581));
#48950=CARTESIAN_POINT('Ctrl Pts',(-0.0137990506689412,-0.0399454494320486,
-0.0129258605399623));
#48951=CARTESIAN_POINT('Ctrl Pts',(-0.0133660337792941,-0.0399871160987153,
-0.0136758677933664));
#48952=CARTESIAN_POINT('Ctrl Pts',(-0.0125,-0.0400287827653819,-0.0136758677933664));
#48953=CARTESIAN_POINT('Ctrl Pts',(-0.0116339662207059,-0.0400704494320486,
-0.0136758677933664));
#48954=CARTESIAN_POINT('Ctrl Pts',(-0.0112009493310588,-0.0401121160987152,
-0.0129258605399623));
#48955=CARTESIAN_POINT('Ctrl Pts',(-0.0107679324414118,-0.0401537827653819,
-0.0121758532865581));
#48956=CARTESIAN_POINT('Ctrl Pts',(-0.0112009493310588,-0.0401954494320485,
-0.0114258460331539));
#48957=CARTESIAN_POINT('Ctrl Pts',(-0.0116339662207059,-0.0402371160987151,
-0.0106758387797498));
#48958=CARTESIAN_POINT('Ctrl Pts',(-0.0125,-0.0402787827653818,-0.0106758387797498));
#48959=CARTESIAN_POINT('Ctrl Pts',(-0.0133660337792941,-0.0403204494320485,
-0.0106758387797498));
#48960=CARTESIAN_POINT('Ctrl Pts',(-0.0137990506689412,-0.0403621160987152,
-0.0114258460331539));
#48961=CARTESIAN_POINT('Ctrl Pts',(-0.0142320675585882,-0.0404037827653818,
-0.0121758532865581));
#48962=CARTESIAN_POINT('Ctrl Pts',(-0.0137990506689412,-0.0404454494320486,
-0.0129258605399623));
#48963=CARTESIAN_POINT('Ctrl Pts',(-0.0133660337792941,-0.0404871160987152,
-0.0136758677933664));
#48964=CARTESIAN_POINT('Ctrl Pts',(-0.0125,-0.0405287827653819,-0.0136758677933664));
#48965=CARTESIAN_POINT('Ctrl Pts',(-0.0116339662207059,-0.0405704494320486,
-0.0136758677933664));
#48966=CARTESIAN_POINT('Ctrl Pts',(-0.0112009493310588,-0.0406121160987152,
-0.0129258605399623));
#48967=CARTESIAN_POINT('Ctrl Pts',(-0.0107679324414118,-0.0406537827653819,
-0.0121758532865581));
#48968=CARTESIAN_POINT('Ctrl Pts',(-0.0112009493310588,-0.0406954494320485,
-0.0114258460331539));
#48969=CARTESIAN_POINT('Ctrl Pts',(-0.0116339662207059,-0.0407371160987152,
-0.0106758387797498));
#48970=CARTESIAN_POINT('Ctrl Pts',(-0.0125,-0.0407787827653818,-0.0106758387797498));
#48971=CARTESIAN_POINT('Ctrl Pts',(-0.0133660337792941,-0.0408204494320485,
-0.0106758387797498));
#48972=CARTESIAN_POINT('Ctrl Pts',(-0.0137990506689412,-0.0408621160987152,
-0.0114258460331539));
#48973=CARTESIAN_POINT('Ctrl Pts',(-0.0142320675585882,-0.0409037827653819,
-0.0121758532865581));
#48974=CARTESIAN_POINT('Ctrl Pts',(-0.0137990506689412,-0.0409454494320486,
-0.0129258605399623));
#48975=CARTESIAN_POINT('Ctrl Pts',(-0.0133660337792941,-0.0409871160987153,
-0.0136758677933664));
#48976=CARTESIAN_POINT('Ctrl Pts',(-0.0125,-0.0410287827653819,-0.0136758677933664));
#48977=CARTESIAN_POINT('Ctrl Pts',(-0.0116339662207059,-0.0410704494320486,
-0.0136758677933664));
#48978=CARTESIAN_POINT('Ctrl Pts',(-0.0112009493310588,-0.0411121160987152,
-0.0129258605399623));
#48979=CARTESIAN_POINT('Ctrl Pts',(-0.0107679324414118,-0.0411537827653819,
-0.012175853286558));
#48980=CARTESIAN_POINT('Ctrl Pts',(-0.0112009493310588,-0.0411954494320485,
-0.0114258460331539));
#48981=CARTESIAN_POINT('Ctrl Pts',(-0.0116339662207059,-0.0412371160987151,
-0.0106758387797497));
#48982=CARTESIAN_POINT('Ctrl Pts',(-0.0125,-0.0412787827653818,-0.0106758387797498));
#48983=CARTESIAN_POINT('Ctrl Pts',(-0.0133660337792941,-0.0413204494320485,
-0.0106758387797497));
#48984=CARTESIAN_POINT('Ctrl Pts',(-0.0137990506689412,-0.0413621160987152,
-0.0114258460331538));
#48985=CARTESIAN_POINT('Ctrl Pts',(-0.0142320675585882,-0.0414037827653819,
-0.012175853286558));
#48986=CARTESIAN_POINT('Ctrl Pts',(-0.0137990506689412,-0.0414454494320486,
-0.0129258605399623));
#48987=CARTESIAN_POINT('Ctrl Pts',(-0.0134462336521574,-0.0414793989369851,
-0.0135369575388066));
#48988=CARTESIAN_POINT('Ctrl Pts',(-0.012750509472736,-0.0415161450767976,
-0.0136548017389069));
#48989=CARTESIAN_POINT('Ctrl Pts',(-0.013319256622239,-0.0332791637687162,
-0.0130184532271587));
#48990=CARTESIAN_POINT('Ctrl Pts',(-0.0129771529854922,-0.0333119647977888,
-0.0133510792533334));
#48991=CARTESIAN_POINT('Ctrl Pts',(-0.0125,-0.033341266014364,-0.0133510792533334));
#48992=CARTESIAN_POINT('Ctrl Pts',(-0.0118214829717238,-0.0333829326810307,
-0.0133510792533334));
#48993=CARTESIAN_POINT('Ctrl Pts',(-0.0114822244575857,-0.0334245993476973,
-0.0127634662699458));
#48994=CARTESIAN_POINT('Ctrl Pts',(-0.0111429659434476,-0.033466266014364,
-0.0121758532865583));
#48995=CARTESIAN_POINT('Ctrl Pts',(-0.0114822244575857,-0.0335079326810306,
-0.0115882403031708));
#48996=CARTESIAN_POINT('Ctrl Pts',(-0.0118214829717238,-0.0335495993476973,
-0.0110006273197833));
#48997=CARTESIAN_POINT('Ctrl Pts',(-0.0125,-0.033591266014364,-0.0110006273197833));
#48998=CARTESIAN_POINT('Ctrl Pts',(-0.0131785170282762,-0.0336329326810306,
-0.0110006273197833));
#48999=CARTESIAN_POINT('Ctrl Pts',(-0.0135177755424142,-0.0336745993476973,
-0.0115882403031708));
#49000=CARTESIAN_POINT('Ctrl Pts',(-0.0138570340565524,-0.033716266014364,
-0.0121758532865583));
#49001=CARTESIAN_POINT('Ctrl Pts',(-0.0135177755424142,-0.0337579326810307,
-0.0127634662699458));
#49002=CARTESIAN_POINT('Ctrl Pts',(-0.0131785170282762,-0.0337995993476974,
-0.0133510792533333));
#49003=CARTESIAN_POINT('Ctrl Pts',(-0.0125,-0.0338412660143641,-0.0133510792533333));
#49004=CARTESIAN_POINT('Ctrl Pts',(-0.0118214829717238,-0.0338829326810307,
-0.0133510792533333));
#49005=CARTESIAN_POINT('Ctrl Pts',(-0.0114822244575857,-0.0339245993476973,
-0.0127634662699458));
#49006=CARTESIAN_POINT('Ctrl Pts',(-0.0111429659434476,-0.033966266014364,
-0.0121758532865583));
#49007=CARTESIAN_POINT('Ctrl Pts',(-0.0114822244575857,-0.0340079326810306,
-0.0115882403031708));
#49008=CARTESIAN_POINT('Ctrl Pts',(-0.0118214829717238,-0.0340495993476973,
-0.0110006273197833));
#49009=CARTESIAN_POINT('Ctrl Pts',(-0.0125,-0.034091266014364,-0.0110006273197833));
#49010=CARTESIAN_POINT('Ctrl Pts',(-0.0131785170282762,-0.0341329326810306,
-0.0110006273197833));
#49011=CARTESIAN_POINT('Ctrl Pts',(-0.0135177755424142,-0.0341745993476973,
-0.0115882403031708));
#49012=CARTESIAN_POINT('Ctrl Pts',(-0.0138570340565524,-0.034216266014364,
-0.0121758532865583));
#49013=CARTESIAN_POINT('Ctrl Pts',(-0.0135177755424142,-0.0342579326810307,
-0.0127634662699458));
#49014=CARTESIAN_POINT('Ctrl Pts',(-0.0131785170282762,-0.0342995993476974,
-0.0133510792533333));
#49015=CARTESIAN_POINT('Ctrl Pts',(-0.0125,-0.0343412660143641,-0.0133510792533333));
#49016=CARTESIAN_POINT('Ctrl Pts',(-0.0118214829717238,-0.0343829326810307,
-0.0133510792533333));
#49017=CARTESIAN_POINT('Ctrl Pts',(-0.0114822244575857,-0.0344245993476973,
-0.0127634662699458));
#49018=CARTESIAN_POINT('Ctrl Pts',(-0.0111429659434476,-0.034466266014364,
-0.0121758532865583));
#49019=CARTESIAN_POINT('Ctrl Pts',(-0.0114822244575857,-0.0345079326810307,
-0.0115882403031708));
#49020=CARTESIAN_POINT('Ctrl Pts',(-0.0118214829717238,-0.0345495993476973,
-0.0110006273197833));
#49021=CARTESIAN_POINT('Ctrl Pts',(-0.0125,-0.034591266014364,-0.0110006273197833));
#49022=CARTESIAN_POINT('Ctrl Pts',(-0.0131785170282762,-0.0346329326810306,
-0.0110006273197833));
#49023=CARTESIAN_POINT('Ctrl Pts',(-0.0135177755424142,-0.0346745993476973,
-0.0115882403031708));
#49024=CARTESIAN_POINT('Ctrl Pts',(-0.0138570340565524,-0.034716266014364,
-0.0121758532865583));
#49025=CARTESIAN_POINT('Ctrl Pts',(-0.0135177755424142,-0.0347579326810307,
-0.0127634662699458));
#49026=CARTESIAN_POINT('Ctrl Pts',(-0.0131785170282762,-0.0347995993476974,
-0.0133510792533333));
#49027=CARTESIAN_POINT('Ctrl Pts',(-0.0125,-0.0348412660143641,-0.0133510792533333));
#49028=CARTESIAN_POINT('Ctrl Pts',(-0.0118214829717238,-0.0348829326810306,
-0.0133510792533333));
#49029=CARTESIAN_POINT('Ctrl Pts',(-0.0114822244575857,-0.0349245993476973,
-0.0127634662699458));
#49030=CARTESIAN_POINT('Ctrl Pts',(-0.0111429659434476,-0.034966266014364,
-0.0121758532865583));
#49031=CARTESIAN_POINT('Ctrl Pts',(-0.0114822244575857,-0.0350079326810307,
-0.0115882403031708));
#49032=CARTESIAN_POINT('Ctrl Pts',(-0.0118214829717238,-0.0350495993476973,
-0.0110006273197832));
#49033=CARTESIAN_POINT('Ctrl Pts',(-0.0125,-0.035091266014364,-0.0110006273197832));
#49034=CARTESIAN_POINT('Ctrl Pts',(-0.0131785170282762,-0.0351329326810307,
-0.0110006273197832));
#49035=CARTESIAN_POINT('Ctrl Pts',(-0.0135177755424142,-0.0351745993476973,
-0.0115882403031707));
#49036=CARTESIAN_POINT('Ctrl Pts',(-0.0138570340565524,-0.035216266014364,
-0.0121758532865583));
#49037=CARTESIAN_POINT('Ctrl Pts',(-0.0135177755424142,-0.0352579326810307,
-0.0127634662699458));
#49038=CARTESIAN_POINT('Ctrl Pts',(-0.0131785170282762,-0.0352995993476974,
-0.0133510792533333));
#49039=CARTESIAN_POINT('Ctrl Pts',(-0.0125,-0.0353412660143641,-0.0133510792533333));
#49040=CARTESIAN_POINT('Ctrl Pts',(-0.0118214829717238,-0.0353829326810307,
-0.0133510792533333));
#49041=CARTESIAN_POINT('Ctrl Pts',(-0.0114822244575857,-0.0354245993476973,
-0.0127634662699458));
#49042=CARTESIAN_POINT('Ctrl Pts',(-0.0111429659434476,-0.035466266014364,
-0.0121758532865583));
#49043=CARTESIAN_POINT('Ctrl Pts',(-0.0114822244575857,-0.0355079326810307,
-0.0115882403031707));
#49044=CARTESIAN_POINT('Ctrl Pts',(-0.0118214829717238,-0.0355495993476973,
-0.0110006273197832));
#49045=CARTESIAN_POINT('Ctrl Pts',(-0.0125,-0.035591266014364,-0.0110006273197832));
#49046=CARTESIAN_POINT('Ctrl Pts',(-0.0131785170282762,-0.0356329326810306,
-0.0110006273197832));
#49047=CARTESIAN_POINT('Ctrl Pts',(-0.0135177755424142,-0.0356745993476973,
-0.0115882403031707));
#49048=CARTESIAN_POINT('Ctrl Pts',(-0.0138570340565524,-0.035716266014364,
-0.0121758532865583));
#49049=CARTESIAN_POINT('Ctrl Pts',(-0.0135177755424142,-0.0357579326810307,
-0.0127634662699458));
#49050=CARTESIAN_POINT('Ctrl Pts',(-0.0131785170282762,-0.0357995993476973,
-0.0133510792533333));
#49051=CARTESIAN_POINT('Ctrl Pts',(-0.0125,-0.0358412660143641,-0.0133510792533333));
#49052=CARTESIAN_POINT('Ctrl Pts',(-0.0118214829717238,-0.0358829326810307,
-0.0133510792533333));
#49053=CARTESIAN_POINT('Ctrl Pts',(-0.0114822244575857,-0.0359245993476973,
-0.0127634662699458));
#49054=CARTESIAN_POINT('Ctrl Pts',(-0.0111429659434476,-0.035966266014364,
-0.0121758532865583));
#49055=CARTESIAN_POINT('Ctrl Pts',(-0.0114822244575857,-0.0360079326810307,
-0.0115882403031707));
#49056=CARTESIAN_POINT('Ctrl Pts',(-0.0118214829717238,-0.0360495993476973,
-0.0110006273197832));
#49057=CARTESIAN_POINT('Ctrl Pts',(-0.0125,-0.0360912660143639,-0.0110006273197832));
#49058=CARTESIAN_POINT('Ctrl Pts',(-0.0131785170282762,-0.0361329326810306,
-0.0110006273197832));
#49059=CARTESIAN_POINT('Ctrl Pts',(-0.0135177755424142,-0.0361745993476973,
-0.0115882403031707));
#49060=CARTESIAN_POINT('Ctrl Pts',(-0.0138570340565524,-0.036216266014364,
-0.0121758532865582));
#49061=CARTESIAN_POINT('Ctrl Pts',(-0.0135177755424142,-0.0362579326810307,
-0.0127634662699457));
#49062=CARTESIAN_POINT('Ctrl Pts',(-0.0131785170282762,-0.0362995993476974,
-0.0133510792533332));
#49063=CARTESIAN_POINT('Ctrl Pts',(-0.0125,-0.036341266014364,-0.0133510792533333));
#49064=CARTESIAN_POINT('Ctrl Pts',(-0.0118214829717238,-0.0363829326810307,
-0.0133510792533332));
#49065=CARTESIAN_POINT('Ctrl Pts',(-0.0114822244575857,-0.0364245993476973,
-0.0127634662699457));
#49066=CARTESIAN_POINT('Ctrl Pts',(-0.0111429659434476,-0.036466266014364,
-0.0121758532865582));
#49067=CARTESIAN_POINT('Ctrl Pts',(-0.0114822244575857,-0.0365079326810307,
-0.0115882403031707));
#49068=CARTESIAN_POINT('Ctrl Pts',(-0.0118214829717238,-0.0365495993476973,
-0.0110006273197832));
#49069=CARTESIAN_POINT('Ctrl Pts',(-0.0125,-0.0365912660143639,-0.0110006273197832));
#49070=CARTESIAN_POINT('Ctrl Pts',(-0.0131785170282762,-0.0366329326810306,
-0.0110006273197832));
#49071=CARTESIAN_POINT('Ctrl Pts',(-0.0135177755424142,-0.0366745993476973,
-0.0115882403031707));
#49072=CARTESIAN_POINT('Ctrl Pts',(-0.0138570340565524,-0.036716266014364,
-0.0121758532865582));
#49073=CARTESIAN_POINT('Ctrl Pts',(-0.0135177755424142,-0.0367579326810307,
-0.0127634662699457));
#49074=CARTESIAN_POINT('Ctrl Pts',(-0.0131785170282762,-0.0367995993476974,
-0.0133510792533332));
#49075=CARTESIAN_POINT('Ctrl Pts',(-0.0125,-0.036841266014364,-0.0133510792533332));
#49076=CARTESIAN_POINT('Ctrl Pts',(-0.0118214829717238,-0.0368829326810307,
-0.0133510792533332));
#49077=CARTESIAN_POINT('Ctrl Pts',(-0.0114822244575857,-0.0369245993476973,
-0.0127634662699457));
#49078=CARTESIAN_POINT('Ctrl Pts',(-0.0111429659434476,-0.036966266014364,
-0.0121758532865582));
#49079=CARTESIAN_POINT('Ctrl Pts',(-0.0114822244575857,-0.0370079326810307,
-0.0115882403031707));
#49080=CARTESIAN_POINT('Ctrl Pts',(-0.0118214829717238,-0.0370495993476973,
-0.0110006273197832));
#49081=CARTESIAN_POINT('Ctrl Pts',(-0.0125,-0.0370912660143639,-0.0110006273197832));
#49082=CARTESIAN_POINT('Ctrl Pts',(-0.0131785170282762,-0.0371329326810306,
-0.0110006273197832));
#49083=CARTESIAN_POINT('Ctrl Pts',(-0.0135177755424142,-0.0371745993476973,
-0.0115882403031707));
#49084=CARTESIAN_POINT('Ctrl Pts',(-0.0138570340565524,-0.037216266014364,
-0.0121758532865582));
#49085=CARTESIAN_POINT('Ctrl Pts',(-0.0135177755424142,-0.0372579326810307,
-0.0127634662699457));
#49086=CARTESIAN_POINT('Ctrl Pts',(-0.0131785170282762,-0.0372995993476973,
-0.0133510792533332));
#49087=CARTESIAN_POINT('Ctrl Pts',(-0.0125,-0.037341266014364,-0.0133510792533332));
#49088=CARTESIAN_POINT('Ctrl Pts',(-0.0118214829717238,-0.0373829326810307,
-0.0133510792533332));
#49089=CARTESIAN_POINT('Ctrl Pts',(-0.0114822244575857,-0.0374245993476973,
-0.0127634662699457));
#49090=CARTESIAN_POINT('Ctrl Pts',(-0.0111429659434476,-0.037466266014364,
-0.0121758532865582));
#49091=CARTESIAN_POINT('Ctrl Pts',(-0.0114822244575857,-0.0375079326810307,
-0.0115882403031707));
#49092=CARTESIAN_POINT('Ctrl Pts',(-0.0118214829717238,-0.0375495993476973,
-0.0110006273197832));
#49093=CARTESIAN_POINT('Ctrl Pts',(-0.0125,-0.0375912660143639,-0.0110006273197831));
#49094=CARTESIAN_POINT('Ctrl Pts',(-0.0131785170282762,-0.0376329326810306,
-0.0110006273197831));
#49095=CARTESIAN_POINT('Ctrl Pts',(-0.0135177755424142,-0.0376745993476973,
-0.0115882403031707));
#49096=CARTESIAN_POINT('Ctrl Pts',(-0.0138570340565524,-0.037716266014364,
-0.0121758532865582));
#49097=CARTESIAN_POINT('Ctrl Pts',(-0.0135177755424142,-0.0377579326810307,
-0.0127634662699457));
#49098=CARTESIAN_POINT('Ctrl Pts',(-0.0131785170282762,-0.0377995993476974,
-0.0133510792533332));
#49099=CARTESIAN_POINT('Ctrl Pts',(-0.0125,-0.037841266014364,-0.0133510792533332));
#49100=CARTESIAN_POINT('Ctrl Pts',(-0.0118214829717238,-0.0378829326810307,
-0.0133510792533332));
#49101=CARTESIAN_POINT('Ctrl Pts',(-0.0114822244575857,-0.0379245993476974,
-0.0127634662699457));
#49102=CARTESIAN_POINT('Ctrl Pts',(-0.0111429659434476,-0.037966266014364,
-0.0121758532865582));
#49103=CARTESIAN_POINT('Ctrl Pts',(-0.0114822244575857,-0.0380079326810307,
-0.0115882403031707));
#49104=CARTESIAN_POINT('Ctrl Pts',(-0.0118214829717238,-0.0380495993476973,
-0.0110006273197831));
#49105=CARTESIAN_POINT('Ctrl Pts',(-0.0125,-0.0380912660143639,-0.0110006273197831));
#49106=CARTESIAN_POINT('Ctrl Pts',(-0.0131785170282762,-0.0381329326810306,
-0.0110006273197831));
#49107=CARTESIAN_POINT('Ctrl Pts',(-0.0135177755424142,-0.0381745993476973,
-0.0115882403031706));
#49108=CARTESIAN_POINT('Ctrl Pts',(-0.0138570340565524,-0.038216266014364,
-0.0121758532865582));
#49109=CARTESIAN_POINT('Ctrl Pts',(-0.0135177755424142,-0.0382579326810306,
-0.0127634662699457));
#49110=CARTESIAN_POINT('Ctrl Pts',(-0.0131785170282762,-0.0382995993476974,
-0.0133510792533332));
#49111=CARTESIAN_POINT('Ctrl Pts',(-0.0125,-0.038341266014364,-0.0133510792533332));
#49112=CARTESIAN_POINT('Ctrl Pts',(-0.0118214829717238,-0.0383829326810307,
-0.0133510792533332));
#49113=CARTESIAN_POINT('Ctrl Pts',(-0.0114822244575857,-0.0384245993476974,
-0.0127634662699457));
#49114=CARTESIAN_POINT('Ctrl Pts',(-0.0111429659434476,-0.0384662660143639,
-0.0121758532865581));
#49115=CARTESIAN_POINT('Ctrl Pts',(-0.0114822244575857,-0.0385079326810306,
-0.0115882403031706));
#49116=CARTESIAN_POINT('Ctrl Pts',(-0.0118214829717238,-0.0385495993476973,
-0.0110006273197831));
#49117=CARTESIAN_POINT('Ctrl Pts',(-0.0125,-0.038591266014364,-0.0110006273197831));
#49118=CARTESIAN_POINT('Ctrl Pts',(-0.0131785170282762,-0.0386329326810306,
-0.0110006273197831));
#49119=CARTESIAN_POINT('Ctrl Pts',(-0.0135177755424142,-0.0386745993476973,
-0.0115882403031706));
#49120=CARTESIAN_POINT('Ctrl Pts',(-0.0138570340565524,-0.038716266014364,
-0.0121758532865581));
#49121=CARTESIAN_POINT('Ctrl Pts',(-0.0135177755424142,-0.0387579326810306,
-0.0127634662699457));
#49122=CARTESIAN_POINT('Ctrl Pts',(-0.0131785170282762,-0.0387995993476974,
-0.0133510792533332));
#49123=CARTESIAN_POINT('Ctrl Pts',(-0.0125,-0.038841266014364,-0.0133510792533332));
#49124=CARTESIAN_POINT('Ctrl Pts',(-0.0118214829717238,-0.0388829326810307,
-0.0133510792533332));
#49125=CARTESIAN_POINT('Ctrl Pts',(-0.0114822244575857,-0.0389245993476974,
-0.0127634662699456));
#49126=CARTESIAN_POINT('Ctrl Pts',(-0.0111429659434476,-0.038966266014364,
-0.0121758532865581));
#49127=CARTESIAN_POINT('Ctrl Pts',(-0.0114822244575857,-0.0390079326810306,
-0.0115882403031706));
#49128=CARTESIAN_POINT('Ctrl Pts',(-0.0118214829717238,-0.0390495993476973,
-0.0110006273197831));
#49129=CARTESIAN_POINT('Ctrl Pts',(-0.0125,-0.039091266014364,-0.0110006273197831));
#49130=CARTESIAN_POINT('Ctrl Pts',(-0.0131785170282762,-0.0391329326810306,
-0.0110006273197831));
#49131=CARTESIAN_POINT('Ctrl Pts',(-0.0135177755424142,-0.0391745993476973,
-0.0115882403031706));
#49132=CARTESIAN_POINT('Ctrl Pts',(-0.0138570340565524,-0.039216266014364,
-0.0121758532865581));
#49133=CARTESIAN_POINT('Ctrl Pts',(-0.0135177755424142,-0.0392579326810306,
-0.0127634662699456));
#49134=CARTESIAN_POINT('Ctrl Pts',(-0.0131785170282762,-0.0392995993476974,
-0.0133510792533332));
#49135=CARTESIAN_POINT('Ctrl Pts',(-0.0125,-0.039341266014364,-0.0133510792533331));
#49136=CARTESIAN_POINT('Ctrl Pts',(-0.0118214829717238,-0.0393829326810307,
-0.0133510792533332));
#49137=CARTESIAN_POINT('Ctrl Pts',(-0.0114822244575857,-0.0394245993476974,
-0.0127634662699456));
#49138=CARTESIAN_POINT('Ctrl Pts',(-0.0111429659434476,-0.039466266014364,
-0.0121758532865581));
#49139=CARTESIAN_POINT('Ctrl Pts',(-0.0114822244575857,-0.0395079326810306,
-0.0115882403031706));
#49140=CARTESIAN_POINT('Ctrl Pts',(-0.0118214829717238,-0.0395495993476973,
-0.0110006273197831));
#49141=CARTESIAN_POINT('Ctrl Pts',(-0.0125,-0.039591266014364,-0.0110006273197831));
#49142=CARTESIAN_POINT('Ctrl Pts',(-0.0131785170282762,-0.0396329326810306,
-0.0110006273197831));
#49143=CARTESIAN_POINT('Ctrl Pts',(-0.0135177755424142,-0.0396745993476973,
-0.0115882403031706));
#49144=CARTESIAN_POINT('Ctrl Pts',(-0.0138570340565524,-0.039716266014364,
-0.0121758532865581));
#49145=CARTESIAN_POINT('Ctrl Pts',(-0.0135177755424142,-0.0397579326810306,
-0.0127634662699456));
#49146=CARTESIAN_POINT('Ctrl Pts',(-0.0131785170282762,-0.0397995993476973,
-0.0133510792533331));
#49147=CARTESIAN_POINT('Ctrl Pts',(-0.0125,-0.039841266014364,-0.0133510792533331));
#49148=CARTESIAN_POINT('Ctrl Pts',(-0.0118214829717238,-0.0398829326810307,
-0.0133510792533331));
#49149=CARTESIAN_POINT('Ctrl Pts',(-0.0114822244575857,-0.0399245993476974,
-0.0127634662699456));
#49150=CARTESIAN_POINT('Ctrl Pts',(-0.0111429659434476,-0.039966266014364,
-0.0121758532865581));
#49151=CARTESIAN_POINT('Ctrl Pts',(-0.0114822244575857,-0.0400079326810306,
-0.0115882403031706));
#49152=CARTESIAN_POINT('Ctrl Pts',(-0.0118214829717238,-0.0400495993476973,
-0.0110006273197831));
#49153=CARTESIAN_POINT('Ctrl Pts',(-0.0125,-0.040091266014364,-0.0110006273197831));
#49154=CARTESIAN_POINT('Ctrl Pts',(-0.0131785170282762,-0.0401329326810306,
-0.0110006273197831));
#49155=CARTESIAN_POINT('Ctrl Pts',(-0.0135177755424142,-0.0401745993476973,
-0.0115882403031706));
#49156=CARTESIAN_POINT('Ctrl Pts',(-0.0138570340565524,-0.040216266014364,
-0.0121758532865581));
#49157=CARTESIAN_POINT('Ctrl Pts',(-0.0135177755424142,-0.0402579326810306,
-0.0127634662699456));
#49158=CARTESIAN_POINT('Ctrl Pts',(-0.0131785170282762,-0.0402995993476974,
-0.0133510792533331));
#49159=CARTESIAN_POINT('Ctrl Pts',(-0.0125,-0.040341266014364,-0.0133510792533331));
#49160=CARTESIAN_POINT('Ctrl Pts',(-0.0118214829717238,-0.0403829326810307,
-0.0133510792533331));
#49161=CARTESIAN_POINT('Ctrl Pts',(-0.0114822244575857,-0.0404245993476973,
-0.0127634662699456));
#49162=CARTESIAN_POINT('Ctrl Pts',(-0.0111429659434476,-0.040466266014364,
-0.0121758532865581));
#49163=CARTESIAN_POINT('Ctrl Pts',(-0.0114822244575857,-0.0405079326810306,
-0.0115882403031706));
#49164=CARTESIAN_POINT('Ctrl Pts',(-0.0118214829717238,-0.0405495993476973,
-0.0110006273197831));
#49165=CARTESIAN_POINT('Ctrl Pts',(-0.0125,-0.040591266014364,-0.011000627319783));
#49166=CARTESIAN_POINT('Ctrl Pts',(-0.0131785170282762,-0.0406329326810306,
-0.011000627319783));
#49167=CARTESIAN_POINT('Ctrl Pts',(-0.0135177755424142,-0.0406745993476973,
-0.0115882403031706));
#49168=CARTESIAN_POINT('Ctrl Pts',(-0.0138570340565524,-0.040716266014364,
-0.0121758532865581));
#49169=CARTESIAN_POINT('Ctrl Pts',(-0.0135177755424142,-0.0407579326810306,
-0.0127634662699456));
#49170=CARTESIAN_POINT('Ctrl Pts',(-0.0131785170282762,-0.0407995993476974,
-0.0133510792533331));
#49171=CARTESIAN_POINT('Ctrl Pts',(-0.0125,-0.040841266014364,-0.0133510792533331));
#49172=CARTESIAN_POINT('Ctrl Pts',(-0.0118214829717238,-0.0408829326810307,
-0.0133510792533331));
#49173=CARTESIAN_POINT('Ctrl Pts',(-0.0114822244575857,-0.0409245993476973,
-0.0127634662699456));
#49174=CARTESIAN_POINT('Ctrl Pts',(-0.0111429659434476,-0.040966266014364,
-0.0121758532865581));
#49175=CARTESIAN_POINT('Ctrl Pts',(-0.0114822244575857,-0.0410079326810306,
-0.0115882403031705));
#49176=CARTESIAN_POINT('Ctrl Pts',(-0.0118214829717238,-0.0410495993476973,
-0.011000627319783));
#49177=CARTESIAN_POINT('Ctrl Pts',(-0.0125,-0.041091266014364,-0.011000627319783));
#49178=CARTESIAN_POINT('Ctrl Pts',(-0.0131785170282762,-0.0411329326810306,
-0.011000627319783));
#49179=CARTESIAN_POINT('Ctrl Pts',(-0.0135177755424142,-0.0411745993476973,
-0.0115882403031705));
#49180=CARTESIAN_POINT('Ctrl Pts',(-0.0138570340565524,-0.041216266014364,
-0.012175853286558));
#49181=CARTESIAN_POINT('Ctrl Pts',(-0.0135177755424142,-0.0412579326810306,
-0.0127634662699456));
#49182=CARTESIAN_POINT('Ctrl Pts',(-0.0132413517360028,-0.0412918821859672,
-0.0132422463470719));
#49183=CARTESIAN_POINT('Ctrl Pts',(-0.0126962682600376,-0.0413286283257797,
-0.0133345744968084));
#49184=CARTESIAN_POINT('Ctrl Pts',(-0.0125000000004755,-0.0412787743898721,
-0.0106758532865977));
#49185=CARTESIAN_POINT('Ctrl Pts',(-0.0125791534151202,-0.0412787743898721,
-0.0106824494045114));
#49186=CARTESIAN_POINT('Ctrl Pts',(-0.012747840893727,-0.0412787743898722,
-0.0107019181802518));
#49187=CARTESIAN_POINT('Ctrl Pts',(-0.0130748131830085,-0.0412787743898722,
-0.0108429922798694));
#49188=CARTESIAN_POINT('Ctrl Pts',(-0.0131946039736345,-0.0412787743898722,
-0.0109172484796293));
#49189=CARTESIAN_POINT('Ctrl Pts',(-0.0134365405523043,-0.0412787743898722,
-0.0111221468405966));
#49190=CARTESIAN_POINT('Ctrl Pts',(-0.0135489323007065,-0.0412787743876939,
-0.0112606089599943));
#49191=CARTESIAN_POINT('Ctrl Pts',(-0.0136815652166612,-0.041278774387694,
-0.0115057517085288));
#49192=CARTESIAN_POINT('Ctrl Pts',(-0.0137143235950122,-0.0412787743898722,
-0.0115888928601645));
#49193=CARTESIAN_POINT('Ctrl Pts',(-0.0137820146531768,-0.0412787743898722,
-0.011813467117283));
#49194=CARTESIAN_POINT('Ctrl Pts',(-0.0137993725080859,-0.0412787743898722,
-0.0119695136960876));
#49195=CARTESIAN_POINT('Ctrl Pts',(-0.0137763187378415,-0.0412787743898722,
-0.012289886224141));
#49196=CARTESIAN_POINT('Ctrl Pts',(-0.0137324577582181,-0.0412787743898722,
-0.012450985065106));
#49197=CARTESIAN_POINT('Ctrl Pts',(-0.0136184626350962,-0.0412787743898722,
-0.0126812497443392));
#49198=CARTESIAN_POINT('Ctrl Pts',(-0.0135679181647976,-0.0412787743897922,
-0.0127611938063621));
#49199=CARTESIAN_POINT('Ctrl Pts',(-0.0134548766008996,-0.0412787743897922,
-0.012900132909092));
#49200=CARTESIAN_POINT('Ctrl Pts',(-0.0133923323265011,-0.0412787743898722,
-0.0129611541294956));
#49201=CARTESIAN_POINT('Ctrl Pts',(-0.0133234078741649,-0.0412787743898722,
-0.013014417323174));
#49202=CARTESIAN_POINT('Origin',(-0.0125,-0.0429287743898722,-0.013675853286558));
#49203=CARTESIAN_POINT('',(-0.0135,-0.0429287743898722,-0.0115985030173684));
#49204=CARTESIAN_POINT('',(-0.0135,-0.0429287743898722,-0.0127532035557476));
#49205=CARTESIAN_POINT('Origin',(-0.0125,-0.0429287743898722,-0.012175853286558));
#49206=CARTESIAN_POINT('',(-0.0125,-0.0429287743898722,-0.0110211527481787));
#49207=CARTESIAN_POINT('Origin',(-0.0125,-0.0429287743898722,-0.012175853286558));
#49208=CARTESIAN_POINT('Origin',(-0.0125,-0.0429287743898722,-0.012175853286558));
#49209=CARTESIAN_POINT('',(-0.0125,-0.0429287743898722,-0.0133305538249372));
#49210=CARTESIAN_POINT('Origin',(-0.0125,-0.0429287743898722,-0.012175853286558));
#49211=CARTESIAN_POINT('Origin',(-0.0125,-0.0429287743898722,-0.012175853286558));
#49212=CARTESIAN_POINT('Origin',(-0.0125,-0.0412787743898723,-0.015025853286558));
#49213=CARTESIAN_POINT('Origin',(-0.0125,-0.0429287743898722,-0.012175853286558));
#49214=CARTESIAN_POINT('Ctrl Pts',(-0.0114999999999901,-0.0429287743898621,
-0.0115985030173583));
#49215=CARTESIAN_POINT('Ctrl Pts',(-0.01199999999999,-0.0426400992552674,
-0.0113098278827636));
#49216=CARTESIAN_POINT('Ctrl Pts',(-0.01249999999999,-0.0429287743898621,
-0.0110211527481688));
#49217=CARTESIAN_POINT('Origin',(-0.0125,-0.0429287743898722,-0.012175853286558));
#49218=CARTESIAN_POINT('Ctrl Pts',(-0.01250000000001,-0.0429287743898621,
-0.0110211527481688));
#49219=CARTESIAN_POINT('Ctrl Pts',(-0.01300000000001,-0.0426400992552674,
-0.0113098278827636));
#49220=CARTESIAN_POINT('Ctrl Pts',(-0.01350000000001,-0.0429287743898621,
-0.0115985030173583));
#49221=CARTESIAN_POINT('Origin',(-0.0125,-0.0429287743898722,-0.012175853286558));
#49222=CARTESIAN_POINT('Ctrl Pts',(-0.01350000000001,-0.0429287743898621,
-0.0115985030173584));
#49223=CARTESIAN_POINT('Ctrl Pts',(-0.01350000000001,-0.0426400992552674,
-0.012175853286548));
#49224=CARTESIAN_POINT('Ctrl Pts',(-0.01350000000001,-0.0429287743898622,
-0.0127532035557576));
#49225=CARTESIAN_POINT('Origin',(-0.0125,-0.0429287743898722,-0.012175853286558));
#49226=CARTESIAN_POINT('Ctrl Pts',(-0.01350000000001,-0.0429287743898622,
-0.0127532035557576));
#49227=CARTESIAN_POINT('Ctrl Pts',(-0.01300000000001,-0.0426400992552675,
-0.0130418786903524));
#49228=CARTESIAN_POINT('Ctrl Pts',(-0.01250000000001,-0.0429287743898622,
-0.0133305538249472));
#49229=CARTESIAN_POINT('Origin',(-0.0125,-0.0429287743898722,-0.012175853286558));
#49230=CARTESIAN_POINT('Ctrl Pts',(-0.01249999999999,-0.0429287743898622,
-0.0133305538249472));
#49231=CARTESIAN_POINT('Ctrl Pts',(-0.01199999999999,-0.0426400992552675,
-0.0130418786903524));
#49232=CARTESIAN_POINT('Ctrl Pts',(-0.0114999999999901,-0.0429287743898622,
-0.0127532035557576));
#49233=CARTESIAN_POINT('Origin',(-0.0115,-0.0417737743898722,-0.0127532035557477));
#49234=CARTESIAN_POINT('',(-0.0125,-0.0417737743898722,-0.0133305538249373));
#49235=CARTESIAN_POINT('',(-0.0115,-0.0417737743898722,-0.0127532035557477));
#49236=CARTESIAN_POINT('',(-0.01249999999999,-0.0417737743898622,-0.0133305538249473));
#49237=CARTESIAN_POINT('',(-0.0115,-0.0417737743898722,-0.0115985030173684));
#49238=CARTESIAN_POINT('',(-0.01149999999999,-0.0417737743898622,-0.0127532035557577));
#49239=CARTESIAN_POINT('',(-0.0125,-0.0417737743898721,-0.0110211527481788));
#49240=CARTESIAN_POINT('',(-0.01149999999999,-0.0417737743898622,-0.0115985030173584));
#49241=CARTESIAN_POINT('',(-0.0135,-0.0417737743898722,-0.0115985030173684));
#49242=CARTESIAN_POINT('',(-0.01250000000001,-0.0417737743898621,-0.0110211527481688));
#49243=CARTESIAN_POINT('',(-0.0135,-0.0417737743898722,-0.0127532035557477));
#49244=CARTESIAN_POINT('',(-0.01350000000001,-0.0417737743898622,-0.0115985030173584));
#49245=CARTESIAN_POINT('',(-0.01350000000001,-0.0417737743898622,-0.0127532035557577));
#49246=CARTESIAN_POINT('Origin',(-0.0115,-0.0417737743898722,-0.0127532035557477));
#49247=CARTESIAN_POINT('',(-0.01149999999999,-0.0417737743898622,-0.0127532035557577));
#49248=CARTESIAN_POINT('',(-0.01149999999999,-0.0417737743898622,-0.0115985030173584));
#49249=CARTESIAN_POINT('Origin',(-0.0115,-0.0417737743898722,-0.0115985030173684));
#49250=CARTESIAN_POINT('',(-0.01250000000001,-0.0417737743898621,-0.0110211527481688));
#49251=CARTESIAN_POINT('Origin',(-0.0125,-0.0417737743898721,-0.0110211527481788));
#49252=CARTESIAN_POINT('',(-0.01350000000001,-0.0417737743898622,-0.0115985030173584));
#49253=CARTESIAN_POINT('Origin',(-0.0135,-0.0417737743898722,-0.0115985030173684));
#49254=CARTESIAN_POINT('',(-0.01350000000001,-0.0417737743898622,-0.0127532035557577));
#49255=CARTESIAN_POINT('Origin',(-0.0135,-0.0417737743898722,-0.0127532035557477));
#49256=CARTESIAN_POINT('',(-0.01249999999999,-0.0417737743898622,-0.0133305538249473));
#49257=CARTESIAN_POINT('Origin',(-0.0125,-0.0417737743898722,-0.0133305538249373));
#49258=CARTESIAN_POINT('',(0.,0.,0.));
#49259=CARTESIAN_POINT('Origin',(-0.0205477808086712,-0.0363249115320537,
0.0038241467581455));
#49260=CARTESIAN_POINT('',(-0.0204175446754309,-0.0355863057172927,0.00382414675814549));
#49261=CARTESIAN_POINT('Origin',(-0.0205477808086811,-0.0363249115320519,
0.0038241467581555));
#49262=CARTESIAN_POINT('Origin',(-0.00676047226650036,-0.0387559860193906,
0.000824146758145397));
#49263=CARTESIAN_POINT('',(-0.00663023613325018,-0.0380173802046314,-0.00217585328655808));
#49264=CARTESIAN_POINT('Origin',(-0.00676047226651023,-0.0387559860193889,
-0.00217585328654808));
#49265=CARTESIAN_POINT('',(-0.00663023613325016,-0.0380173802046314,0.000824146758165397));
#49266=CARTESIAN_POINT('',(-0.00663023613325016,-0.0380173802046314,0.000824146758145397));
#49267=CARTESIAN_POINT('',(-0.0074990780812792,-0.0386257498861369,0.000824146758145402));
#49268=CARTESIAN_POINT('Origin',(-0.00676047226651021,-0.0387559860193889,
0.000824146758155397));
#49269=CARTESIAN_POINT('Origin',(-0.00676047226651021,-0.0387559860193889,
0.000824146758155397));
#49270=CARTESIAN_POINT('Origin',(-0.00971489552553699,-0.0382350414863898,
0.000824146758145418));
#49271=CARTESIAN_POINT('',(-0.00971489552554682,-0.0382350414863881,0.00307414675814542));
#49272=CARTESIAN_POINT('Origin',(-0.00971489552553699,-0.0382350414863898,
0.000824146758145418));
#49273=CARTESIAN_POINT('',(-0.00958465939229661,-0.0374964356716289,0.00382414675814542));
#49274=CARTESIAN_POINT('Origin',(-0.00971489552554682,-0.0382350414863881,
0.00382414675815542));
#49275=CARTESIAN_POINT('Origin',(-0.00971489552554682,-0.0382350414863881,
0.00382414675815542));
#49276=CARTESIAN_POINT('Origin',(-0.0244870118207201,-0.0356303188213859,
0.00382414675814552));
#49277=CARTESIAN_POINT('',(-0.0243567756874699,-0.0348917130066267,0.00382414675814552));
#49278=CARTESIAN_POINT('Origin',(-0.00676047226650038,-0.0387559860193906,
-0.00217585328655808));
#49279=CARTESIAN_POINT('',(0.,0.,0.));
#49280=CARTESIAN_POINT('Origin',(0.00621130913087035,-0.035075620496354,
-0.0013758532865581));
#49281=CARTESIAN_POINT('',(0.00610565456543517,-0.0353021974431132,-0.0043758532865581));
#49282=CARTESIAN_POINT('Origin',(0.00621130913087458,-0.035075620496345,
-0.0043758532865481));
#49283=CARTESIAN_POINT('',(0.00610565456543517,-0.0353021974431132,-0.0013758532865381));
#49284=CARTESIAN_POINT('',(0.00610565456543517,-0.0353021974431132,-0.0013758532865581));
#49285=CARTESIAN_POINT('',(0.00598473218410215,-0.0349699659309146,-0.0013758532865581));
#49286=CARTESIAN_POINT('Origin',(0.00621130913087458,-0.035075620496345,
-0.0013758532865481));
#49287=CARTESIAN_POINT('Origin',(0.00621130913087458,-0.035075620496345,
-0.0013758532865481));
#49288=CARTESIAN_POINT('Origin',(0.00349238576976041,-0.0338077657111319,
-0.0013758532865581));
#49289=CARTESIAN_POINT('',(0.00349238576975134,-0.0338077657111277,0.0013741467134419));
#49290=CARTESIAN_POINT('Origin',(0.00349238576976041,-0.0338077657111319,
-0.0013758532865581));
#49291=CARTESIAN_POINT('',(0.00338673120431614,-0.0340343426578869,0.0016241467134419));
#49292=CARTESIAN_POINT('Origin',(0.00349238576975557,-0.0338077657111186,
0.0016241467134519));
#49293=CARTESIAN_POINT('Origin',(0.00349238576975557,-0.0338077657111186,
0.0016241467134519));
#49294=CARTESIAN_POINT('Origin',(-0.0101022310357893,-0.0274684917850214,
0.00162414671344191));
#49295=CARTESIAN_POINT('',(-0.0102078856012336,-0.0276950687317763,0.00162414671344191));
#49296=CARTESIAN_POINT('',(-0.0102078856012245,-0.0276950687317806,0.00162414671344191));
#49297=CARTESIAN_POINT('Origin',(-0.0101022310357941,-0.027468491785008,
0.00162414671345191));
#49298=CARTESIAN_POINT('Origin',(0.00621130913087035,-0.035075620496354,
-0.0043758532865581));
#49299=CARTESIAN_POINT('Origin',(-0.0101022310357893,-0.0274684917850214,
0.00162414671344191));
#49300=CARTESIAN_POINT('',(0.,0.,0.));
#49301=CARTESIAN_POINT('Origin',(0.,0.0135212256101277,-0.0121758532865581));
#49302=CARTESIAN_POINT('',(-0.00444207914276344,0.0140214195594295,-0.0121760606789385));
#49303=CARTESIAN_POINT('',(-0.00444199985070438,0.0138962255208211,-0.0121770049558098));
#49304=CARTESIAN_POINT('',(-0.004442,0.0135212256101277,-0.0121758532865581));
#49305=CARTESIAN_POINT('',(0.00444199999990267,0.0135213203764857,-0.0121758826923265));
#49306=CARTESIAN_POINT('Ctrl Pts',(-0.00444199963579549,0.0140212256101377,
-0.01217765206189));
#49307=CARTESIAN_POINT('Ctrl Pts',(-0.00444169691062519,0.0139944421724318,
-0.0129252190717282));
#49308=CARTESIAN_POINT('Ctrl Pts',(-0.00424834946874033,0.0139676587347259,
-0.0136731455972233));
#49309=CARTESIAN_POINT('Ctrl Pts',(-0.00388623378020746,0.0139408752970199,
-0.0143272600369367));
#49310=CARTESIAN_POINT('Ctrl Pts',(-0.0036851172893592,0.0139259999652549,
-0.0146905505678201));
#49311=CARTESIAN_POINT('Ctrl Pts',(-0.00343290851149104,0.0139111246334898,
-0.0150250580165878));
#49312=CARTESIAN_POINT('Ctrl Pts',(-0.00314001943231033,0.0138962493017247,
-0.0153177702117351));
#49313=CARTESIAN_POINT('Ctrl Pts',(-0.00262238939480316,0.0138699597638524,
-0.0158350876377611));
#49314=CARTESIAN_POINT('Ctrl Pts',(-0.00197179931976566,0.0138436702259802,
-0.016223435502831));
#49315=CARTESIAN_POINT('Ctrl Pts',(-0.00126781229392693,0.0138173806881079,
-0.0164330843100483));
#49316=CARTESIAN_POINT('Ctrl Pts',(-0.000856251630700209,0.0138020114565092,
-0.0165556479354792));
#49317=CARTESIAN_POINT('Ctrl Pts',(-0.000427119037945985,0.0137866422249104,
-0.0166179384412321));
#49318=CARTESIAN_POINT('Ctrl Pts',(8.84684800475695E-7,0.0137712729933117,
-0.0166178531984596));
#49319=CARTESIAN_POINT('Ctrl Pts',(0.000732998063814579,0.0137449834554394,
-0.0166177073881058));
#49320=CARTESIAN_POINT('Ctrl Pts',(0.00146774307875059,0.0137186939175672,
-0.0164322051299338));
#49321=CARTESIAN_POINT('Ctrl Pts',(0.00211372343292607,0.0136924043796949,
-0.0160827110071693));
#49322=CARTESIAN_POINT('Ctrl Pts',(0.0024913725844557,0.0136770351480962,
-0.0158783918540039));
#49323=CARTESIAN_POINT('Ctrl Pts',(0.00283877742384937,0.0136616659164974,
-0.0156190707264348));
#49324=CARTESIAN_POINT('Ctrl Pts',(0.00314127069427827,0.0136462966848987,
-0.0153165192072298));
#49325=CARTESIAN_POINT('Ctrl Pts',(0.00366841543882451,0.0136195132471928,
-0.0147892729545205));
#49326=CARTESIAN_POINT('Ctrl Pts',(0.00406108394339532,0.0135927298094869,
-0.0141249068751873));
#49327=CARTESIAN_POINT('Ctrl Pts',(0.00426828489609652,0.0135659463717809,
-0.0134059378550957));
#49328=CARTESIAN_POINT('Ctrl Pts',(0.00438336283893988,0.0135510710400159,
-0.0130066275492229));
#49329=CARTESIAN_POINT('Ctrl Pts',(0.00444199725134734,0.0135361957082508,
-0.0125910761533599));
#49330=CARTESIAN_POINT('Ctrl Pts',(0.00444199999990267,0.0135213203764857,
-0.0121758826923265));
#49331=CARTESIAN_POINT('',(0.00314096832203065,0.0135212256101277,-0.0153168216085888));
#49332=CARTESIAN_POINT('Origin',(0.,0.0135212256101277,-0.0121758532865581));
#49333=CARTESIAN_POINT('Ctrl Pts',(0.00314096832203065,0.0135212256101277,
-0.0153168216085887));
#49334=CARTESIAN_POINT('Ctrl Pts',(0.00252430835006519,0.0135524756101285,
-0.0159334815805542));
#49335=CARTESIAN_POINT('Ctrl Pts',(0.000918657482604838,0.0136149756101302,
-0.0167914720831634));
#49336=CARTESIAN_POINT('Ctrl Pts',(-0.00180052581929913,0.0137087256101327,
-0.0165242980061952));
#49337=CARTESIAN_POINT('Ctrl Pts',(-0.00391264718618217,0.013802475580363,
-0.0147910125690047));
#49338=CARTESIAN_POINT('Ctrl Pts',(-0.00444177373170171,0.0138649755505925,
-0.0130490929893534));
#49339=CARTESIAN_POINT('Ctrl Pts',(-0.00444199985070438,0.0138962255208211,
-0.0121770049558098));
#49340=CARTESIAN_POINT('Origin',(0.,0.0118503152635658,-0.0121758532865581));
#49341=CARTESIAN_POINT('',(-0.000351540290533838,0.0143316213495927,-0.0160318620293038));
#49342=CARTESIAN_POINT('',(-0.000351540291350108,0.0141148214918298,-0.0160318620292294));
#49343=CARTESIAN_POINT('',(-0.000351540291350108,0.0118503152635658,-0.0160318620292294));
#49344=CARTESIAN_POINT('',(-0.00387240384587368,0.013567201943267,-0.0121762315324215));
#49345=CARTESIAN_POINT('Ctrl Pts',(-0.000351540290533835,0.0143316213495927,
-0.0160318620293038));
#49346=CARTESIAN_POINT('Ctrl Pts',(-0.000234595974335966,0.0143267909932129,
-0.0160425234778728));
#49347=CARTESIAN_POINT('Ctrl Pts',(-0.000117241700454775,0.0143219606368333,
-0.0160478536951273));
#49348=CARTESIAN_POINT('Ctrl Pts',(1.34925462922058E-8,0.0143171302804535,
-0.0160478532865346));
#49349=CARTESIAN_POINT('Ctrl Pts',(0.000662756442570941,0.0142898284223879,
-0.0160478509771105));
#49350=CARTESIAN_POINT('Ctrl Pts',(0.00132773602328349,0.0142625265643224,
-0.0158733453024538));
#49351=CARTESIAN_POINT('Ctrl Pts',(0.00190636873638902,0.0142352247062569,
-0.01554603759026));
#49352=CARTESIAN_POINT('Ctrl Pts',(0.00221076076499003,0.0142208624557775,
-0.0153738560729781));
#49353=CARTESIAN_POINT('Ctrl Pts',(0.002491395206892,0.0142065002052982,
-0.0151602947490979));
#49354=CARTESIAN_POINT('Ctrl Pts',(0.00273792720729818,0.0141921379548189,
-0.0149137609927338));
#49355=CARTESIAN_POINT('Ctrl Pts',(0.00320648315722661,0.0141648412229327,
-0.0144452017054515));
#49356=CARTESIAN_POINT('Ctrl Pts',(0.00355326033299318,0.0141375444910466,
-0.0138517103965861));
#49357=CARTESIAN_POINT('Ctrl Pts',(0.00373099531145518,0.0141102477591604,
-0.0132112556170072));
#49358=CARTESIAN_POINT('Ctrl Pts',(0.00382454443637019,0.0140958803825017,
-0.0128741583011288));
#49359=CARTESIAN_POINT('Ctrl Pts',(0.00387200126873256,0.014081513005843,
-0.0125245939908508));
#49360=CARTESIAN_POINT('Ctrl Pts',(0.00387199999997438,0.0140671456291843,
-0.0121758392003525));
#49361=CARTESIAN_POINT('Ctrl Pts',(0.0038719975894472,0.0140398488972981,
-0.0115132362606235));
#49362=CARTESIAN_POINT('Ctrl Pts',(0.00369756338123366,0.0140125521654119,
-0.0108483757539588));
#49363=CARTESIAN_POINT('Ctrl Pts',(0.00337037109597679,0.0139852554335258,
-0.0102698148096631));
#49364=CARTESIAN_POINT('Ctrl Pts',(0.00319815653118179,0.0139708880568671,
-0.00996529472860113));
#49365=CARTESIAN_POINT('Ctrl Pts',(0.00298452907348282,0.0139565206802084,
-0.00968454561436105));
#49366=CARTESIAN_POINT('Ctrl Pts',(0.00273790728639367,0.0139421533035497,
-0.00943792565948093));
#49367=CARTESIAN_POINT('Ctrl Pts',(0.00226925993434475,0.0139148514454841,
-0.00896928178911916));
#49368=CARTESIAN_POINT('Ctrl Pts',(0.00167564221543866,0.0138875495874186,
-0.00862246838979723));
#49369=CARTESIAN_POINT('Ctrl Pts',(0.00103505110354679,0.013860247729353,
-0.00844476052262867));
#49370=CARTESIAN_POINT('Ctrl Pts',(0.000698065614071849,0.0138458854788737,
-0.0083512765958466));
#49371=CARTESIAN_POINT('Ctrl Pts',(0.000348623871723006,0.0138315232283944,
-0.00830385196479697));
#49372=CARTESIAN_POINT('Ctrl Pts',(-1.46798648791328E-8,0.0138171609779151,
-0.00830385328658593));
#49373=CARTESIAN_POINT('Ctrl Pts',(-0.000660315171071245,0.0137899597375385,
-0.00830385578997487));
#49374=CARTESIAN_POINT('Ctrl Pts',(-0.00132303731134038,0.0137627584971618,
-0.00847711421478658));
#49375=CARTESIAN_POINT('Ctrl Pts',(-0.00190015089531529,0.0137355572567851,
-0.008802159380017));
#49376=CARTESIAN_POINT('Ctrl Pts',(-0.00220700152299049,0.0137210943886169,
-0.00897498551986764));
#49377=CARTESIAN_POINT('Ctrl Pts',(-0.00248978451650191,0.0137066315204487,
-0.00918980096997239));
#49378=CARTESIAN_POINT('Ctrl Pts',(-0.00273792804685609,0.0136921686522805,
-0.00943794641994652));
#49379=CARTESIAN_POINT('Ctrl Pts',(-0.0032133888562143,0.0136644567591069,
-0.00991341090743431));
#49380=CARTESIAN_POINT('Ctrl Pts',(-0.00356314378027725,0.0136367448659333,
-0.0105169991745023));
#49381=CARTESIAN_POINT('Ctrl Pts',(-0.00373869397446481,0.0136090329727596,
-0.0111686038808494));
#49382=CARTESIAN_POINT('Ctrl Pts',(-0.00382707773856266,0.0135950809435961,
-0.0114966654755253));
#49383=CARTESIAN_POINT('Ctrl Pts',(-0.00387200014747813,0.0135811289144327,
-0.0118364022358235));
#49384=CARTESIAN_POINT('Ctrl Pts',(-0.00387199999999964,0.0135671768852691,
-0.0121758549687856));
#49385=CARTESIAN_POINT('',(-0.003716429273515,0.0135218273791635,-0.0132634579329233));
#49386=CARTESIAN_POINT('Ctrl Pts',(-0.00387199984773757,0.0135691082707264,
-0.0121769391595942));
#49387=CARTESIAN_POINT('Ctrl Pts',(-0.00387189688840871,0.013553594427274,
-0.012544070944243));
#49388=CARTESIAN_POINT('Ctrl Pts',(-0.00381923731567736,0.013537090597348,
-0.0129110808850903));
#49389=CARTESIAN_POINT('Ctrl Pts',(-0.00371613325532325,0.013521920367515,
-0.0132633907013998));
#49390=CARTESIAN_POINT('',(-0.001845911937833,0.0135212256101277,-0.00877217981253542));
#49391=CARTESIAN_POINT('Origin',(0.,0.0135212256101277,-0.0121758532865581));
#49392=CARTESIAN_POINT('Ctrl Pts',(-0.00184591193783652,0.0135212256101277,
-0.00877217981253733));
#49393=CARTESIAN_POINT('Ctrl Pts',(-0.00124967671895911,0.0135491075912296,
-0.00844882396871596));
#49394=CARTESIAN_POINT('Ctrl Pts',(-0.000566623170632383,0.0135769895723315,
-0.0082859973652041));
#49395=CARTESIAN_POINT('Ctrl Pts',(0.000273039296966733,0.0136115349745585,
-0.00831009505947237));
#49396=CARTESIAN_POINT('Ctrl Pts',(0.000434650783267868,0.0136181983956836,
-0.00832492201216256));
#49397=CARTESIAN_POINT('Ctrl Pts',(0.00125539759212987,0.0136523856215694,
-0.00845247702085292));
#49398=CARTESIAN_POINT('Ctrl Pts',(0.00189000029279552,0.0136799094263301,
-0.00873076549636361));
#49399=CARTESIAN_POINT('Ctrl Pts',(0.00254715434705814,0.0137144548285571,
-0.00925462620708204));
#49400=CARTESIAN_POINT('Ctrl Pts',(0.00267361409669593,0.0137214764260234,
-0.0093699152669625));
#49401=CARTESIAN_POINT('Ctrl Pts',(0.00325663696424368,0.0137561008155063,
-0.00997661268728381));
#49402=CARTESIAN_POINT('Ctrl Pts',(0.00359322573364207,0.0137837036075229,
-0.0105846386258012));
#49403=CARTESIAN_POINT('Ctrl Pts',(0.00379719867837587,0.0138182490097499,
-0.0113998457298512));
#49404=CARTESIAN_POINT('Ctrl Pts',(0.00382743978479439,0.0138251916199603,
-0.0115663016482717));
#49405=CARTESIAN_POINT('Ctrl Pts',(0.00392323031147953,0.0138597271111741,
-0.0124000735232294));
#49406=CARTESIAN_POINT('Ctrl Pts',(0.00382254929095312,0.0138873199921774,
-0.0130874600833825));
#49407=CARTESIAN_POINT('Ctrl Pts',(0.00349085943066387,0.0139218653944044,
-0.0138595656610514));
#49408=CARTESIAN_POINT('Ctrl Pts',(0.00341393321808629,0.0139288179156281,
-0.0140105164085618));
#49409=CARTESIAN_POINT('Ctrl Pts',(0.0029846834402559,0.0139633633178551,
-0.0147319556112248));
#49410=CARTESIAN_POINT('Ctrl Pts',(0.00248800000162184,0.0139909561988584,
-0.0152176908676159));
#49411=CARTESIAN_POINT('Ctrl Pts',(0.00175621105354843,0.0140255016010854,
-0.0156308077414003));
#49412=CARTESIAN_POINT('Ctrl Pts',(0.00160353389092322,0.0140324541223091,
-0.0157042536173573));
#49413=CARTESIAN_POINT('Ctrl Pts',(0.000880174584334333,0.0140645449262985,
-0.0159956525091302));
#49414=CARTESIAN_POINT('Ctrl Pts',(0.000257583798528075,0.0140896832090642,
-0.0160873939728307));
#49415=CARTESIAN_POINT('Ctrl Pts',(-0.000351540291350107,0.0141148214918298,
-0.0160318620292294));
#49416=CARTESIAN_POINT('Origin',(0.,0.0118503152635658,-0.0121758532865581));
#49417=CARTESIAN_POINT('',(-0.0038721948279186,0.0143506728583483,-0.0121769419744163));
#49418=CARTESIAN_POINT('Ctrl Pts',(-0.000351540291350108,0.0141148214918298,
-0.0160318620292294));
#49419=CARTESIAN_POINT('Ctrl Pts',(-0.000579483589373538,0.0141242286112912,
-0.0160110811496345));
#49420=CARTESIAN_POINT('Ctrl Pts',(-0.000805485184122002,0.0141336357307525,
-0.0159700381770124));
#49421=CARTESIAN_POINT('Ctrl Pts',(-0.00102592211344818,0.0141430428502138,
-0.0159094665253843));
#49422=CARTESIAN_POINT('Ctrl Pts',(-0.00167088713486345,0.0141705666549745,
-0.0157322430596569));
#49423=CARTESIAN_POINT('Ctrl Pts',(-0.00226971427169042,0.0141980904597352,
-0.0153835001696018));
#49424=CARTESIAN_POINT('Ctrl Pts',(-0.00274234814416526,0.0142256142644959,
-0.0149093328742253));
#49425=CARTESIAN_POINT('Ctrl Pts',(-0.00286292176508331,0.0142326358619622,
-0.0147883680618112));
#49426=CARTESIAN_POINT('Ctrl Pts',(-0.00297542408952281,0.0142396574594285,
-0.0146594671455982));
#49427=CARTESIAN_POINT('Ctrl Pts',(-0.00307887154314382,0.0142466790568948,
-0.0145238170896903));
#49428=CARTESIAN_POINT('Ctrl Pts',(-0.00348964985403048,0.0142745610379969,
-0.0139851658335498));
#49429=CARTESIAN_POINT('Ctrl Pts',(-0.0037560121468941,0.0143024430190989,
-0.0133356522401737));
#49430=CARTESIAN_POINT('Ctrl Pts',(-0.00384129369772598,0.014330325000201,
-0.0126625222991433));
#49431=CARTESIAN_POINT('Ctrl Pts',(-0.0038616748494561,0.0143369884213259,
-0.0125016532327578));
#49432=CARTESIAN_POINT('Ctrl Pts',(-0.0038719340412436,0.0143436518424509,
-0.0123395196245888));
#49433=CARTESIAN_POINT('Ctrl Pts',(-0.00387199968253043,0.0143503152635758,
-0.012177421242004));
#49434=CARTESIAN_POINT('',(0.00380878994044106,0.0148791457076089,-0.0128757686928533));
#49435=CARTESIAN_POINT('Ctrl Pts',(-0.0038719999999991,0.0143503793522163,
-0.0121758559200756));
#49436=CARTESIAN_POINT('Ctrl Pts',(-0.00387200045770963,0.0143780325348381,
-0.01150289470167));
#49437=CARTESIAN_POINT('Ctrl Pts',(-0.00369222349743829,0.01440568571746,
-0.0108293876420033));
#49438=CARTESIAN_POINT('Ctrl Pts',(-0.00335670115622441,0.0144333389000819,
-0.0102458425747221));
#49439=CARTESIAN_POINT('Ctrl Pts',(-0.00315760406319418,0.0144497481450018,
-0.00989957017411986));
#49440=CARTESIAN_POINT('Ctrl Pts',(-0.00290472696423594,0.0144661573899216,
-0.00958484115308815));
#49441=CARTESIAN_POINT('Ctrl Pts',(-0.00261081926799486,0.0144825666348415,
-0.0093164815461461));
#49442=CARTESIAN_POINT('Ctrl Pts',(-0.00212574766486381,0.0145096488066976,
-0.00887357506081123));
#49443=CARTESIAN_POINT('Ctrl Pts',(-0.00152261847466415,0.0145367309785537,
-0.00855513870295691));
#49444=CARTESIAN_POINT('Ctrl Pts',(-0.000879918305563984,0.0145638131504098,
-0.00840516001137203));
#49445=CARTESIAN_POINT('Ctrl Pts',(-0.000476945286284811,0.014580793672722,
-0.00831112336865555));
#49446=CARTESIAN_POINT('Ctrl Pts',(-5.91672300722142E-5,0.0145977741950343,
-0.00828244179970653));
#49447=CARTESIAN_POINT('Ctrl Pts',(0.000351165990502362,0.0146147547173465,
-0.00831981043836327));
#49448=CARTESIAN_POINT('Ctrl Pts',(0.00100560491726355,0.0146418368892026,
-0.00837940954111882));
#49449=CARTESIAN_POINT('Ctrl Pts',(0.00164751455549754,0.0146689190610587,
-0.00861024688705076));
#49450=CARTESIAN_POINT('Ctrl Pts',(0.00219154154443199,0.0146960012329149,
-0.00898374901836311));
#49451=CARTESIAN_POINT('Ctrl Pts',(0.0025326464777122,0.0147129817552271,
-0.00921793486239789));
#49452=CARTESIAN_POINT('Ctrl Pts',(0.00283541353171744,0.0147299622775394,
-0.00950706446100596));
#49453=CARTESIAN_POINT('Ctrl Pts',(0.00308438600525397,0.0147469427998516,
-0.00983513823115442));
#49454=CARTESIAN_POINT('Ctrl Pts',(0.00348984360037339,0.0147745959843294,
-0.0103694141692799));
#49455=CARTESIAN_POINT('Ctrl Pts',(0.00375432056697956,0.0148022491688071,
-0.0110133833702221));
#49456=CARTESIAN_POINT('Ctrl Pts',(0.0038403218868933,0.0148299023532849,
-0.0116815742104804));
#49457=CARTESIAN_POINT('Ctrl Pts',(0.00389135541229657,0.0148463118629755,
-0.0120780813135661));
#49458=CARTESIAN_POINT('Ctrl Pts',(0.00388043750613101,0.0148627213726661,
-0.0124825444984827));
#49459=CARTESIAN_POINT('Ctrl Pts',(0.00380829892483911,0.0148791308823567,
-0.0128753125770599));
#49460=CARTESIAN_POINT('',(0.00147252214094898,0.0148792256101277,-0.0085947832587012));
#49461=CARTESIAN_POINT('Origin',(0.,0.0148792256101377,-0.0121758532865581));
#49462=CARTESIAN_POINT('',(-0.00387344021111285,0.0145664623429172,-0.012175597920995));
#49463=CARTESIAN_POINT('Ctrl Pts',(0.0014725221409559,0.0148792256101304,
-0.00859478325869949));
#49464=CARTESIAN_POINT('Ctrl Pts',(0.000887378242150321,0.0148532194115101,
-0.00835417514568843));
#49465=CARTESIAN_POINT('Ctrl Pts',(0.000242176794320239,0.0148310402855,
-0.00826224698544157));
#49466=CARTESIAN_POINT('Ctrl Pts',(-0.00038679968741254,0.0148044058086255,
-0.00832508349183273));
#49467=CARTESIAN_POINT('Ctrl Pts',(-0.000994091281060047,0.0147786895944635,
-0.0083857536173681));
#49468=CARTESIAN_POINT('Ctrl Pts',(-0.00158890100584688,0.0147498679363824,
-0.00858900078255042));
#49469=CARTESIAN_POINT('Ctrl Pts',(-0.00210175235193759,0.0147243548334753,
-0.00892093623646652));
#49470=CARTESIAN_POINT('Ctrl Pts',(-0.00212006501122793,0.0147234438233658,
-0.00893278883453473));
#49471=CARTESIAN_POINT('Ctrl Pts',(-0.00213827499674151,0.0147225370317578,
-0.00894480592354508));
#49472=CARTESIAN_POINT('Ctrl Pts',(-0.00215638108303436,0.0147216347506687,
-0.00895698443036752));
#49473=CARTESIAN_POINT('Ctrl Pts',(-0.00268155337858154,0.0146954638254269,
-0.00931022556049541));
#49474=CARTESIAN_POINT('Ctrl Pts',(-0.00311665188306085,0.0146740956855631,
-0.00979568174368227));
#49475=CARTESIAN_POINT('Ctrl Pts',(-0.00341452495792785,0.0146477578505066,
-0.0103532822316314));
#49476=CARTESIAN_POINT('Ctrl Pts',(-0.00369210313818325,0.0146232144830668,
-0.0108728918970016));
#49477=CARTESIAN_POINT('Ctrl Pts',(-0.00385395922200843,0.0145957954793885,
-0.0114565046869531));
#49478=CARTESIAN_POINT('Ctrl Pts',(-0.00387330707293454,0.0145710179582555,
-0.012045887858781));
#49479=CARTESIAN_POINT('Ctrl Pts',(-0.00387472167474202,0.0145692063706888,
-0.0120889801124556));
#49480=CARTESIAN_POINT('Ctrl Pts',(-0.00387537557451555,0.0145674089036423,
-0.012132109253815));
#49481=CARTESIAN_POINT('Ctrl Pts',(-0.00387528217137323,0.0145656277134538,
-0.0121752548237611));
#49482=CARTESIAN_POINT('Ctrl Pts',(-0.00387199999997852,0.0145671149317227,
-0.0121758661854451));
#49483=CARTESIAN_POINT('Ctrl Pts',(-0.00387199775389951,0.0145394030373481,
-0.0128500962879766));
#49484=CARTESIAN_POINT('Ctrl Pts',(-0.0036915722611453,0.0145116911429736,
-0.0135246572134559));
#49485=CARTESIAN_POINT('Ctrl Pts',(-0.00318550729473349,0.0144700270344287,
-0.0144029950422947));
#49486=CARTESIAN_POINT('Ctrl Pts',(-0.00297729196260053,0.0144560748202584,
-0.0146743978690617));
#49487=CARTESIAN_POINT('Ctrl Pts',(-0.00227184049541597,0.0144149583852686,
-0.0153798445279271));
#49488=CARTESIAN_POINT('Ctrl Pts',(-0.00168184678885426,0.0143877941644492,
-0.0157257004608036));
#49489=CARTESIAN_POINT('Ctrl Pts',(-0.000818093438899106,0.0143509604122953,
-0.0159677606078325));
#49490=CARTESIAN_POINT('Ctrl Pts',(-0.000585642423977778,0.0143412908809608,
-0.0160105196678911));
#49491=CARTESIAN_POINT('Ctrl Pts',(-0.000351540291350112,0.0143316213496264,
-0.0160318620292294));
#49492=CARTESIAN_POINT('Origin',(0.,0.0135212256101277,-0.0121758532865581));
#49493=CARTESIAN_POINT('',(-0.00441705924701761,0.0148779965858899,-0.0126490161932378));
#49494=CARTESIAN_POINT('Ctrl Pts',(-0.00444199982066862,0.0138992441597151,
-0.0121771154988945));
#49495=CARTESIAN_POINT('Ctrl Pts',(-0.00444202564285501,0.0139026434699815,
-0.0120862416070427));
#49496=CARTESIAN_POINT('Ctrl Pts',(-0.00443926284757712,0.0139059652244875,
-0.0119953857450405));
#49497=CARTESIAN_POINT('Ctrl Pts',(-0.00442784020811473,0.0139126423178769,
-0.0118086274885908));
#49498=CARTESIAN_POINT('Ctrl Pts',(-0.00441884605653583,0.0139159862346956,
-0.011712793506025));
#49499=CARTESIAN_POINT('Ctrl Pts',(-0.00436012104913382,0.0139318211304826,
-0.0112494584350861));
#49500=CARTESIAN_POINT('Ctrl Pts',(-0.00426762388218305,0.0139429719947748,
-0.0108889008820107));
#49501=CARTESIAN_POINT('Ctrl Pts',(-0.00408183008368174,0.0139587528637333,
-0.0104185152039224));
#49502=CARTESIAN_POINT('Ctrl Pts',(-0.00402656448691405,0.0139630294214672,
-0.0102953347732247));
#49503=CARTESIAN_POINT('Ctrl Pts',(-0.0039190876339132,0.0139709582836448,
-0.0100823251324102));
#49504=CARTESIAN_POINT('Ctrl Pts',(-0.00386917138242235,0.0139745238664448,
-0.00999144956897392));
#49505=CARTESIAN_POINT('Ctrl Pts',(-0.0037589689820606,0.0139823260620285,
-0.00980646792407794));
#49506=CARTESIAN_POINT('Ctrl Pts',(-0.00369821953128187,0.0139865846864293,
-0.00971272431953164));
#49507=CARTESIAN_POINT('Ctrl Pts',(-0.00345694603367115,0.014003057015773,
-0.00936948810311859));
#49508=CARTESIAN_POINT('Ctrl Pts',(-0.00325417807693909,0.014015993488214,
-0.00913669352427505));
#49509=CARTESIAN_POINT('Ctrl Pts',(-0.00286690602984965,0.0140373522192455,
-0.00877566206955802));
#49510=CARTESIAN_POINT('Ctrl Pts',(-0.00269376401373504,0.0140460078826927,
-0.00863691273066231));
#49511=CARTESIAN_POINT('Ctrl Pts',(-0.00238734867400198,0.0140597165348944,
-0.0084269345529207));
#49512=CARTESIAN_POINT('Ctrl Pts',(-0.00225950732541166,0.0140650257412601,
-0.00834852307781464));
#49513=CARTESIAN_POINT('Ctrl Pts',(-0.00180398266701824,0.0140826920725418,
-0.00809992200172164));
#49514=CARTESIAN_POINT('Ctrl Pts',(-0.00145927492313164,0.0140937984255215,
-0.00796419217128511));
#49515=CARTESIAN_POINT('Ctrl Pts',(-0.000957875691113172,0.0141097294880842,
-0.00783581957683498));
#49516=CARTESIAN_POINT('Ctrl Pts',(-0.00081225663396107,0.0141143537888474,
-0.00780622462977062));
#49517=CARTESIAN_POINT('Ctrl Pts',(-0.000557372889022838,0.0141227966525157,
-0.00776760590496824));
#49518=CARTESIAN_POINT('Ctrl Pts',(-0.000448748702513778,0.0141265036555715,
-0.00775522758600577));
#49519=CARTESIAN_POINT('Ctrl Pts',(-0.000240635274618488,0.0141339827762971,
-0.00773926144347405));
#49520=CARTESIAN_POINT('Ctrl Pts',(-0.00014126741769445,0.0141377235338807,
-0.00773498711422376));
#49521=CARTESIAN_POINT('Ctrl Pts',(0.000306994394699704,0.0141551135397262,
-0.00773076373155874));
#49522=CARTESIAN_POINT('Ctrl Pts',(0.000655010087065435,0.0141699083735277,
-0.00776858196043291));
#49523=CARTESIAN_POINT('Ctrl Pts',(0.00120088270129325,0.0141924504912556,
-0.00789404729244587));
#49524=CARTESIAN_POINT('Ctrl Pts',(0.0014031188511572,0.0142006717415967,
-0.00795598930669396));
#49525=CARTESIAN_POINT('Ctrl Pts',(0.0017389154139472,0.0142139322248016,
-0.00808566373784058));
#49526=CARTESIAN_POINT('Ctrl Pts',(0.00187486434873533,0.0142191892410764,
-0.00814616775676237));
#49527=CARTESIAN_POINT('Ctrl Pts',(0.00224729365688353,0.0142333740904071,
-0.00833485374749599));
#49528=CARTESIAN_POINT('Ctrl Pts',(0.00247554526504795,0.0142417772933865,
-0.00847784133140785));
#49529=CARTESIAN_POINT('Ctrl Pts',(0.00290080912554325,0.0142581730502546,
-0.00880136355572665));
#49530=CARTESIAN_POINT('Ctrl Pts',(0.00309728882477237,0.014266149521508,
-0.00898075391918834));
#49531=CARTESIAN_POINT('Ctrl Pts',(0.00334346015629937,0.0142782658930626,
-0.00924968594702028));
#49532=CARTESIAN_POINT('Ctrl Pts',(0.00340789540087553,0.0142816775959886,
-0.00932498854984708));
#49533=CARTESIAN_POINT('Ctrl Pts',(0.0035390771685509,0.0142892904191578,
-0.00948910385116271));
#49534=CARTESIAN_POINT('Ctrl Pts',(0.00360511680304918,0.0142935235954553,
-0.00957838917469358));
#49535=CARTESIAN_POINT('Ctrl Pts',(0.00384118729230714,0.0143099517519287,
-0.00992392484989375));
#49536=CARTESIAN_POINT('Ctrl Pts',(0.00398780770180776,0.0143228737041738,
-0.0101951219230348));
#49537=CARTESIAN_POINT('Ctrl Pts',(0.00416806792381943,0.0143419226672198,
-0.0106313051000987));
#49538=CARTESIAN_POINT('Ctrl Pts',(0.00422240145574149,0.0143484143021054,
-0.0107866986366084));
#49539=CARTESIAN_POINT('Ctrl Pts',(0.00431078430291874,0.0143605282374881,
-0.0110931060617778));
#49540=CARTESIAN_POINT('Ctrl Pts',(0.00434581377783233,0.0143661717611491,
-0.0112435922783342));
#49541=CARTESIAN_POINT('Ctrl Pts',(0.00440497242788833,0.0143779803658016,
-0.0115751502407589));
#49542=CARTESIAN_POINT('Ctrl Pts',(0.00442592101926712,0.0143840405180869,
-0.0117565016923853));
#49543=CARTESIAN_POINT('Ctrl Pts',(0.0044485050283149,0.0143975713436589,
-0.0121787980643437));
#49544=CARTESIAN_POINT('Ctrl Pts',(0.00444182285338998,0.0144048440842986,
-0.0124196075199902));
#49545=CARTESIAN_POINT('Ctrl Pts',(0.00439504372400568,0.0144181251602001,
-0.0128474188210095));
#49546=CARTESIAN_POINT('Ctrl Pts',(0.00436232903356552,0.0144240730846339,
-0.0130346240245222));
#49547=CARTESIAN_POINT('Ctrl Pts',(0.00429620162246521,0.0144336162605868,
-0.0133082960703997));
#49548=CARTESIAN_POINT('Ctrl Pts',(0.00427190638161057,0.0144368417064606,
-0.013396751043192));
#49549=CARTESIAN_POINT('Ctrl Pts',(0.004206342556907,0.0144450367530583,
-0.0136094390137663));
#49550=CARTESIAN_POINT('Ctrl Pts',(0.00416229188503837,0.0144501295990971,
-0.0137327116651824));
#49551=CARTESIAN_POINT('Ctrl Pts',(0.00403434800258625,0.014463667204684,
-0.0140463091881702));
#49552=CARTESIAN_POINT('Ctrl Pts',(0.00394241718416269,0.0144722938544275,
-0.0142330150455762));
#49553=CARTESIAN_POINT('Ctrl Pts',(0.00370430753313148,0.0144916471115149,
-0.0146415583246631));
#49554=CARTESIAN_POINT('Ctrl Pts',(0.00355062992283893,0.0145022380231317,
-0.0148581371018604));
#49555=CARTESIAN_POINT('Ctrl Pts',(0.00328200221519045,0.0145176958856387,
-0.0151728415838315));
#49556=CARTESIAN_POINT('Ctrl Pts',(0.00317983554487372,0.0145230350650933,
-0.0152810308739914));
#49557=CARTESIAN_POINT('Ctrl Pts',(0.00291987917654451,0.0145354483168824,
-0.0155299978923077));
#49558=CARTESIAN_POINT('Ctrl Pts',(0.00275709835575286,0.0145422831631224,
-0.0156650361916866));
#49559=CARTESIAN_POINT('Ctrl Pts',(0.00230163247088849,0.0145597961086379,
-0.0159910277457426));
#49560=CARTESIAN_POINT('Ctrl Pts',(0.00199504193389812,0.0145699609360743,
-0.0161599265322212));
#49561=CARTESIAN_POINT('Ctrl Pts',(0.00157974383068174,0.0145848500268095,
-0.0163286431974242));
#49562=CARTESIAN_POINT('Ctrl Pts',(0.00148637580315657,0.0145882723180297,
-0.0163629693617686));
#49563=CARTESIAN_POINT('Ctrl Pts',(0.0012881695489773,0.0145958323980512,
-0.0164283728988262));
#49564=CARTESIAN_POINT('Ctrl Pts',(0.00118318067977982,0.0145999960508943,
-0.016458771058935));
#49565=CARTESIAN_POINT('Ctrl Pts',(0.000933170033887146,0.01461010917163,
-0.0165212639361954));
#49566=CARTESIAN_POINT('Ctrl Pts',(0.000787445823063148,0.0146161554287245,
-0.016550019072331));
#49567=CARTESIAN_POINT('Ctrl Pts',(0.000275234332457088,0.0146373873156637,
-0.0166246630399494));
#49568=CARTESIAN_POINT('Ctrl Pts',(-9.53581726507817E-5,0.0146525639350941,
-0.0166321559733303));
#49569=CARTESIAN_POINT('Ctrl Pts',(-0.00061167697770944,0.0146719322510565,
-0.0165780886136249));
#49570=CARTESIAN_POINT('Ctrl Pts',(-0.000759850829046054,0.0146773045740417,
-0.016554946334376));
#49571=CARTESIAN_POINT('Ctrl Pts',(-0.00112358278574679,0.0146900996218849,
-0.0164791151526359));
#49572=CARTESIAN_POINT('Ctrl Pts',(-0.00133690223515231,0.0146972419957619,
-0.0164176927757886));
#49573=CARTESIAN_POINT('Ctrl Pts',(-0.00183341324129367,0.0147137641533747,
-0.0162335308955262));
#49574=CARTESIAN_POINT('Ctrl Pts',(-0.00211014030225272,0.0147228682765576,
-0.0160967510559873));
#49575=CARTESIAN_POINT('Ctrl Pts',(-0.00246486977430493,0.014736588663987,
-0.015872911145969));
#49576=CARTESIAN_POINT('Ctrl Pts',(-0.00255697215138027,0.0147403681868445,
-0.0158098195212305));
#49577=CARTESIAN_POINT('Ctrl Pts',(-0.00272988663573368,0.0147480751647543,
-0.0156815398685845));
#49578=CARTESIAN_POINT('Ctrl Pts',(-0.00281098163028683,0.0147519752446657,
-0.0156168558138115));
#49579=CARTESIAN_POINT('Ctrl Pts',(-0.00299230489974038,0.0147612267332673,
-0.0154615368153484));
#49580=CARTESIAN_POINT('Ctrl Pts',(-0.00309081359260155,0.0147666543088073,
-0.0153690450639589));
#49581=CARTESIAN_POINT('Ctrl Pts',(-0.00345781174343217,0.014788035248714,
-0.0149915465128209));
#49582=CARTESIAN_POINT('Ctrl Pts',(-0.00369241921182423,0.0148041250738692,
-0.0146759947882948));
#49583=CARTESIAN_POINT('Ctrl Pts',(-0.00395640640981797,0.0148242677548495,
-0.0142010143467172));
#49584=CARTESIAN_POINT('Ctrl Pts',(-0.00402333154541086,0.0148296748123009,
-0.0140645663290976));
#49585=CARTESIAN_POINT('Ctrl Pts',(-0.00418065875611654,0.0148433397730415,
-0.0136972973811787));
#49586=CARTESIAN_POINT('Ctrl Pts',(-0.00425897224168211,0.0148511999675334,
-0.0134618803121984));
#49587=CARTESIAN_POINT('Ctrl Pts',(-0.00436286304922231,0.0148648375902373,
-0.0130327950468715));
#49588=CARTESIAN_POINT('Ctrl Pts',(-0.004396092120752,0.0148706917529315,
-0.0128416570437104));
#49589=CARTESIAN_POINT('Ctrl Pts',(-0.00441673296289603,0.0148767675448707,
-0.012648964197939));
#49590=CARTESIAN_POINT('',(-0.00278820502685331,0.0148792256101277,-0.0156337828301188));
#49591=CARTESIAN_POINT('Origin',(0.,0.0148792256101377,-0.0121758532865581));
#49592=CARTESIAN_POINT('Ctrl Pts',(-0.00278820502685448,0.0148792256101377,
-0.0156337828301179));
#49593=CARTESIAN_POINT('Ctrl Pts',(-0.00201147069505603,0.0148434782482309,
-0.0162600808911887));
#49594=CARTESIAN_POINT('Ctrl Pts',(-2.30099782061264E-5,0.0147719835244173,
-0.0169665420603791));
#49595=CARTESIAN_POINT('Ctrl Pts',(0.00297216531875188,0.0146647414386969,
-0.015933805333576));
#49596=CARTESIAN_POINT('Ctrl Pts',(0.00466732644442066,0.0145574993529764,
-0.0132576561457133));
#49597=CARTESIAN_POINT('Ctrl Pts',(0.00432221053072379,0.014450257267256,
-0.0101086911624707));
#49598=CARTESIAN_POINT('Ctrl Pts',(0.00208747382629606,0.0143430151815356,
-0.00786346571244169));
#49599=CARTESIAN_POINT('Ctrl Pts',(-0.00105984742215624,0.0142357730958152,
-0.00750330647444095));
#49600=CARTESIAN_POINT('Ctrl Pts',(-0.0037438236759896,0.0141285312769041,
-0.00918670830698344));
#49601=CARTESIAN_POINT('Ctrl Pts',(-0.00444200032332976,0.0140570368198998,
-0.0111780827837936));
#49602=CARTESIAN_POINT('Ctrl Pts',(-0.00444199999999725,0.0140212897248023,
-0.0121758555835873));
#49603=CARTESIAN_POINT('Origin',(0.,0.0137212256101277,-0.0121758532865581));
#49604=CARTESIAN_POINT('',(-0.0025,0.0139212256101277,-0.0121758532865581));
#49605=CARTESIAN_POINT('Origin',(0.,0.0139212256101377,-0.0121758532865581));
#49606=CARTESIAN_POINT('',(-0.002900000000005,0.0135212256101227,-0.0121758532865581));
#49607=CARTESIAN_POINT('',(-0.0027,0.0137212256101277,-0.0121758532865581));
#49608=CARTESIAN_POINT('Origin',(0.,0.0135212256101277,-0.0121758532865581));
#49609=CARTESIAN_POINT('Origin',(0.,0.0135212256101277,-0.0121758532865581));
#49610=CARTESIAN_POINT('',(-0.0025,0.0151212256101377,-0.0121758532865581));
#49611=CARTESIAN_POINT('',(-0.0025,0.0135212256101277,-0.0121758532865581));
#49612=CARTESIAN_POINT('Origin',(0.,0.0151212256101377,-0.0121758532865581));
#49613=CARTESIAN_POINT('Origin',(0.,0.0135212256101277,-0.0121758532865581));
#49614=CARTESIAN_POINT('',(-0.00371483287819128,0.013521225610129,-0.0132805663438727));
#49615=CARTESIAN_POINT('Ctrl Pts',(-0.0037148328777567,0.0135212256101303,
-0.0132805663459238));
#49616=CARTESIAN_POINT('Ctrl Pts',(-0.00367676010924277,0.0135212256101305,
-0.0134593107044183));
#49617=CARTESIAN_POINT('Ctrl Pts',(-0.00362588667618153,0.0135212256101307,
-0.0136344111414368));
#49618=CARTESIAN_POINT('Ctrl Pts',(-0.00356215531751432,0.0135212256101308,
-0.0138044431938857));
#49619=CARTESIAN_POINT('Ctrl Pts',(-0.00352036300244373,0.0135212256101308,
-0.0139159429838894));
#49620=CARTESIAN_POINT('Ctrl Pts',(-0.00347303710944158,0.0135212256101309,
-0.0140252648516543));
#49621=CARTESIAN_POINT('Ctrl Pts',(-0.0034205447519999,0.0135212256101335,
-0.0141322036001223));
#49622=CARTESIAN_POINT('Ctrl Pts',(-0.00336697272343145,0.0135212256101361,
-0.0142413418817163));
#49623=CARTESIAN_POINT('Ctrl Pts',(-0.00330801916308001,0.0135212256101311,
-0.0143479986131602));
#49624=CARTESIAN_POINT('Ctrl Pts',(-0.00324402262044731,0.0135212256101344,
-0.0144519391983276));
#49625=CARTESIAN_POINT('Ctrl Pts',(-0.00320932607863089,0.0135212256101362,
-0.0145082919122607));
#49626=CARTESIAN_POINT('Ctrl Pts',(-0.00317314634461811,0.0135212256101312,
-0.0145638459036323));
#49627=CARTESIAN_POINT('Ctrl Pts',(-0.00313553181154857,0.0135212256101312,
-0.0146185608267094));
#49628=CARTESIAN_POINT('Ctrl Pts',(-0.00312568654141207,0.0135212256101312,
-0.0146328819721347));
#49629=CARTESIAN_POINT('Ctrl Pts',(-0.00311574295633818,0.0135212256101312,
-0.0146471456214485));
#49630=CARTESIAN_POINT('Ctrl Pts',(-0.00310570188433775,0.0135212256101312,
-0.0146613510227781));
#49631=CARTESIAN_POINT('Ctrl Pts',(-0.00309590668589143,0.0135212256101312,
-0.0146752085795238));
#49632=CARTESIAN_POINT('Ctrl Pts',(-0.00308602434663422,0.0135212256101312,
-0.0146890027305733));
#49633=CARTESIAN_POINT('Ctrl Pts',(-0.00307605677284421,0.0135212256101312,
-0.0147027318404865));
#49634=CARTESIAN_POINT('Ctrl Pts',(-0.00300316097838175,0.0135212256101313,
-0.0148031368533285));
#49635=CARTESIAN_POINT('Ctrl Pts',(-0.00292569704568872,0.0135212256101363,
-0.0149000838514716));
#49636=CARTESIAN_POINT('Ctrl Pts',(-0.00284407294034953,0.0135212256101338,
-0.0149933598189867));
#49637=CARTESIAN_POINT('Ctrl Pts',(-0.00276104793101491,0.0135212256101313,
-0.0150882366699054));
#49638=CARTESIAN_POINT('Ctrl Pts',(-0.00267371826719912,0.0135212256101313,
-0.0151793160423849));
#49639=CARTESIAN_POINT('Ctrl Pts',(-0.00258246178724139,0.0135212256101313,
-0.0152663540581625));
#49640=CARTESIAN_POINT('Ctrl Pts',(-0.00243774910228737,0.0135212256101313,
-0.0154043771877208));
#49641=CARTESIAN_POINT('Ctrl Pts',(-0.00228317140345813,0.0135212256101313,
-0.015532250623269));
#49642=CARTESIAN_POINT('Ctrl Pts',(-0.00212002316546883,0.0135212256101312,
-0.0156488439511656));
#49643=CARTESIAN_POINT('Ctrl Pts',(-0.00208706339792013,0.0135212256101312,
-0.0156723985358339));
#49644=CARTESIAN_POINT('Ctrl Pts',(-0.00205375312855055,0.0135212256101312,
-0.0156954919643269));
#49645=CARTESIAN_POINT('Ctrl Pts',(-0.00202010203786124,0.0135212256101312,
-0.0157181136505389));
#49646=CARTESIAN_POINT('Ctrl Pts',(-0.0020052538477559,0.0135212256101312,
-0.0157280952318338));
#49647=CARTESIAN_POINT('Ctrl Pts',(-0.00199033775336458,0.0135212256101312,
-0.0157379859714015));
#49648=CARTESIAN_POINT('Ctrl Pts',(-0.00197535945581412,0.0135212256101312,
-0.0157477817383071));
#49649=CARTESIAN_POINT('Ctrl Pts',(-0.00186683699532327,0.0135212256101312,
-0.015818755139884));
#49650=CARTESIAN_POINT('Ctrl Pts',(-0.00175538512191969,0.0135212256101362,
-0.0158845295934832));
#49651=CARTESIAN_POINT('Ctrl Pts',(-0.00164139770383617,0.0135212256101336,
-0.0159448584383389));
#49652=CARTESIAN_POINT('Ctrl Pts',(-0.00152735310373093,0.013521225610131,
-0.0160052175472831));
#49653=CARTESIAN_POINT('Ctrl Pts',(-0.00141076975051351,0.0135212256101309,
-0.0160601262200838));
#49654=CARTESIAN_POINT('Ctrl Pts',(-0.00129200332480448,0.0135212256101308,
-0.0161093027019261));
#49655=CARTESIAN_POINT('Ctrl Pts',(-0.00111285742462027,0.0135212256101308,
-0.0161834799372428));
#49656=CARTESIAN_POINT('Ctrl Pts',(-0.000928748119590978,0.0135212256101306,
-0.0162446291259923));
#49657=CARTESIAN_POINT('Ctrl Pts',(-0.000740778709230239,0.0135212256101304,
-0.0162915858099064));
#49658=CARTESIAN_POINT('Ctrl Pts',(-0.00069400337526837,0.0135212256101304,
-0.0163032707674088));
#49659=CARTESIAN_POINT('Ctrl Pts',(-0.00064698849963088,0.0135212256101304,
-0.0163140755329016));
#49660=CARTESIAN_POINT('Ctrl Pts',(-0.000599754198781191,0.0135212256101303,
-0.0163240069284197));
#49661=CARTESIAN_POINT('Ctrl Pts',(-0.000571358594604591,0.0135212256101303,
-0.0163299773349036));
#49662=CARTESIAN_POINT('Ctrl Pts',(-0.000542883685759838,0.0135212256101303,
-0.016335632085061));
#49663=CARTESIAN_POINT('Ctrl Pts',(-0.000514333811540033,0.0135212256101303,
-0.0163409724716758));
#49664=CARTESIAN_POINT('Ctrl Pts',(-0.000497614725750705,0.0135212256101302,
-0.0163440998543492));
#49665=CARTESIAN_POINT('Ctrl Pts',(-0.000480871848590969,0.0135212256101352,
-0.0163471190178022));
#49666=CARTESIAN_POINT('Ctrl Pts',(-0.000464117417771817,0.0135212256101346,
-0.0163500284533313));
#49667=CARTESIAN_POINT('Ctrl Pts',(-0.000341217338960648,0.0135212256101301,
-0.0163713702619364));
#49668=CARTESIAN_POINT('Ctrl Pts',(-0.000217529147290246,0.0135212256101298,
-0.0163868437048162));
#49669=CARTESIAN_POINT('Ctrl Pts',(-9.3428659998974E-5,0.0135212256101295,
-0.0163966664507915));
#49670=CARTESIAN_POINT('Ctrl Pts',(3.36391484278545E-5,0.0135212256101292,
-0.0164067240648353));
#49671=CARTESIAN_POINT('Ctrl Pts',(0.000161139813868302,0.0135212256101295,
-0.0164108575969878));
#49672=CARTESIAN_POINT('Ctrl Pts',(0.000288690269230646,0.0135212256101296,
-0.0164092501650054));
#49673=CARTESIAN_POINT('Ctrl Pts',(0.000532010107936883,0.0135212256101298,
-0.0164061837699105));
#49674=CARTESIAN_POINT('Ctrl Pts',(0.000775513572144928,0.0135212256101301,
-0.0163822632742277));
#49675=CARTESIAN_POINT('Ctrl Pts',(0.00101661218976315,0.0135212256101302,
-0.0163382677180292));
#49676=CARTESIAN_POINT('Ctrl Pts',(0.00104574194951984,0.0135212256101303,
-0.0163329521339122));
#49677=CARTESIAN_POINT('Ctrl Pts',(0.00107483656722365,0.0135212256101353,
-0.0163273427497234));
#49678=CARTESIAN_POINT('Ctrl Pts',(0.00110389140778561,0.0135212256101353,
-0.0163214403265222));
#49679=CARTESIAN_POINT('Ctrl Pts',(0.00112687781898231,0.0135212256101353,
-0.0163167706906153));
#49680=CARTESIAN_POINT('Ctrl Pts',(0.00114984177385114,0.0135212256101303,
-0.0163119170173606));
#49681=CARTESIAN_POINT('Ctrl Pts',(0.00117275806504747,0.0135212256101303,
-0.0163068849107322));
#49682=CARTESIAN_POINT('Ctrl Pts',(0.00130317602529154,0.0135212256101305,
-0.0162782468961171));
#49683=CARTESIAN_POINT('Ctrl Pts',(0.00143220650179616,0.0135212256101355,
-0.0162438036971463));
#49684=CARTESIAN_POINT('Ctrl Pts',(0.00155943569693481,0.0135212256101356,
-0.0162037234389758));
#49685=CARTESIAN_POINT('Ctrl Pts',(0.00168729814890097,0.0135212256101357,
-0.0161634436896657));
#49686=CARTESIAN_POINT('Ctrl Pts',(0.00181334218941698,0.0135212256101308,
-0.016117470513265));
#49687=CARTESIAN_POINT('Ctrl Pts',(0.00193714485169985,0.0135212256101309,
-0.0160659222475803));
#49688=CARTESIAN_POINT('Ctrl Pts',(0.00199197341364183,0.0135212256101309,
-0.0160430930351387));
#49689=CARTESIAN_POINT('Ctrl Pts',(0.00204636224868705,0.0135212256101359,
-0.0160191696812025));
#49690=CARTESIAN_POINT('Ctrl Pts',(0.00210027376306881,0.0135212256101328,
-0.0159941592988056));
#49691=CARTESIAN_POINT('Ctrl Pts',(0.00213093281696214,0.013521225610131,
-0.0159799360911923));
#49692=CARTESIAN_POINT('Ctrl Pts',(0.00216143748795381,0.013521225610131,
-0.0159653612919411));
#49693=CARTESIAN_POINT('Ctrl Pts',(0.00219178074621081,0.013521225610131,
-0.0159504359356592));
#49694=CARTESIAN_POINT('Ctrl Pts',(0.00221206061632124,0.013521225610131,
-0.0159404605966833));
#49695=CARTESIAN_POINT('Ctrl Pts',(0.00223225959097951,0.013521225610131,
-0.0159303329738333));
#49696=CARTESIAN_POINT('Ctrl Pts',(0.00225237355325245,0.013521225610131,
-0.0159200548931265));
#49697=CARTESIAN_POINT('Ctrl Pts',(0.00237320353572851,0.0135212256101311,
-0.0158583116972888));
#49698=CARTESIAN_POINT('Ctrl Pts',(0.00249099215410104,0.0135212256101311,
-0.0157911304018793));
#49699=CARTESIAN_POINT('Ctrl Pts',(0.00260531366703308,0.0135212256101312,
-0.0157186451039207));
#49700=CARTESIAN_POINT('Ctrl Pts',(0.00271786118642715,0.0135212256101312,
-0.015647284602572));
#49701=CARTESIAN_POINT('Ctrl Pts',(0.00282704914459482,0.0135212256101363,
-0.015570783150034));
#49702=CARTESIAN_POINT('Ctrl Pts',(0.00293245440604282,0.0135212256101363,
-0.0154892218352429));
#49703=CARTESIAN_POINT('Ctrl Pts',(0.00300373533197715,0.0135212256101363,
-0.0154340655180073));
#49704=CARTESIAN_POINT('Ctrl Pts',(0.00307328599312713,0.0135212256101313,
-0.0153765942559097));
#49705=CARTESIAN_POINT('Ctrl Pts',(0.00314096832203064,0.0135212256101277,
-0.0153168216085888));
#49706=CARTESIAN_POINT('Ctrl Pts',(0.00444614404405592,0.0135212256101274,
-0.0121732434012118));
#49707=CARTESIAN_POINT('Ctrl Pts',(0.00443886810540444,0.0135212256101255,
-0.0120407103896413));
#49708=CARTESIAN_POINT('Ctrl Pts',(0.00442548803232603,0.0135212256101254,
-0.0119089346953794));
#49709=CARTESIAN_POINT('Ctrl Pts',(0.00440586757070844,0.0135212256101253,
-0.0117782950810129));
#49710=CARTESIAN_POINT('Ctrl Pts',(0.00439482636005699,0.0135212256101252,
-0.0117047789971533));
#49711=CARTESIAN_POINT('Ctrl Pts',(0.00438180805572112,0.0135212256101251,
-0.0116316227160819));
#49712=CARTESIAN_POINT('Ctrl Pts',(0.00436678116022483,0.013521225610125,
-0.011558894860445));
#49713=CARTESIAN_POINT('Ctrl Pts',(0.00429880769955738,0.0135212256101248,
-0.011229913798736));
#49714=CARTESIAN_POINT('Ctrl Pts',(0.00418987598555604,0.0135212256101246,
-0.0109096134480047));
#49715=CARTESIAN_POINT('Ctrl Pts',(0.00404445376166765,0.0135212256101244,
-0.0106037286146905));
#49716=CARTESIAN_POINT('Ctrl Pts',(0.00403582379204659,0.0135212256101244,
-0.0105855761153788));
#49717=CARTESIAN_POINT('Ctrl Pts',(0.00402706483909659,0.0135212256101244,
-0.0105674747504207));
#49718=CARTESIAN_POINT('Ctrl Pts',(0.00401817766918596,0.0135212256101244,
-0.0105494258704874));
#49719=CARTESIAN_POINT('Ctrl Pts',(0.00401119004020987,0.0135212256101244,
-0.0105352347525414));
#49720=CARTESIAN_POINT('Ctrl Pts',(0.00400412394035098,0.0135212256101244,
-0.0105210777685657));
#49721=CARTESIAN_POINT('Ctrl Pts',(0.00399698403616598,0.0135212256101244,
-0.0105069637321066));
#49722=CARTESIAN_POINT('Ctrl Pts',(0.00381744654911037,0.0135212256101242,
-0.0101520571994109));
#49723=CARTESIAN_POINT('Ctrl Pts',(0.00359079765244732,0.0135212256101241,
-0.00982262213931191));
#49724=CARTESIAN_POINT('Ctrl Pts',(0.00332467018493774,0.0135212256101241,
-0.00952801515336511));
#49725=CARTESIAN_POINT('Ctrl Pts',(0.00327375278488671,0.0135212256101241,
-0.00947164884927159));
#49726=CARTESIAN_POINT('Ctrl Pts',(0.0032213815704452,0.013521225610119,
-0.00941656604383548));
#49727=CARTESIAN_POINT('Ctrl Pts',(0.0031675992986144,0.013521225610119,
-0.00936284615281305));
#49728=CARTESIAN_POINT('Ctrl Pts',(0.00313750849569358,0.013521225610119,
-0.00933279025151588));
#49729=CARTESIAN_POINT('Ctrl Pts',(0.0031069759402194,0.0135212256101241,
-0.00930316108343312));
#49730=CARTESIAN_POINT('Ctrl Pts',(0.00307600881182139,0.0135212256101241,
-0.00927397334107523));
#49731=CARTESIAN_POINT('Ctrl Pts',(0.00305592031613699,0.0135212256101241,
-0.00925503913998115));
#49732=CARTESIAN_POINT('Ctrl Pts',(0.0030356489406292,0.0135212256101191,
-0.00923629070985852));
#49733=CARTESIAN_POINT('Ctrl Pts',(0.00301519660291451,0.0135212256101191,
-0.00921773219655775));
#49734=CARTESIAN_POINT('Ctrl Pts',(0.00290572585389851,0.0135212256101191,
-0.00911839810673394));
#49735=CARTESIAN_POINT('Ctrl Pts',(0.00279161951354767,0.0135212256101191,
-0.00902499526771897));
#49736=CARTESIAN_POINT('Ctrl Pts',(0.00267329637337972,0.0135212256101191,
-0.00893802803368589));
#49737=CARTESIAN_POINT('Ctrl Pts',(0.00257075184570355,0.0135212256101192,
-0.00886265804329714));
#49738=CARTESIAN_POINT('Ctrl Pts',(0.00246503183794056,0.0135212256101242,
-0.00879211589896134));
#49739=CARTESIAN_POINT('Ctrl Pts',(0.00235636239577334,0.0135212256101242,
-0.00872675896201271));
#49740=CARTESIAN_POINT('Ctrl Pts',(0.00219814089042433,0.0135212256101243,
-0.00863159998500149));
#49741=CARTESIAN_POINT('Ctrl Pts',(0.00203366811371355,0.0135212256101244,
-0.00854742067631489));
#49742=CARTESIAN_POINT('Ctrl Pts',(0.00186357782707476,0.0135212256101245,
-0.00847552126255479));
#49743=CARTESIAN_POINT('Ctrl Pts',(0.00179024018558216,0.0135212256101246,
-0.00844452047153923));
#49744=CARTESIAN_POINT('Ctrl Pts',(0.00171585740388813,0.0135212256101246,
-0.00841580601568659));
#49745=CARTESIAN_POINT('Ctrl Pts',(0.00164053200032731,0.0135212256101247,
-0.00838938077384102));
#49746=CARTESIAN_POINT('Ctrl Pts',(0.0016227936715147,0.0135212256101247,
-0.00838315791134508));
#49747=CARTESIAN_POINT('Ctrl Pts',(0.00160501052496767,0.0135212256101247,
-0.00837706468038289));
#49748=CARTESIAN_POINT('Ctrl Pts',(0.00158719063949712,0.0135212256101247,
-0.00837110296172034));
#49749=CARTESIAN_POINT('Ctrl Pts',(0.00112804892776666,0.0135212256101251,
-0.00821749514442541));
#49750=CARTESIAN_POINT('Ctrl Pts',(0.000643190067065385,0.0135212256101255,
-0.00814977887709749));
#49751=CARTESIAN_POINT('Ctrl Pts',(0.000156630255982111,0.013521225610126,
-0.00816621136866286));
#49752=CARTESIAN_POINT('Ctrl Pts',(0.000132844566441299,0.0135212256101261,
-0.00816701467821259));
#49753=CARTESIAN_POINT('Ctrl Pts',(0.000109055105933201,0.0135212256101261,
-0.00816802124209177));
#49754=CARTESIAN_POINT('Ctrl Pts',(8.52648460987993E-5,0.0135212256101261,
-0.0081692315113233));
#49755=CARTESIAN_POINT('Ctrl Pts',(6.53964806939949E-5,0.0135212256101261,
-0.00817024226410605));
#49756=CARTESIAN_POINT('Ctrl Pts',(4.55369000206317E-5,0.0135212256101262,
-0.00817139463835654));
#49757=CARTESIAN_POINT('Ctrl Pts',(2.56914149112288E-5,0.0135212256101261,
-0.00817268824315978));
#49758=CARTESIAN_POINT('Ctrl Pts',(-0.000298296126733115,0.0135212256101251,
-0.00819380699323063));
#49759=CARTESIAN_POINT('Ctrl Pts',(-0.000618909869140803,0.013521225610125,
-0.00825239931907039));
#49760=CARTESIAN_POINT('Ctrl Pts',(-0.000928653071344667,0.0135212256101248,
-0.00834875706957382));
#49761=CARTESIAN_POINT('Ctrl Pts',(-0.000948935745052395,0.0135212256101248,
-0.00835506678936352));
#49762=CARTESIAN_POINT('Ctrl Pts',(-0.000969162136026976,0.0135212256101248,
-0.00836153633871243));
#49763=CARTESIAN_POINT('Ctrl Pts',(-0.000989328103931621,0.0135212256101248,
-0.00836816498528667));
#49764=CARTESIAN_POINT('Ctrl Pts',(-0.00110526038790483,0.0135212256101247,
-0.00840627246124005));
#49765=CARTESIAN_POINT('Ctrl Pts',(-0.00121922018951225,0.0135212256101196,
-0.00844964141738153));
#49766=CARTESIAN_POINT('Ctrl Pts',(-0.00133080618113665,0.013521225610122,
-0.00849828346020436));
#49767=CARTESIAN_POINT('Ctrl Pts',(-0.00143947616796051,0.0135212256101244,
-0.0085456543718725));
#49768=CARTESIAN_POINT('Ctrl Pts',(-0.00154589536550546,0.0135212256101244,
-0.00859802668055264));
#49769=CARTESIAN_POINT('Ctrl Pts',(-0.00164966624456178,0.0135212256101243,
-0.0086554518957699));
#49770=CARTESIAN_POINT('Ctrl Pts',(-0.00171620850601353,0.0135212256101243,
-0.0086922753641616));
#49771=CARTESIAN_POINT('Ctrl Pts',(-0.00178166123650336,0.0135212256101192,
-0.00873117735060907));
#49772=CARTESIAN_POINT('Ctrl Pts',(-0.00184591193783782,0.0135212256101219,
-0.00877217981252655));
#49773=CARTESIAN_POINT('Ctrl Pts',(-0.00371483287808303,0.0135212256101277,
-0.01328056634437));
#49774=CARTESIAN_POINT('Ctrl Pts',(-0.00371549183366996,0.0135212256101277,
-0.0132774726740512));
#49775=CARTESIAN_POINT('Ctrl Pts',(-0.0037161468930533,0.0135212256101277,
-0.0132743781740399));
#49776=CARTESIAN_POINT('Ctrl Pts',(-0.00371731615019988,0.0135212256101277,
-0.0132688200925666));
#49777=CARTESIAN_POINT('Ctrl Pts',(-0.003717831777219,0.0135212256101277,
-0.0132663568120799));
#49778=CARTESIAN_POINT('Ctrl Pts',(-0.00371834493906906,0.0135212256101277,
-0.0132638930180542));
#49779=CARTESIAN_POINT('Origin',(0.,0.0153212256101277,-0.0121758532865581));
#49780=CARTESIAN_POINT('',(-0.00290000000001,0.0155212256101377,-0.0121758532865581));
#49781=CARTESIAN_POINT('',(-0.0027,0.0153212256101277,-0.0121758532865581));
#49782=CARTESIAN_POINT('Origin',(0.,0.0155212256101377,-0.0121758532865581));
#49783=CARTESIAN_POINT('Origin',(0.,0.0155212256101277,-0.0121758532865581));
#49784=CARTESIAN_POINT('',(-0.0038,0.0155212256101277,-0.0121758532865581));
#49785=CARTESIAN_POINT('Origin',(0.,0.0155212256101377,-0.0121758532865581));
#49786=CARTESIAN_POINT('Origin',(4.78424556569738E-19,0.0148792256101277,
-0.0121758532865581));
#49787=CARTESIAN_POINT('',(-0.00442435797140522,0.0148792256101377,-0.0125713536543859));
#49788=CARTESIAN_POINT('',(-0.00444200000001,0.0148792256101377,-0.0121758532865581));
#49789=CARTESIAN_POINT('Origin',(0.,0.0148792256101377,-0.0121758532865581));
#49790=CARTESIAN_POINT('Ctrl Pts',(-0.00442435797140521,0.0148792256101308,
-0.0125713536543859));
#49791=CARTESIAN_POINT('Ctrl Pts',(-0.00442800643686139,0.0148792260236933,
-0.0124648769960618));
#49792=CARTESIAN_POINT('Ctrl Pts',(-0.00442766428860729,0.0148792256101345,
-0.012358442139106));
#49793=CARTESIAN_POINT('Ctrl Pts',(-0.00442322426732517,0.0148792256101344,
-0.0122522393837103));
#49794=CARTESIAN_POINT('Ctrl Pts',(-0.00442009298055464,0.0148792256101343,
-0.0121773408051147));
#49795=CARTESIAN_POINT('Ctrl Pts',(-0.00441492275573164,0.0148792256101349,
-0.012102557690367));
#49796=CARTESIAN_POINT('Ctrl Pts',(-0.00440766855611385,0.014879225610135,
-0.0120279578270332));
#49797=CARTESIAN_POINT('Ctrl Pts',(-0.00439351054235581,0.0148792256101351,
-0.0118823613522907));
#49798=CARTESIAN_POINT('Ctrl Pts',(-0.00437141830531153,0.0148792256101352,
-0.0117374609477969));
#49799=CARTESIAN_POINT('Ctrl Pts',(-0.00434171523037098,0.0148792256101353,
-0.0115937591489407));
#49800=CARTESIAN_POINT('Ctrl Pts',(-0.00433640963489609,0.0148792256101354,
-0.0115680909777069));
#49801=CARTESIAN_POINT('Ctrl Pts',(-0.00433086104162323,0.0148792256101354,
-0.0115424611293754));
#49802=CARTESIAN_POINT('Ctrl Pts',(-0.00432507107819976,0.0148792256101354,
-0.0115168725829161));
#49803=CARTESIAN_POINT('Ctrl Pts',(-0.00432033646974495,0.0148792256101354,
-0.011495948141853));
#49804=CARTESIAN_POINT('Ctrl Pts',(-0.00431544270971432,0.0148792256101354,
-0.0114750612571913));
#49805=CARTESIAN_POINT('Ctrl Pts',(-0.00431039114734557,0.0148792256101355,
-0.0114542136188716));
#49806=CARTESIAN_POINT('Ctrl Pts',(-0.00423477824437842,0.0148792256101357,
-0.011142161556897));
#49807=CARTESIAN_POINT('Ctrl Pts',(-0.00412393664690842,0.0148792256101358,
-0.0108388232708057));
#49808=CARTESIAN_POINT('Ctrl Pts',(-0.0039813631737944,0.014879225610136,
-0.0105495620737052));
#49809=CARTESIAN_POINT('Ctrl Pts',(-0.00396120669884738,0.014879225610136,
-0.0105086674672601));
#49810=CARTESIAN_POINT('Ctrl Pts',(-0.00394040419837136,0.0148792256101361,
-0.010468038341568));
#49811=CARTESIAN_POINT('Ctrl Pts',(-0.00391899916438485,0.0148792256101361,
-0.0104277578853243));
#49812=CARTESIAN_POINT('Ctrl Pts',(-0.00364785767429892,0.0148792256101363,
-0.0099175179607283));
#49813=CARTESIAN_POINT('Ctrl Pts',(-0.00328050367389714,0.0148792256101364,
-0.00946181130830208));
#49814=CARTESIAN_POINT('Ctrl Pts',(-0.0028374264715703,0.0148792256101363,
-0.00909769299540765));
#49815=CARTESIAN_POINT('Ctrl Pts',(-0.0026578942354509,0.0148792256101363,
-0.00895015442970699));
#49816=CARTESIAN_POINT('Ctrl Pts',(-0.00246696490726739,0.0148792256101362,
-0.00881866982220281));
#49817=CARTESIAN_POINT('Ctrl Pts',(-0.00226578756927449,0.0148792256101361,
-0.00870553397651577));
#49818=CARTESIAN_POINT('Ctrl Pts',(-0.0022596861691341,0.0148792256101361,
-0.00870210273981861));
#49819=CARTESIAN_POINT('Ctrl Pts',(-0.00225357532131785,0.0148792256101361,
-0.00869868842155052));
#49820=CARTESIAN_POINT('Ctrl Pts',(-0.00224745505410032,0.0148792256101361,
-0.00869529109370495));
#49821=CARTESIAN_POINT('Ctrl Pts',(-0.00204000448908894,0.014879225610136,
-0.00858013638623183));
#49822=CARTESIAN_POINT('Ctrl Pts',(-0.0018217385611798,0.0148792256101359,
-0.00848445099112787));
#49823=CARTESIAN_POINT('Ctrl Pts',(-0.00159542878803322,0.0148792256101357,
-0.00840845967616131));
#49824=CARTESIAN_POINT('Ctrl Pts',(-0.00157798612369806,0.0148792256101357,
-0.00840260269976599));
#49825=CARTESIAN_POINT('Ctrl Pts',(-0.00156049566425499,0.0148792256101357,
-0.00839686301748051));
#49826=CARTESIAN_POINT('Ctrl Pts',(-0.0015429586822898,0.0148792256101356,
-0.0083912408836659));
#49827=CARTESIAN_POINT('Ctrl Pts',(-0.00152548865319278,0.0148792256101356,
-0.00838564021409097));
#49828=CARTESIAN_POINT('Ctrl Pts',(-0.00150797990800617,0.0148792256101356,
-0.00838015861597521));
#49829=CARTESIAN_POINT('Ctrl Pts',(-0.00149043985841481,0.0148792256101356,
-0.00837479781767868));
#49830=CARTESIAN_POINT('Ctrl Pts',(-0.00105189130935771,0.0148792256101353,
-0.00824076340104341));
#49831=CARTESIAN_POINT('Ctrl Pts',(-0.000592610978165706,0.0148792256101349,
-0.00818111254743533));
#49832=CARTESIAN_POINT('Ctrl Pts',(-0.000133044966495837,0.0148792256101344,
-0.00819713049545326));
#49833=CARTESIAN_POINT('Ctrl Pts',(-9.07585202619122E-5,0.0148792256101343,
-0.00819860436880429));
#49834=CARTESIAN_POINT('Ctrl Pts',(-4.84705149864253E-5,0.0148792256101342,
-0.0082007251339189));
#49835=CARTESIAN_POINT('Ctrl Pts',(-6.19786154605748E-6,0.0148792256101346,
-0.00820349756757392));
#49836=CARTESIAN_POINT('Ctrl Pts',(1.05822949543223E-5,0.0148792256101348,
-0.00820459808686552));
#49837=CARTESIAN_POINT('Ctrl Pts',(2.73591648051649E-5,0.0148792256101349,
-0.00820580129296554));
#49838=CARTESIAN_POINT('Ctrl Pts',(4.41187140605433E-5,0.0148792256101349,
-0.00820710631154845));
#49839=CARTESIAN_POINT('Ctrl Pts',(0.00053266307801239,0.0148792256101353,
-0.00824514787602107));
#49840=CARTESIAN_POINT('Ctrl Pts',(0.00100981843523539,0.0148792256101357,
-0.00836886688399673));
#49841=CARTESIAN_POINT('Ctrl Pts',(0.00144931013511217,0.014879225610136,
-0.00858335194830635));
#49842=CARTESIAN_POINT('Ctrl Pts',(0.00145705942355413,0.014879225610136,
-0.00858713383231075));
#49843=CARTESIAN_POINT('Ctrl Pts',(0.00146479681474301,0.014879225610136,
-0.00859094424863076));
#49844=CARTESIAN_POINT('Ctrl Pts',(0.0014725221409543,0.0148792256101358,
-0.00859478325868824));
#49845=CARTESIAN_POINT('Ctrl Pts',(0.00381143632930178,0.0148792256101254,
-0.0128782269849118));
#49846=CARTESIAN_POINT('Ctrl Pts',(0.00379265690764781,0.0148792256101253,
-0.0130598161005132));
#49847=CARTESIAN_POINT('Ctrl Pts',(0.00376077051328938,0.0148792256101251,
-0.0132393446902149));
#49848=CARTESIAN_POINT('Ctrl Pts',(0.0037154799419432,0.0148792256101249,
-0.0134153953703416));
#49849=CARTESIAN_POINT('Ctrl Pts',(0.00359834182940471,0.0148792256101245,
-0.0138707273250554));
#49850=CARTESIAN_POINT('Ctrl Pts',(0.00339149886618397,0.0148792256101244,
-0.0143027317276141));
#49851=CARTESIAN_POINT('Ctrl Pts',(0.00311742360125872,0.0148792256101242,
-0.014689428358699));
#49852=CARTESIAN_POINT('Ctrl Pts',(0.00310474522725224,0.0148792256101242,
-0.0147073164542091));
#49853=CARTESIAN_POINT('Ctrl Pts',(0.00309192048944817,0.0148792256101242,
-0.0147251109745272));
#49854=CARTESIAN_POINT('Ctrl Pts',(0.00307895095117516,0.0148792256101242,
-0.0147428102674581));
#49855=CARTESIAN_POINT('Ctrl Pts',(0.00306895335665116,0.0148792256101241,
-0.0147564538028223));
#49856=CARTESIAN_POINT('Ctrl Pts',(0.00305887098271552,0.0148792256101241,
-0.0147700389667957));
#49857=CARTESIAN_POINT('Ctrl Pts',(0.00304871004275737,0.0148792256101241,
-0.0147835579687215));
#49858=CARTESIAN_POINT('Ctrl Pts',(0.00275708960701588,0.014879225610124,
-0.0151715552650946));
#49859=CARTESIAN_POINT('Ctrl Pts',(0.00240031763648512,0.0148792256101241,
-0.0155071774786443));
#49860=CARTESIAN_POINT('Ctrl Pts',(0.00199622853595507,0.0148792256101242,
-0.0157734834877795));
#49861=CARTESIAN_POINT('Ctrl Pts',(0.00197766359633304,0.0148792256101242,
-0.01578571830177));
#49862=CARTESIAN_POINT('Ctrl Pts',(0.00195899734363262,0.0148792256101242,
-0.0157978055987294));
#49863=CARTESIAN_POINT('Ctrl Pts',(0.00194023113042077,0.0148792256101242,
-0.0158097433372555));
#49864=CARTESIAN_POINT('Ctrl Pts',(0.00192221297627362,0.0148792256101242,
-0.0158212052134744));
#49865=CARTESIAN_POINT('Ctrl Pts',(0.00190410052124748,0.0148792256101242,
-0.0158325304376092));
#49866=CARTESIAN_POINT('Ctrl Pts',(0.00188591545527795,0.0148792256101242,
-0.0158437048587242));
#49867=CARTESIAN_POINT('Ctrl Pts',(0.00165994072930097,0.0148792256101243,
-0.0159825625760211));
#49868=CARTESIAN_POINT('Ctrl Pts',(0.00142215214426251,0.0148792256101245,
-0.0160986101768173));
#49869=CARTESIAN_POINT('Ctrl Pts',(0.00117533764999415,0.0148792256101246,
-0.0161891562829656));
#49870=CARTESIAN_POINT('Ctrl Pts',(0.000983773707973866,0.0148792256101247,
-0.0162594332295435));
#49871=CARTESIAN_POINT('Ctrl Pts',(0.000786753455184054,0.0148792256101249,
-0.0163143417760653));
#49872=CARTESIAN_POINT('Ctrl Pts',(0.000585895492336925,0.0148792256101251,
-0.016354328533745));
#49873=CARTESIAN_POINT('Ctrl Pts',(0.000547731427410494,0.0148792256101251,
-0.0163619262271332));
#49874=CARTESIAN_POINT('Ctrl Pts',(0.000509428491718366,0.0148792256101251,
-0.0163689842436916));
#49875=CARTESIAN_POINT('Ctrl Pts',(0.000470997421712016,0.0148792256101252,
-0.0163755042835421));
#49876=CARTESIAN_POINT('Ctrl Pts',(0.000452558590985941,0.0148792256101252,
-0.0163786325313664));
#49877=CARTESIAN_POINT('Ctrl Pts',(0.000434090263008574,0.0148792256101252,
-0.0163816369315463));
#49878=CARTESIAN_POINT('Ctrl Pts',(0.000415593619263268,0.0148792256101253,
-0.0163845176364076));
#49879=CARTESIAN_POINT('Ctrl Pts',(0.000272246469694449,0.0148792256101253,
-0.0164068428126023));
#49880=CARTESIAN_POINT('Ctrl Pts',(0.000127921404413201,0.0148792256101256,
-0.0164216327040426));
#49881=CARTESIAN_POINT('Ctrl Pts',(-1.67712264430525E-5,0.0148792256101258,
-0.0164291348700418));
#49882=CARTESIAN_POINT('Ctrl Pts',(-0.000147634627786554,0.0148792256101261,
-0.016435920004532));
#49883=CARTESIAN_POINT('Ctrl Pts',(-0.000278803631839533,0.0148792256101258,
-0.0164367434329844));
#49884=CARTESIAN_POINT('Ctrl Pts',(-0.000409859018321533,0.0148792256101257,
-0.0164317350067629));
#49885=CARTESIAN_POINT('Ctrl Pts',(-0.000631005280122476,0.0148792256101255,
-0.0164232836583208));
#49886=CARTESIAN_POINT('Ctrl Pts',(-0.000851830836900023,0.0148792256101253,
-0.0163982486578753));
#49887=CARTESIAN_POINT('Ctrl Pts',(-0.0010703627002491,0.0148792256101251,
-0.0163569246506869));
#49888=CARTESIAN_POINT('Ctrl Pts',(-0.00111258219104488,0.0148792256101251,
-0.0163489410161066));
#49889=CARTESIAN_POINT('Ctrl Pts',(-0.0011547159952234,0.0148792256101251,
-0.0163403481742521));
#49890=CARTESIAN_POINT('Ctrl Pts',(-0.0011967496481623,0.0148792256101251,
-0.0163311464959581));
#49891=CARTESIAN_POINT('Ctrl Pts',(-0.00175017068631047,0.0148792256101247,
-0.0162099958940444));
#49892=CARTESIAN_POINT('Ctrl Pts',(-0.00227675051008725,0.0148792256101242,
-0.0159865200250432));
#49893=CARTESIAN_POINT('Ctrl Pts',(-0.00274261385400554,0.0148792256101242,
-0.0156656390938508));
#49894=CARTESIAN_POINT('Ctrl Pts',(-0.00275787640298179,0.0148792256101242,
-0.0156551264381723));
#49895=CARTESIAN_POINT('Ctrl Pts',(-0.00277307388134729,0.0148792256101242,
-0.0156445077234186));
#49896=CARTESIAN_POINT('Ctrl Pts',(-0.00278820502685331,0.0148792256101277,
-0.0156337828301188));
#49897=CARTESIAN_POINT('Origin',(0.,0.0148792256101377,-0.0121758532865581));
#49898=CARTESIAN_POINT('Ctrl Pts',(0.00273585250541839,0.0131897093384203,
-0.0149100121428775));
#49899=CARTESIAN_POINT('Ctrl Pts',(0.00185731657271958,0.0132408496933581,
-0.0157891323687994));
#49900=CARTESIAN_POINT('Ctrl Pts',(-0.00079607063101126,0.0133431139771879,
-0.0166247363049608));
#49901=CARTESIAN_POINT('Ctrl Pts',(-0.00411358954646197,0.0134965021899098,
-0.0140558444908958));
#49902=CARTESIAN_POINT('Ctrl Pts',(-0.00388811418891142,0.013649873976586,
-0.00987182162251869));
#49903=CARTESIAN_POINT('Ctrl Pts',(-0.000327275852545556,0.0138032457632622,
-0.00766718327907073));
#49904=CARTESIAN_POINT('Ctrl Pts',(0.0035167017971211,0.0139566175499384,
-0.00933527410552452));
#49905=CARTESIAN_POINT('Ctrl Pts',(0.0043393335020202,0.0141099893366145,
-0.013443238931041));
#49906=CARTESIAN_POINT('Ctrl Pts',(0.00143408777942091,0.0142633611232907,
-0.0164628810402578));
#49907=CARTESIAN_POINT('Ctrl Pts',(-0.00270110084645509,0.0144167329099669,
-0.0157993941062799));
#49908=CARTESIAN_POINT('Ctrl Pts',(-0.00452030709288378,0.0145701046966431,
-0.0120248245767944));
#49909=CARTESIAN_POINT('Ctrl Pts',(-0.00244790251763072,0.0147234846528409,
-0.00837675920613522));
#49910=CARTESIAN_POINT('Ctrl Pts',(0.000322306800181459,0.0148257406801466,
-0.00812604927686857));
#49911=CARTESIAN_POINT('Ctrl Pts',(0.0014715070400914,0.0148768727785604,
-0.00859881810453392));
#49912=CARTESIAN_POINT('Ctrl Pts',(0.00287311792214242,0.0133017513966655,
-0.0150471925844616));
#49913=CARTESIAN_POINT('Ctrl Pts',(0.00195050337019417,0.0133528917516033,
-0.0159704207452677));
#49914=CARTESIAN_POINT('Ctrl Pts',(-0.000836011734082826,0.0134551560354331,
-0.0168479492816357));
#49915=CARTESIAN_POINT('Ctrl Pts',(-0.00431997990639855,0.013608544248155,
-0.0141501689384272));
#49916=CARTESIAN_POINT('Ctrl Pts',(-0.00408319181585019,0.0137619160348312,
-0.00975622187220928));
#49917=CARTESIAN_POINT('Ctrl Pts',(-0.000343696202763411,0.0139152878215074,
-0.00744097062096028));
#49918=CARTESIAN_POINT('Ctrl Pts',(0.00369314461950277,0.0140686596081836,
-0.00919275425686676));
#49919=CARTESIAN_POINT('Ctrl Pts',(0.00455705007127225,0.0142220313948598,
-0.0135068272342465));
#49920=CARTESIAN_POINT('Ctrl Pts',(0.0015060399977043,0.014375403181536,
-0.0166779732829696));
#49921=CARTESIAN_POINT('Ctrl Pts',(-0.00283662267468522,0.0145287749682122,
-0.0159811973429861));
#49922=CARTESIAN_POINT('Ctrl Pts',(-0.00474710361630614,0.0146821467548883,
-0.0120172470415502));
#49923=CARTESIAN_POINT('Ctrl Pts',(-0.0025707206734037,0.0148355267110861,
-0.00818614796847156));
#49924=CARTESIAN_POINT('Ctrl Pts',(0.000338477839063224,0.0149377827383919,
-0.00792285921675396));
#49925=CARTESIAN_POINT('Ctrl Pts',(0.00154533668795086,0.0149889148368055,
-0.00841934818650121));
#49926=CARTESIAN_POINT('Ctrl Pts',(0.00301038333886644,0.0134137934549108,
-0.0151843730260457));
#49927=CARTESIAN_POINT('Ctrl Pts',(0.00204369016766876,0.0134649338098485,
-0.0161517091217361));
#49928=CARTESIAN_POINT('Ctrl Pts',(-0.000875952837154391,0.0135671980936784,
-0.0170711622583103));
#49929=CARTESIAN_POINT('Ctrl Pts',(-0.00452637026633513,0.0137205863064002,
-0.0142444933859585));
#49930=CARTESIAN_POINT('Ctrl Pts',(-0.00427826944278896,0.0138739580930764,
-0.00964062212189988));
#49931=CARTESIAN_POINT('Ctrl Pts',(-0.000360116552981276,0.0140273298797526,
-0.00721475796284981));
#49932=CARTESIAN_POINT('Ctrl Pts',(0.00386958744188443,0.0141807016664288,
-0.00905023440820901));
#49933=CARTESIAN_POINT('Ctrl Pts',(0.00477476664052429,0.014334073453105,
-0.0135704155374519));
#49934=CARTESIAN_POINT('Ctrl Pts',(0.00157799221598771,0.0144874452397812,
-0.0168930655256812));
#49935=CARTESIAN_POINT('Ctrl Pts',(-0.00297214450291535,0.0146408170264574,
-0.0161630005796922));
#49936=CARTESIAN_POINT('Ctrl Pts',(-0.0049739001397285,0.0147941888131336,
-0.0120096695063059));
#49937=CARTESIAN_POINT('Ctrl Pts',(-0.00269353882917668,0.0149475687693314,
-0.0079955367308079));
#49938=CARTESIAN_POINT('Ctrl Pts',(0.000354648877944988,0.0150498247966371,
-0.00771966915663935));
#49939=CARTESIAN_POINT('Ctrl Pts',(0.00161916633581033,0.0151009568950508,
-0.00823987826846848));
#49940=CARTESIAN_POINT('Ctrl Pts',(0.00314764875559048,0.013525835513156,
-0.0153215534676299));
#49941=CARTESIAN_POINT('Ctrl Pts',(0.00213687696514335,0.0135769758680938,
-0.0163329974982044));
#49942=CARTESIAN_POINT('Ctrl Pts',(-0.000915893940225956,0.0136792401519236,
-0.0172943752349851));
#49943=CARTESIAN_POINT('Ctrl Pts',(-0.00473276062627171,0.0138326283646455,
-0.0143388178334899));
#49944=CARTESIAN_POINT('Ctrl Pts',(-0.00447334706972773,0.0139860001513217,
-0.00952502237159047));
#49945=CARTESIAN_POINT('Ctrl Pts',(-0.000376536903199133,0.0141393719379978,
-0.00698854530473934));
#49946=CARTESIAN_POINT('Ctrl Pts',(0.00404603026426609,0.014292743724674,
-0.00890771455955126));
#49947=CARTESIAN_POINT('Ctrl Pts',(0.00499248320977635,0.0144461155113502,
-0.0136340038406574));
#49948=CARTESIAN_POINT('Ctrl Pts',(0.00164994443427111,0.0145994872980264,
-0.017108157768393));
#49949=CARTESIAN_POINT('Ctrl Pts',(-0.00310766633114547,0.0147528590847026,
-0.0163448038163983));
#49950=CARTESIAN_POINT('Ctrl Pts',(-0.00520069666315088,0.0149062308713788,
-0.0120020919710616));
#49951=CARTESIAN_POINT('Ctrl Pts',(-0.00281635698494966,0.0150596108275766,
-0.00780492549314423));
#49952=CARTESIAN_POINT('Ctrl Pts',(0.000370819916826753,0.0151618668548823,
-0.00751647909652474));
#49953=CARTESIAN_POINT('Ctrl Pts',(0.00169299598366981,0.015212998953296,
-0.00806040835043577));
#49954=CARTESIAN_POINT('Ctrl Pts',(-0.00441828210417968,0.0148776665296917,
-0.0126491402494078));
#49955=CARTESIAN_POINT('Ctrl Pts',(-0.00441940407973438,0.0148779235829229,
-0.0126362528549548));
#49956=CARTESIAN_POINT('Ctrl Pts',(-0.004420469123244,0.0148781812985605,
-0.0126233605617627));
#49957=CARTESIAN_POINT('Ctrl Pts',(-0.00442249570517061,0.0148787009257427,
-0.0125974314178203));
#49958=CARTESIAN_POINT('Ctrl Pts',(-0.00442345603009106,0.014878962850937,
-0.0125843945715201));
#49959=CARTESIAN_POINT('Ctrl Pts',(-0.00442435797139694,0.014879225610126,
-0.0125713536543851));
#49960=CARTESIAN_POINT('Ctrl Pts',(-0.00212268276440621,0.0131872148797876,
-0.00826423615450915));
#49961=CARTESIAN_POINT('Ctrl Pts',(-0.000865862298820361,0.0132383524108938,
-0.00758217776404467));
#49962=CARTESIAN_POINT('Ctrl Pts',(0.00233441369372333,0.0133406138708919,
-0.00752903712240916));
#49963=CARTESIAN_POINT('Ctrl Pts',(0.00515297679530513,0.0134939992597821,
-0.011448570453063));
#49964=CARTESIAN_POINT('Ctrl Pts',(0.00353471435351032,0.0136473710464583,
-0.0159900584693641));
#49965=CARTESIAN_POINT('Ctrl Pts',(-0.0011147975591788,0.0138007428331345,
-0.017256387645163));
#49966=CARTESIAN_POINT('Ctrl Pts',(-0.00480898843763011,0.0139541146198107,
-0.0141581177086575));
#49967=CARTESIAN_POINT('Ctrl Pts',(-0.00437176720712775,0.0141074864064868,
-0.00935745063273735));
#49968=CARTESIAN_POINT('Ctrl Pts',(-0.000178648504016178,0.014260858193163,
-0.00697751819934707));
#49969=CARTESIAN_POINT('Ctrl Pts',(0.00416560098168492,0.0144142299798392,
-0.00906295508731642));
#49970=CARTESIAN_POINT('Ctrl Pts',(0.0049368105886653,0.0145676017665154,
-0.013822064507663));
#49971=CARTESIAN_POINT('Ctrl Pts',(0.00145635533370079,0.0147209957524096,
-0.0171681194120463));
#49972=CARTESIAN_POINT('Ctrl Pts',(-0.00168199952693254,0.0148232658094117,
-0.0165374240793895));
#49973=CARTESIAN_POINT('Ctrl Pts',(-0.00279496027439306,0.0148744119375218,
-0.0156391938142977));
#49974=CARTESIAN_POINT('Ctrl Pts',(-0.00203007829900054,0.0132993109570197,
-0.00843488492947408));
#49975=CARTESIAN_POINT('Ctrl Pts',(-0.000828088064892557,0.0133504484881259,
-0.00778258211703734));
#49976=CARTESIAN_POINT('Ctrl Pts',(0.00223257222416043,0.013452709948124,
-0.0077317597967226));
#49977=CARTESIAN_POINT('Ctrl Pts',(0.00492817228406173,0.0136060953370142,
-0.0114802989991858));
#49978=CARTESIAN_POINT('Ctrl Pts',(0.00338050839369504,0.0137594671236905,
-0.0158236594021912));
#49979=CARTESIAN_POINT('Ctrl Pts',(-0.00106616323956478,0.0139128389103666,
-0.0170347435181447));
#49980=CARTESIAN_POINT('Ctrl Pts',(-0.00459919081224947,0.0140662106970428,
-0.0140716391541701));
#49981=CARTESIAN_POINT('Ctrl Pts',(-0.00418104385840945,0.014219582483719,
-0.00948040667470061));
#49982=CARTESIAN_POINT('Ctrl Pts',(-0.000170854758531761,0.0143729542703952,
-0.00720430151799592));
#49983=CARTESIAN_POINT('Ctrl Pts',(0.00398387187054749,0.0145263260570714,
-0.00919875883455404));
#49984=CARTESIAN_POINT('Ctrl Pts',(0.00472143657562934,0.0146796978437475,
-0.0137502466587449));
#49985=CARTESIAN_POINT('Ctrl Pts',(0.00139282016519631,0.0148330918296417,
-0.0169503260877372));
#49986=CARTESIAN_POINT('Ctrl Pts',(-0.00160862037220625,0.0149353618866439,
-0.0163471455609165));
#49987=CARTESIAN_POINT('Ctrl Pts',(-0.00267302693306653,0.014986508014754,
-0.0154881016193325));
#49988=CARTESIAN_POINT('Ctrl Pts',(-0.00193747383359484,0.013411407034252,
-0.00860553370443901));
#49989=CARTESIAN_POINT('Ctrl Pts',(-0.000790313830964761,0.013462544565358,
-0.00798298647003001));
#49990=CARTESIAN_POINT('Ctrl Pts',(0.00213073075459756,0.0135648060253562,
-0.00793448247103606));
#49991=CARTESIAN_POINT('Ctrl Pts',(0.00470336777281834,0.0137181914142464,
-0.0115120275453086));
#49992=CARTESIAN_POINT('Ctrl Pts',(0.00322630243387977,0.0138715632009226,
-0.0156572603350182));
#49993=CARTESIAN_POINT('Ctrl Pts',(-0.00101752891995075,0.0140249349875988,
-0.0168130993911263));
#49994=CARTESIAN_POINT('Ctrl Pts',(-0.00438939318686883,0.014178306774275,
-0.0139851605996826));
#49995=CARTESIAN_POINT('Ctrl Pts',(-0.00399032050969115,0.0143316785609512,
-0.00960336271666387));
#49996=CARTESIAN_POINT('Ctrl Pts',(-0.000163061013047346,0.0144850503476274,
-0.00743108483664477));
#49997=CARTESIAN_POINT('Ctrl Pts',(0.00380214275941005,0.0146384221343036,
-0.00933456258179167));
#49998=CARTESIAN_POINT('Ctrl Pts',(0.00450606256259337,0.0147917939209798,
-0.0136784288098268));
#49999=CARTESIAN_POINT('Ctrl Pts',(0.00132928499669186,0.0149451879068739,
-0.0167325327634281));
#50000=CARTESIAN_POINT('Ctrl Pts',(-0.00153524121747995,0.0150474579638761,
-0.0161568670424437));
#50001=CARTESIAN_POINT('Ctrl Pts',(-0.00255109359174,0.0150986040919861,
-0.0153370094243671));
#50002=CARTESIAN_POINT('Ctrl Pts',(-0.00184486936818917,0.0135235031114842,
-0.00877618247940394));
#50003=CARTESIAN_POINT('Ctrl Pts',(-0.000752539597036957,0.0135746406425903,
-0.00818339082302267));
#50004=CARTESIAN_POINT('Ctrl Pts',(0.00202888928503466,0.0136769021025885,
-0.00813720514534951));
#50005=CARTESIAN_POINT('Ctrl Pts',(0.00447856326157495,0.0138302874914787,
-0.0115437560914314));
#50006=CARTESIAN_POINT('Ctrl Pts',(0.0030720964740645,0.0139836592781549,
-0.0154908612678453));
#50007=CARTESIAN_POINT('Ctrl Pts',(-0.000968894600336737,0.0141370310648311,
-0.0165914552641079));
#50008=CARTESIAN_POINT('Ctrl Pts',(-0.0041795955614882,0.0142904028515072,
-0.0138986820451953));
#50009=CARTESIAN_POINT('Ctrl Pts',(-0.00379959716097288,0.0144437746381834,
-0.00972631875862713));
#50010=CARTESIAN_POINT('Ctrl Pts',(-0.000155267267562925,0.0145971464248596,
-0.00765786815529363));
#50011=CARTESIAN_POINT('Ctrl Pts',(0.0036204136482726,0.0147505182115358,
-0.00947036632902929));
#50012=CARTESIAN_POINT('Ctrl Pts',(0.0042906885495574,0.014903889998212,
-0.0136066109609086));
#50013=CARTESIAN_POINT('Ctrl Pts',(0.00126574982818739,0.0150572839841062,
-0.0165147394391191));
#50014=CARTESIAN_POINT('Ctrl Pts',(-0.00146186206275366,0.0151595540411082,
-0.0159665885239708));
#50015=CARTESIAN_POINT('Ctrl Pts',(-0.00242916025041347,0.0152107001692183,
-0.0151859172294018));
#50016=CARTESIAN_POINT('Origin',(0.,0.0154212256101277,-0.0121758532865581));
#50017=CARTESIAN_POINT('',(-0.0039,0.0154212256101277,-0.0121758532865581));
#50018=CARTESIAN_POINT('',(0.122354602804926,0.119215454316483,0.148920627538376));
#50019=CARTESIAN_POINT('',(0.122354602804926,0.119215454316483,0.148920627538376));
#50020=CARTESIAN_POINT('',(0.122354602804926,0.119215454316483,0.148920627538376));
#50021=CARTESIAN_POINT('',(0.122354602804926,0.119215454316483,0.148920627538376));
#50022=CARTESIAN_POINT('',(0.122354602804926,0.119215454316483,0.148920627538376));
#50023=CARTESIAN_POINT('',(0.122354602804926,0.119215454316483,0.148920627538376));
#50024=CARTESIAN_POINT('',(0.122354602804926,0.119215454316483,0.148920627538376));
#50025=CARTESIAN_POINT('',(0.122354602804926,0.119215454316483,0.148920627538376));
#50026=CARTESIAN_POINT('',(0.122354602804926,0.119215454316483,0.148920627538376));
#50027=CARTESIAN_POINT('',(0.122354602804926,0.119215454316483,0.148920627538376));
#50028=CARTESIAN_POINT('',(0.122354602804926,0.119215454316483,0.148920627538376));
#50029=CARTESIAN_POINT('',(0.122354602804926,0.119215454316483,0.148920627538376));
#50030=CARTESIAN_POINT('',(0.122354602804926,0.119215454316483,0.148920627538376));
#50031=CARTESIAN_POINT('',(0.122354602804926,0.119215454316483,0.148920627538376));
#50032=CARTESIAN_POINT('',(0.122354602804926,0.119215454316483,0.148920627538376));
#50033=CARTESIAN_POINT('',(0.122354602804926,0.119215454316483,0.148920627538376));
#50034=CARTESIAN_POINT('',(0.122354602804926,0.119215454316483,0.148920627538376));
#50035=CARTESIAN_POINT('',(0.122354602804926,0.119215454316483,0.148920627538376));
#50036=CARTESIAN_POINT('',(0.122354602804926,0.119215454316483,0.148920627538376));
#50037=CARTESIAN_POINT('',(0.122354602804926,0.119215454316483,0.148920627538376));
#50038=UNCERTAINTY_MEASURE_WITH_UNIT(LENGTH_MEASURE(1.E-5),#50082,
'DISTANCE_ACCURACY_VALUE',
'Maximum model space distance between geometric entities at asserted c
onnectivities');
#50039=UNCERTAINTY_MEASURE_WITH_UNIT(LENGTH_MEASURE(1.E-5),#50082,
'DISTANCE_ACCURACY_VALUE',
'Maximum model space distance between geometric entities at asserted c
onnectivities');
#50040=UNCERTAINTY_MEASURE_WITH_UNIT(LENGTH_MEASURE(1.E-5),#50082,
'DISTANCE_ACCURACY_VALUE',
'Maximum model space distance between geometric entities at asserted c
onnectivities');
#50041=UNCERTAINTY_MEASURE_WITH_UNIT(LENGTH_MEASURE(1.E-5),#50082,
'DISTANCE_ACCURACY_VALUE',
'Maximum model space distance between geometric entities at asserted c
onnectivities');
#50042=UNCERTAINTY_MEASURE_WITH_UNIT(LENGTH_MEASURE(1.E-5),#50082,
'DISTANCE_ACCURACY_VALUE',
'Maximum model space distance between geometric entities at asserted c
onnectivities');
#50043=UNCERTAINTY_MEASURE_WITH_UNIT(LENGTH_MEASURE(1.E-5),#50082,
'DISTANCE_ACCURACY_VALUE',
'Maximum model space distance between geometric entities at asserted c
onnectivities');
#50044=UNCERTAINTY_MEASURE_WITH_UNIT(LENGTH_MEASURE(1.E-5),#50082,
'DISTANCE_ACCURACY_VALUE',
'Maximum model space distance between geometric entities at asserted c
onnectivities');
#50045=UNCERTAINTY_MEASURE_WITH_UNIT(LENGTH_MEASURE(1.E-5),#50082,
'DISTANCE_ACCURACY_VALUE',
'Maximum model space distance between geometric entities at asserted c
onnectivities');
#50046=UNCERTAINTY_MEASURE_WITH_UNIT(LENGTH_MEASURE(1.E-5),#50082,
'DISTANCE_ACCURACY_VALUE',
'Maximum model space distance between geometric entities at asserted c
onnectivities');
#50047=UNCERTAINTY_MEASURE_WITH_UNIT(LENGTH_MEASURE(1.E-5),#50082,
'DISTANCE_ACCURACY_VALUE',
'Maximum model space distance between geometric entities at asserted c
onnectivities');
#50048=UNCERTAINTY_MEASURE_WITH_UNIT(LENGTH_MEASURE(1.E-5),#50082,
'DISTANCE_ACCURACY_VALUE',
'Maximum model space distance between geometric entities at asserted c
onnectivities');
#50049=UNCERTAINTY_MEASURE_WITH_UNIT(LENGTH_MEASURE(1.E-5),#50082,
'DISTANCE_ACCURACY_VALUE',
'Maximum model space distance between geometric entities at asserted c
onnectivities');
#50050=UNCERTAINTY_MEASURE_WITH_UNIT(LENGTH_MEASURE(1.E-5),#50082,
'DISTANCE_ACCURACY_VALUE',
'Maximum model space distance between geometric entities at asserted c
onnectivities');
#50051=UNCERTAINTY_MEASURE_WITH_UNIT(LENGTH_MEASURE(1.E-5),#50082,
'DISTANCE_ACCURACY_VALUE',
'Maximum model space distance between geometric entities at asserted c
onnectivities');
#50052=UNCERTAINTY_MEASURE_WITH_UNIT(LENGTH_MEASURE(1.E-5),#50082,
'DISTANCE_ACCURACY_VALUE',
'Maximum model space distance between geometric entities at asserted c
onnectivities');
#50053=UNCERTAINTY_MEASURE_WITH_UNIT(LENGTH_MEASURE(1.E-5),#50082,
'DISTANCE_ACCURACY_VALUE',
'Maximum model space distance between geometric entities at asserted c
onnectivities');
#50054=UNCERTAINTY_MEASURE_WITH_UNIT(LENGTH_MEASURE(1.E-5),#50082,
'DISTANCE_ACCURACY_VALUE',
'Maximum model space distance between geometric entities at asserted c
onnectivities');
#50055=UNCERTAINTY_MEASURE_WITH_UNIT(LENGTH_MEASURE(1.E-5),#50082,
'DISTANCE_ACCURACY_VALUE',
'Maximum model space distance between geometric entities at asserted c
onnectivities');
#50056=UNCERTAINTY_MEASURE_WITH_UNIT(LENGTH_MEASURE(1.E-5),#50082,
'DISTANCE_ACCURACY_VALUE',
'Maximum model space distance between geometric entities at asserted c
onnectivities');
#50057=UNCERTAINTY_MEASURE_WITH_UNIT(LENGTH_MEASURE(1.E-5),#50082,
'DISTANCE_ACCURACY_VALUE',
'Maximum model space distance between geometric entities at asserted c
onnectivities');
#50058=UNCERTAINTY_MEASURE_WITH_UNIT(LENGTH_MEASURE(1.E-5),#50082,
'DISTANCE_ACCURACY_VALUE',
'Maximum model space distance between geometric entities at asserted c
onnectivities');
#50059=UNCERTAINTY_MEASURE_WITH_UNIT(LENGTH_MEASURE(1.E-5),#50082,
'DISTANCE_ACCURACY_VALUE',
'Maximum model space distance between geometric entities at asserted c
onnectivities');
#50060=(
GEOMETRIC_REPRESENTATION_CONTEXT(3)
GLOBAL_UNCERTAINTY_ASSIGNED_CONTEXT((#50038))
GLOBAL_UNIT_ASSIGNED_CONTEXT((#50082,#50083,#50084))
REPRESENTATION_CONTEXT('','3D')
);
#50061=(
GEOMETRIC_REPRESENTATION_CONTEXT(3)
GLOBAL_UNCERTAINTY_ASSIGNED_CONTEXT((#50039))
GLOBAL_UNIT_ASSIGNED_CONTEXT((#50082,#50083,#50084))
REPRESENTATION_CONTEXT('','3D')
);
#50062=(
GEOMETRIC_REPRESENTATION_CONTEXT(3)
GLOBAL_UNCERTAINTY_ASSIGNED_CONTEXT((#50040))
GLOBAL_UNIT_ASSIGNED_CONTEXT((#50082,#50083,#50084))
REPRESENTATION_CONTEXT('','3D')
);
#50063=(
GEOMETRIC_REPRESENTATION_CONTEXT(3)
GLOBAL_UNCERTAINTY_ASSIGNED_CONTEXT((#50041))
GLOBAL_UNIT_ASSIGNED_CONTEXT((#50082,#50083,#50084))
REPRESENTATION_CONTEXT('','3D')
);
#50064=(
GEOMETRIC_REPRESENTATION_CONTEXT(3)
GLOBAL_UNCERTAINTY_ASSIGNED_CONTEXT((#50042))
GLOBAL_UNIT_ASSIGNED_CONTEXT((#50082,#50083,#50084))
REPRESENTATION_CONTEXT('','3D')
);
#50065=(
GEOMETRIC_REPRESENTATION_CONTEXT(3)
GLOBAL_UNCERTAINTY_ASSIGNED_CONTEXT((#50043))
GLOBAL_UNIT_ASSIGNED_CONTEXT((#50082,#50083,#50084))
REPRESENTATION_CONTEXT('','3D')
);
#50066=(
GEOMETRIC_REPRESENTATION_CONTEXT(3)
GLOBAL_UNCERTAINTY_ASSIGNED_CONTEXT((#50044))
GLOBAL_UNIT_ASSIGNED_CONTEXT((#50082,#50083,#50084))
REPRESENTATION_CONTEXT('','3D')
);
#50067=(
GEOMETRIC_REPRESENTATION_CONTEXT(3)
GLOBAL_UNCERTAINTY_ASSIGNED_CONTEXT((#50045))
GLOBAL_UNIT_ASSIGNED_CONTEXT((#50082,#50083,#50084))
REPRESENTATION_CONTEXT('','3D')
);
#50068=(
GEOMETRIC_REPRESENTATION_CONTEXT(3)
GLOBAL_UNCERTAINTY_ASSIGNED_CONTEXT((#50046))
GLOBAL_UNIT_ASSIGNED_CONTEXT((#50082,#50083,#50084))
REPRESENTATION_CONTEXT('','3D')
);
#50069=(
GEOMETRIC_REPRESENTATION_CONTEXT(3)
GLOBAL_UNCERTAINTY_ASSIGNED_CONTEXT((#50047))
GLOBAL_UNIT_ASSIGNED_CONTEXT((#50082,#50083,#50084))
REPRESENTATION_CONTEXT('','3D')
);
#50070=(
GEOMETRIC_REPRESENTATION_CONTEXT(3)
GLOBAL_UNCERTAINTY_ASSIGNED_CONTEXT((#50048))
GLOBAL_UNIT_ASSIGNED_CONTEXT((#50082,#50083,#50084))
REPRESENTATION_CONTEXT('','3D')
);
#50071=(
GEOMETRIC_REPRESENTATION_CONTEXT(3)
GLOBAL_UNCERTAINTY_ASSIGNED_CONTEXT((#50049))
GLOBAL_UNIT_ASSIGNED_CONTEXT((#50082,#50083,#50084))
REPRESENTATION_CONTEXT('','3D')
);
#50072=(
GEOMETRIC_REPRESENTATION_CONTEXT(3)
GLOBAL_UNCERTAINTY_ASSIGNED_CONTEXT((#50050))
GLOBAL_UNIT_ASSIGNED_CONTEXT((#50082,#50083,#50084))
REPRESENTATION_CONTEXT('','3D')
);
#50073=(
GEOMETRIC_REPRESENTATION_CONTEXT(3)
GLOBAL_UNCERTAINTY_ASSIGNED_CONTEXT((#50051))
GLOBAL_UNIT_ASSIGNED_CONTEXT((#50082,#50083,#50084))
REPRESENTATION_CONTEXT('','3D')
);
#50074=(
GEOMETRIC_REPRESENTATION_CONTEXT(3)
GLOBAL_UNCERTAINTY_ASSIGNED_CONTEXT((#50052))
GLOBAL_UNIT_ASSIGNED_CONTEXT((#50082,#50083,#50084))
REPRESENTATION_CONTEXT('','3D')
);
#50075=(
GEOMETRIC_REPRESENTATION_CONTEXT(3)
GLOBAL_UNCERTAINTY_ASSIGNED_CONTEXT((#50053))
GLOBAL_UNIT_ASSIGNED_CONTEXT((#50082,#50083,#50084))
REPRESENTATION_CONTEXT('','3D')
);
#50076=(
GEOMETRIC_REPRESENTATION_CONTEXT(3)
GLOBAL_UNCERTAINTY_ASSIGNED_CONTEXT((#50054))
GLOBAL_UNIT_ASSIGNED_CONTEXT((#50082,#50083,#50084))
REPRESENTATION_CONTEXT('','3D')
);
#50077=(
GEOMETRIC_REPRESENTATION_CONTEXT(3)
GLOBAL_UNCERTAINTY_ASSIGNED_CONTEXT((#50055))
GLOBAL_UNIT_ASSIGNED_CONTEXT((#50082,#50083,#50084))
REPRESENTATION_CONTEXT('','3D')
);
#50078=(
GEOMETRIC_REPRESENTATION_CONTEXT(3)
GLOBAL_UNCERTAINTY_ASSIGNED_CONTEXT((#50056))
GLOBAL_UNIT_ASSIGNED_CONTEXT((#50082,#50083,#50084))
REPRESENTATION_CONTEXT('','3D')
);
#50079=(
GEOMETRIC_REPRESENTATION_CONTEXT(3)
GLOBAL_UNCERTAINTY_ASSIGNED_CONTEXT((#50057))
GLOBAL_UNIT_ASSIGNED_CONTEXT((#50082,#50083,#50084))
REPRESENTATION_CONTEXT('','3D')
);
#50080=(
GEOMETRIC_REPRESENTATION_CONTEXT(3)
GLOBAL_UNCERTAINTY_ASSIGNED_CONTEXT((#50058))
GLOBAL_UNIT_ASSIGNED_CONTEXT((#50082,#50083,#50084))
REPRESENTATION_CONTEXT('','3D')
);
#50081=(
GEOMETRIC_REPRESENTATION_CONTEXT(3)
GLOBAL_UNCERTAINTY_ASSIGNED_CONTEXT((#50059))
GLOBAL_UNIT_ASSIGNED_CONTEXT((#50082,#50083,#50084))
REPRESENTATION_CONTEXT('','3D')
);
#50082=(
LENGTH_UNIT()
NAMED_UNIT(*)
SI_UNIT($,.METRE.)
);
#50083=(
NAMED_UNIT(*)
PLANE_ANGLE_UNIT()
SI_UNIT($,.RADIAN.)
);
#50084=(
NAMED_UNIT(*)
SI_UNIT($,.STERADIAN.)
SOLID_ANGLE_UNIT()
);
#50085=SHAPE_DEFINITION_REPRESENTATION(#50106,#50147);
#50086=SHAPE_DEFINITION_REPRESENTATION(#50107,#50148);
#50087=SHAPE_DEFINITION_REPRESENTATION(#50108,#50149);
#50088=SHAPE_DEFINITION_REPRESENTATION(#50109,#50150);
#50089=SHAPE_DEFINITION_REPRESENTATION(#50110,#50151);
#50090=SHAPE_DEFINITION_REPRESENTATION(#50111,#50152);
#50091=SHAPE_DEFINITION_REPRESENTATION(#50112,#50153);
#50092=SHAPE_DEFINITION_REPRESENTATION(#50113,#50154);
#50093=SHAPE_DEFINITION_REPRESENTATION(#50114,#50155);
#50094=SHAPE_DEFINITION_REPRESENTATION(#50115,#50156);
#50095=SHAPE_DEFINITION_REPRESENTATION(#50116,#50157);
#50096=SHAPE_DEFINITION_REPRESENTATION(#50117,#50158);
#50097=SHAPE_DEFINITION_REPRESENTATION(#50118,#50159);
#50098=SHAPE_DEFINITION_REPRESENTATION(#50119,#50160);
#50099=SHAPE_DEFINITION_REPRESENTATION(#50120,#50161);
#50100=SHAPE_DEFINITION_REPRESENTATION(#50121,#50162);
#50101=SHAPE_DEFINITION_REPRESENTATION(#50122,#50163);
#50102=SHAPE_DEFINITION_REPRESENTATION(#50123,#50164);
#50103=SHAPE_DEFINITION_REPRESENTATION(#50124,#50165);
#50104=SHAPE_DEFINITION_REPRESENTATION(#50125,#50166);
#50105=SHAPE_DEFINITION_REPRESENTATION(#50126,#50167);
#50106=PRODUCT_DEFINITION_SHAPE('',$,#50169);
#50107=PRODUCT_DEFINITION_SHAPE('',$,#50170);
#50108=PRODUCT_DEFINITION_SHAPE('',$,#50171);
#50109=PRODUCT_DEFINITION_SHAPE('',$,#50172);
#50110=PRODUCT_DEFINITION_SHAPE('',$,#50173);
#50111=PRODUCT_DEFINITION_SHAPE('',$,#50174);
#50112=PRODUCT_DEFINITION_SHAPE('',$,#50175);
#50113=PRODUCT_DEFINITION_SHAPE('',$,#50176);
#50114=PRODUCT_DEFINITION_SHAPE('',$,#50177);
#50115=PRODUCT_DEFINITION_SHAPE('',$,#50178);
#50116=PRODUCT_DEFINITION_SHAPE('',$,#50179);
#50117=PRODUCT_DEFINITION_SHAPE('',$,#50180);
#50118=PRODUCT_DEFINITION_SHAPE('',$,#50181);
#50119=PRODUCT_DEFINITION_SHAPE('',$,#50182);
#50120=PRODUCT_DEFINITION_SHAPE('',$,#50183);
#50121=PRODUCT_DEFINITION_SHAPE('',$,#50184);
#50122=PRODUCT_DEFINITION_SHAPE('',$,#50185);
#50123=PRODUCT_DEFINITION_SHAPE('',$,#50186);
#50124=PRODUCT_DEFINITION_SHAPE('',$,#50187);
#50125=PRODUCT_DEFINITION_SHAPE('',$,#50188);
#50126=PRODUCT_DEFINITION_SHAPE('',$,#50189);
#50127=PRODUCT_DEFINITION_SHAPE($,$,#71);
#50128=PRODUCT_DEFINITION_SHAPE($,$,#72);
#50129=PRODUCT_DEFINITION_SHAPE($,$,#73);
#50130=PRODUCT_DEFINITION_SHAPE($,$,#74);
#50131=PRODUCT_DEFINITION_SHAPE($,$,#75);
#50132=PRODUCT_DEFINITION_SHAPE($,$,#76);
#50133=PRODUCT_DEFINITION_SHAPE($,$,#77);
#50134=PRODUCT_DEFINITION_SHAPE($,$,#78);
#50135=PRODUCT_DEFINITION_SHAPE($,$,#79);
#50136=PRODUCT_DEFINITION_SHAPE($,$,#80);
#50137=PRODUCT_DEFINITION_SHAPE($,$,#81);
#50138=PRODUCT_DEFINITION_SHAPE($,$,#82);
#50139=PRODUCT_DEFINITION_SHAPE($,$,#83);
#50140=PRODUCT_DEFINITION_SHAPE($,$,#84);
#50141=PRODUCT_DEFINITION_SHAPE($,$,#85);
#50142=PRODUCT_DEFINITION_SHAPE($,$,#86);
#50143=PRODUCT_DEFINITION_SHAPE($,$,#87);
#50144=PRODUCT_DEFINITION_SHAPE($,$,#88);
#50145=PRODUCT_DEFINITION_SHAPE($,$,#89);
#50146=PRODUCT_DEFINITION_SHAPE($,$,#90);
#50147=SHAPE_REPRESENTATION('',(#10106,#11015,#11016,#11017,#11018,#11019,
#11020,#11021,#11022,#11023,#11024,#11025,#11026,#11027,#11028,#11029,#11030,
#11031,#11032,#11033,#11034),#50060);
#50148=SHAPE_REPRESENTATION('',(#10107),#50061);
#50149=SHAPE_REPRESENTATION('',(#10113),#50062);
#50150=SHAPE_REPRESENTATION('',(#10126),#50063);
#50151=SHAPE_REPRESENTATION('',(#10139),#50064);
#50152=SHAPE_REPRESENTATION('',(#10265),#50065);
#50153=SHAPE_REPRESENTATION('',(#10400),#50066);
#50154=SHAPE_REPRESENTATION('',(#10427),#50067);
#50155=SHAPE_REPRESENTATION('',(#10440),#50068);
#50156=SHAPE_REPRESENTATION('',(#10453),#50069);
#50157=SHAPE_REPRESENTATION('',(#10466),#50070);
#50158=SHAPE_REPRESENTATION('',(#10607),#50071);
#50159=SHAPE_REPRESENTATION('',(#10620),#50072);
#50160=SHAPE_REPRESENTATION('',(#10669),#50073);
#50161=SHAPE_REPRESENTATION('',(#10679),#50074);
#50162=SHAPE_REPRESENTATION('',(#10748),#50075);
#50163=SHAPE_REPRESENTATION('',(#10891),#50076);
#50164=SHAPE_REPRESENTATION('',(#10899),#50077);
#50165=SHAPE_REPRESENTATION('',(#10966),#50078);
#50166=SHAPE_REPRESENTATION('',(#10979),#50079);
#50167=SHAPE_REPRESENTATION('',(#10992),#50080);
#50168=PRODUCT_DEFINITION_CONTEXT('part definition',#50233,'design');
#50169=PRODUCT_DEFINITION('MAT-069','MAT-069',#50190,#50168);
#50170=PRODUCT_DEFINITION('Sensor connector','Sensor connector',#50191,
#50168);
#50171=PRODUCT_DEFINITION('Wire Insulation D','Wire Insulation D',#50192,
#50168);
#50172=PRODUCT_DEFINITION('Wire Insulation C','Wire Insulation C',#50193,
#50168);
#50173=PRODUCT_DEFINITION('Tube coupler','Tube coupler',#50194,#50168);
#50174=PRODUCT_DEFINITION('Heatsink','Heatsink',#50195,#50168);
#50175=PRODUCT_DEFINITION('Collet Clip','Collet Clip',#50196,#50168);
#50176=PRODUCT_DEFINITION('Wire insulation A','Wire insulation A',#50197,
#50168);
#50177=PRODUCT_DEFINITION('Wire 2','Wire 2',#50198,#50168);
#50178=PRODUCT_DEFINITION('Wire 1','Wire 1',#50199,#50168);
#50179=PRODUCT_DEFINITION('Aluminum Thermal Heater Block',
'Aluminum Thermal Heater Block',#50200,#50168);
#50180=PRODUCT_DEFINITION('Wire 4','Wire 4',#50201,#50168);
#50181=PRODUCT_DEFINITION('Filament Thermal Heatbreak Throat',
'Filament Thermal Heatbreak Throat',#50202,#50168);
#50182=PRODUCT_DEFINITION('Heating Cartridge','Heating Cartridge',#50203,
#50168);
#50183=PRODUCT_DEFINITION('Brass Thermal Extrusion Nozzle',
'Brass Thermal Extrusion Nozzle',#50204,#50168);
#50184=PRODUCT_DEFINITION('Silicone Heat Block Thermal Insulator',
'Silicone Heat Block Thermal Insulator',#50205,#50168);
#50185=PRODUCT_DEFINITION('Temperature Sensor Cartridge',
'Temperature Sensor Cartridge',#50206,#50168);
#50186=PRODUCT_DEFINITION('Screw','Screw',#50207,#50168);
#50187=PRODUCT_DEFINITION('Wire Insulation B','Wire Insulation B',#50208,
#50168);
#50188=PRODUCT_DEFINITION('Wire 3','Wire 3',#50209,#50168);
#50189=PRODUCT_DEFINITION('Threaded Drive Coupler Insert',
'Threaded Drive Coupler Insert',#50210,#50168);
#50190=PRODUCT_DEFINITION_FORMATION('',$,#50235);
#50191=PRODUCT_DEFINITION_FORMATION('',$,#50236);
#50192=PRODUCT_DEFINITION_FORMATION('',$,#50237);
#50193=PRODUCT_DEFINITION_FORMATION('',$,#50238);
#50194=PRODUCT_DEFINITION_FORMATION('',$,#50239);
#50195=PRODUCT_DEFINITION_FORMATION('',$,#50240);
#50196=PRODUCT_DEFINITION_FORMATION('',$,#50241);
#50197=PRODUCT_DEFINITION_FORMATION('',$,#50242);
#50198=PRODUCT_DEFINITION_FORMATION('',$,#50243);
#50199=PRODUCT_DEFINITION_FORMATION('',$,#50244);
#50200=PRODUCT_DEFINITION_FORMATION('',$,#50245);
#50201=PRODUCT_DEFINITION_FORMATION('',$,#50246);
#50202=PRODUCT_DEFINITION_FORMATION('',$,#50247);
#50203=PRODUCT_DEFINITION_FORMATION('',$,#50248);
#50204=PRODUCT_DEFINITION_FORMATION('',$,#50249);
#50205=PRODUCT_DEFINITION_FORMATION('',$,#50250);
#50206=PRODUCT_DEFINITION_FORMATION('',$,#50251);
#50207=PRODUCT_DEFINITION_FORMATION('',$,#50252);
#50208=PRODUCT_DEFINITION_FORMATION('',$,#50253);
#50209=PRODUCT_DEFINITION_FORMATION('',$,#50254);
#50210=PRODUCT_DEFINITION_FORMATION('',$,#50255);
#50211=PRODUCT_RELATED_PRODUCT_CATEGORY('MAT-069',
'MAT-069',(#50235));
#50212=PRODUCT_RELATED_PRODUCT_CATEGORY('Sensor connector',
'Sensor connector',(#50236));
#50213=PRODUCT_RELATED_PRODUCT_CATEGORY('Wire Insulation D',
'Wire Insulation D',(#50237));
#50214=PRODUCT_RELATED_PRODUCT_CATEGORY('Wire Insulation C',
'Wire Insulation C',(#50238));
#50215=PRODUCT_RELATED_PRODUCT_CATEGORY('Tube coupler','Tube coupler',(#50239));
#50216=PRODUCT_RELATED_PRODUCT_CATEGORY('Heatsink','Heatsink',(#50240));
#50217=PRODUCT_RELATED_PRODUCT_CATEGORY('Collet Clip','Collet Clip',(#50241));
#50218=PRODUCT_RELATED_PRODUCT_CATEGORY('Wire insulation A',
'Wire insulation A',(#50242));
#50219=PRODUCT_RELATED_PRODUCT_CATEGORY('Wire 2','Wire 2',(#50243));
#50220=PRODUCT_RELATED_PRODUCT_CATEGORY('Wire 1','Wire 1',(#50244));
#50221=PRODUCT_RELATED_PRODUCT_CATEGORY('Aluminum Thermal Heater Block',
'Aluminum Thermal Heater Block',(#50245));
#50222=PRODUCT_RELATED_PRODUCT_CATEGORY('Wire 4','Wire 4',(#50246));
#50223=PRODUCT_RELATED_PRODUCT_CATEGORY(
'Filament Thermal Heatbreak Throat','Filament Thermal Heatbreak Throat',
(#50247));
#50224=PRODUCT_RELATED_PRODUCT_CATEGORY('Heating Cartridge',
'Heating Cartridge',(#50248));
#50225=PRODUCT_RELATED_PRODUCT_CATEGORY(
'Brass Thermal Extrusion Nozzle','Brass Thermal Extrusion Nozzle',(#50249));
#50226=PRODUCT_RELATED_PRODUCT_CATEGORY(
'Silicone Heat Block Thermal Insulator',
'Silicone Heat Block Thermal Insulator',(#50250));
#50227=PRODUCT_RELATED_PRODUCT_CATEGORY('Temperature Sensor Cartridge',
'Temperature Sensor Cartridge',(#50251));
#50228=PRODUCT_RELATED_PRODUCT_CATEGORY('Screw','Screw',(#50252));
#50229=PRODUCT_RELATED_PRODUCT_CATEGORY('Wire Insulation B',
'Wire Insulation B',(#50253));
#50230=PRODUCT_RELATED_PRODUCT_CATEGORY('Wire 3','Wire 3',(#50254));
#50231=PRODUCT_RELATED_PRODUCT_CATEGORY('Threaded Drive Coupler Insert',
'Threaded Drive Coupler Insert',(#50255));
#50232=APPLICATION_PROTOCOL_DEFINITION('international standard',
'ap242_managed_model_based_3d_engineering',2011,#50233);
#50233=APPLICATION_CONTEXT('Managed model based 3d engineering');
#50234=PRODUCT_CONTEXT('part definition',#50233,'mechanical');
#50235=PRODUCT('MAT-069','MAT-069',
'LEGAL AND USAGE DISCLAIMER: this Data/Model is provided \X2\201C\X0\A
S IS\X2\201D\X0\ for informational and representational only. It is a 
geometric approximation and is NOT engineered, certified, or guarantee
d for dimensional accuracy, exact tolerances, or production-level prec
ision. Vendor disclaims all implied warranties including fitness for a
 particular purpose. DO NOT USE FOR DIRECT PHYSICAL MANUFACTURING, AUT
OMATED PRODUCTION, OR SAFETY-CRITICAL SYSTEMS without independent engi
neering verification and resolution of any design discrepancies.',(#50234));
#50236=PRODUCT('Sensor connector','Sensor connector',
'LEGAL AND USAGE DISCLAIMER: this Data/Model is provided \X2\201C\X0\A
S IS\X2\201D\X0\ for informational and representational only. It is a 
geometric approximation and is NOT engineered, certified, or guarantee
d for dimensional accuracy, exact tolerances, or production-level prec
ision. Vendor disclaims all implied warranties including fitness for a
 particular purpose. DO NOT USE FOR DIRECT PHYSICAL MANUFACTURING, AUT
OMATED PRODUCTION, OR SAFETY-CRITICAL SYSTEMS without independent engi
neering verification and resolution of any design discrepancies.',(#50234));
#50237=PRODUCT('Wire Insulation D','Wire Insulation D',
'LEGAL AND USAGE DISCLAIMER: this Data/Model is provided \X2\201C\X0\A
S IS\X2\201D\X0\ for informational and representational only. It is a 
geometric approximation and is NOT engineered, certified, or guarantee
d for dimensional accuracy, exact tolerances, or production-level prec
ision. Vendor disclaims all implied warranties including fitness for a
 particular purpose. DO NOT USE FOR DIRECT PHYSICAL MANUFACTURING, AUT
OMATED PRODUCTION, OR SAFETY-CRITICAL SYSTEMS without independent engi
neering verification and resolution of any design discrepancies.',(#50234));
#50238=PRODUCT('Wire Insulation C','Wire Insulation C',
'Sensor Cartridge v1',(#50234));
#50239=PRODUCT('Tube coupler','Tube coupler',
'LEGAL AND USAGE DISCLAIMER: this Data/Model is provided \X2\201C\X0\A
S IS\X2\201D\X0\ for informational and representational only. It is a 
geometric approximation and is NOT engineered, certified, or guarantee
d for dimensional accuracy, exact tolerances, or production-level prec
ision. Vendor disclaims all implied warranties including fitness for a
 particular purpose. DO NOT USE FOR DIRECT PHYSICAL MANUFACTURING, AUT
OMATED PRODUCTION, OR SAFETY-CRITICAL SYSTEMS without independent engi
neering verification and resolution of any design discrepancies.',(#50234));
#50240=PRODUCT('Heatsink','Heatsink',
'LEGAL AND USAGE DISCLAIMER: this Data/Model is provided \X2\201C\X0\A
S IS\X2\201D\X0\ for informational and representational only. It is a 
geometric approximation and is NOT engineered, certified, or guarantee
d for dimensional accuracy, exact tolerances, or production-level prec
ision. Vendor disclaims all implied warranties including fitness for a
 particular purpose. DO NOT USE FOR DIRECT PHYSICAL MANUFACTURING, AUT
OMATED PRODUCTION, OR SAFETY-CRITICAL SYSTEMS without independent engi
neering verification and resolution of any design discrepancies.',(#50234));
#50241=PRODUCT('Collet Clip','Collet Clip',
'LEGAL AND USAGE DISCLAIMER: this Data/Model is provided \X2\201C\X0\A
S IS\X2\201D\X0\ for informational and representational only. It is a 
geometric approximation and is NOT engineered, certified, or guarantee
d for dimensional accuracy, exact tolerances, or production-level prec
ision. Vendor disclaims all implied warranties including fitness for a
 particular purpose. DO NOT USE FOR DIRECT PHYSICAL MANUFACTURING, AUT
OMATED PRODUCTION, OR SAFETY-CRITICAL SYSTEMS without independent engi
neering verification and resolution of any design discrepancies.',(#50234));
#50242=PRODUCT('Wire insulation A','Wire insulation A',
'LEGAL AND USAGE DISCLAIMER: this Data/Model is provided \X2\201C\X0\A
S IS\X2\201D\X0\ for informational and representational only. It is a 
geometric approximation and is NOT engineered, certified, or guarantee
d for dimensional accuracy, exact tolerances, or production-level prec
ision. Vendor disclaims all implied warranties including fitness for a
 particular purpose. DO NOT USE FOR DIRECT PHYSICAL MANUFACTURING, AUT
OMATED PRODUCTION, OR SAFETY-CRITICAL SYSTEMS without independent engi
neering verification and resolution of any design discrepancies.',(#50234));
#50243=PRODUCT('Wire 2','Wire 2','Wire',(#50234));
#50244=PRODUCT('Wire 1','Wire 1','Wire_1',(#50234));
#50245=PRODUCT('Aluminum Thermal Heater Block',
'Aluminum Thermal Heater Block',
'LEGAL AND USAGE DISCLAIMER: this Data/Model is provided \X2\201C\X0\A
S IS\X2\201D\X0\ for informational and representational only. It is a 
geometric approximation and is NOT engineered, certified, or guarantee
d for dimensional accuracy, exact tolerances, or production-level prec
ision. Vendor disclaims all implied warranties including fitness for a
 particular purpose. DO NOT USE FOR DIRECT PHYSICAL MANUFACTURING, AUT
OMATED PRODUCTION, OR SAFETY-CRITICAL SYSTEMS without independent engi
neering verification and resolution of any design discrepancies.',(#50234));
#50246=PRODUCT('Wire 4','Wire 4',
'LEGAL AND USAGE DISCLAIMER: this Data/Model is provided \X2\201C\X0\A
S IS\X2\201D\X0\ for informational and representational only. It is a 
geometric approximation and is NOT engineered, certified, or guarantee
d for dimensional accuracy, exact tolerances, or production-level prec
ision. Vendor disclaims all implied warranties including fitness for a
 particular purpose. DO NOT USE FOR DIRECT PHYSICAL MANUFACTURING, AUT
OMATED PRODUCTION, OR SAFETY-CRITICAL SYSTEMS without independent engi
neering verification and resolution of any design discrepancies.',(#50234));
#50247=PRODUCT('Filament Thermal Heatbreak Throat',
'Filament Thermal Heatbreak Throat',
'LEGAL AND USAGE DISCLAIMER: this Data/Model is provided \X2\201C\X0\A
S IS\X2\201D\X0\ for informational and representational only. It is a 
geometric approximation and is NOT engineered, certified, or guarantee
d for dimensional accuracy, exact tolerances, or production-level prec
ision. Vendor disclaims all implied warranties including fitness for a
 particular purpose. DO NOT USE FOR DIRECT PHYSICAL MANUFACTURING, AUT
OMATED PRODUCTION, OR SAFETY-CRITICAL SYSTEMS without independent engi
neering verification and resolution of any design discrepancies.',(#50234));
#50248=PRODUCT('Heating Cartridge','Heating Cartridge',
'LEGAL AND USAGE DISCLAIMER: this Data/Model is provided \X2\201C\X0\A
S IS\X2\201D\X0\ for informational and representational only. It is a 
geometric approximation and is NOT engineered, certified, or guarantee
d for dimensional accuracy, exact tolerances, or production-level prec
ision. Vendor disclaims all implied warranties including fitness for a
 particular purpose. DO NOT USE FOR DIRECT PHYSICAL MANUFACTURING, AUT
OMATED PRODUCTION, OR SAFETY-CRITICAL SYSTEMS without independent engi
neering verification and resolution of any design discrepancies.',(#50234));
#50249=PRODUCT('Brass Thermal Extrusion Nozzle',
'Brass Thermal Extrusion Nozzle',
'LEGAL AND USAGE DISCLAIMER: this Data/Model is provided \X2\201C\X0\A
S IS\X2\201D\X0\ for informational and representational only. It is a 
geometric approximation and is NOT engineered, certified, or guarantee
d for dimensional accuracy, exact tolerances, or production-level prec
ision. Vendor disclaims all implied warranties including fitness for a
 particular purpose. DO NOT USE FOR DIRECT PHYSICAL MANUFACTURING, AUT
OMATED PRODUCTION, OR SAFETY-CRITICAL SYSTEMS without independent engi
neering verification and resolution of any design discrepancies.',(#50234));
#50250=PRODUCT('Silicone Heat Block Thermal Insulator',
'Silicone Heat Block Thermal Insulator',
'LEGAL AND USAGE DISCLAIMER: this Data/Model is provided \X2\201C\X0\A
S IS\X2\201D\X0\ for informational and representational only. It is a 
geometric approximation and is NOT engineered, certified, or guarantee
d for dimensional accuracy, exact tolerances, or production-level prec
ision. Vendor disclaims all implied warranties including fitness for a
 particular purpose. DO NOT USE FOR DIRECT PHYSICAL MANUFACTURING, AUT
OMATED PRODUCTION, OR SAFETY-CRITICAL SYSTEMS without independent engi
neering verification and resolution of any design discrepancies.',(#50234));
#50251=PRODUCT('Temperature Sensor Cartridge',
'Temperature Sensor Cartridge',
'LEGAL AND USAGE DISCLAIMER: this Data/Model is provided \X2\201C\X0\A
S IS\X2\201D\X0\ for informational and representational only. It is a 
geometric approximation and is NOT engineered, certified, or guarantee
d for dimensional accuracy, exact tolerances, or production-level prec
ision. Vendor disclaims all implied warranties including fitness for a
 particular purpose. DO NOT USE FOR DIRECT PHYSICAL MANUFACTURING, AUT
OMATED PRODUCTION, OR SAFETY-CRITICAL SYSTEMS without independent engi
neering verification and resolution of any design discrepancies.',(#50234));
#50252=PRODUCT('Screw','Screw',$,(#50234));
#50253=PRODUCT('Wire Insulation B','Wire Insulation B','Component3',(#50234));
#50254=PRODUCT('Wire 3','Wire 3','Sensor Cartridge v1',(#50234));
#50255=PRODUCT('Threaded Drive Coupler Insert',
'Threaded Drive Coupler Insert',
'LEGAL AND USAGE DISCLAIMER: this Data/Model is provided \X2\201C\X0\A
S IS\X2\201D\X0\ for informational and representational only. It is a 
geometric approximation and is NOT engineered, certified, or guarantee
d for dimensional accuracy, exact tolerances, or production-level prec
ision. Vendor disclaims all implied warranties including fitness for a
 particular purpose. DO NOT USE FOR DIRECT PHYSICAL MANUFACTURING, AUT
OMATED PRODUCTION, OR SAFETY-CRITICAL SYSTEMS without independent engi
neering verification and resolution of any design discrepancies.',(#50234));
#50256=PRESENTATION_STYLE_ASSIGNMENT((#50263));
#50257=PRESENTATION_STYLE_ASSIGNMENT((#50264));
#50258=PRESENTATION_STYLE_ASSIGNMENT((#50265));
#50259=PRESENTATION_STYLE_ASSIGNMENT((#50266));
#50260=PRESENTATION_STYLE_ASSIGNMENT((#50267));
#50261=PRESENTATION_STYLE_ASSIGNMENT((#50268));
#50262=PRESENTATION_STYLE_ASSIGNMENT((#50269));
#50263=SURFACE_STYLE_USAGE(.BOTH.,#50270);
#50264=SURFACE_STYLE_USAGE(.BOTH.,#50271);
#50265=SURFACE_STYLE_USAGE(.BOTH.,#50272);
#50266=SURFACE_STYLE_USAGE(.BOTH.,#50273);
#50267=SURFACE_STYLE_USAGE(.BOTH.,#50274);
#50268=SURFACE_STYLE_USAGE(.BOTH.,#50275);
#50269=SURFACE_STYLE_USAGE(.BOTH.,#50276);
#50270=SURFACE_SIDE_STYLE('',(#50277));
#50271=SURFACE_SIDE_STYLE('',(#50278));
#50272=SURFACE_SIDE_STYLE('',(#50279));
#50273=SURFACE_SIDE_STYLE('',(#50280));
#50274=SURFACE_SIDE_STYLE('',(#50281));
#50275=SURFACE_SIDE_STYLE('',(#50282));
#50276=SURFACE_SIDE_STYLE('',(#50283));
#50277=SURFACE_STYLE_FILL_AREA(#50284);
#50278=SURFACE_STYLE_FILL_AREA(#50285);
#50279=SURFACE_STYLE_FILL_AREA(#50286);
#50280=SURFACE_STYLE_FILL_AREA(#50287);
#50281=SURFACE_STYLE_FILL_AREA(#50288);
#50282=SURFACE_STYLE_FILL_AREA(#50289);
#50283=SURFACE_STYLE_FILL_AREA(#50290);
#50284=FILL_AREA_STYLE('Steel - Satin',(#50291));
#50285=FILL_AREA_STYLE('Opaque(137,137,137)',(#50292));
#50286=FILL_AREA_STYLE('Opaque(89,149,218)',(#50293));
#50287=FILL_AREA_STYLE('Opaque(246,246,243)',(#50294));
#50288=FILL_AREA_STYLE('Opaque(25,25,25)',(#50295));
#50289=FILL_AREA_STYLE('Opaque(179,179,179)',(#50296));
#50290=FILL_AREA_STYLE('Opaque(48,59,150)',(#50297));
#50291=FILL_AREA_STYLE_COLOUR('Steel - Satin',#50298);
#50292=FILL_AREA_STYLE_COLOUR('Opaque(137,137,137)',#50299);
#50293=FILL_AREA_STYLE_COLOUR('Opaque(89,149,218)',#50300);
#50294=FILL_AREA_STYLE_COLOUR('Opaque(246,246,243)',#50301);
#50295=FILL_AREA_STYLE_COLOUR('Opaque(25,25,25)',#50302);
#50296=FILL_AREA_STYLE_COLOUR('Opaque(179,179,179)',#50303);
#50297=FILL_AREA_STYLE_COLOUR('Opaque(48,59,150)',#50304);
#50298=COLOUR_RGB('Steel - Satin',0.627450980392157,0.627450980392157,0.627450980392157);
#50299=COLOUR_RGB('Opaque(137,137,137)',0.537254901960784,0.537254901960784,
0.537254901960784);
#50300=COLOUR_RGB('Opaque(89,149,218)',0.349019607843137,0.584313725490196,
0.854901960784314);
#50301=COLOUR_RGB('Opaque(246,246,243)',0.964705882352941,0.964705882352941,
0.952941176470588);
#50302=COLOUR_RGB('Opaque(25,25,25)',0.0980392156862745,0.0980392156862745,
0.0980392156862745);
#50303=COLOUR_RGB('Opaque(179,179,179)',0.701960784313725,0.701960784313725,
0.701960784313725);
#50304=COLOUR_RGB('Opaque(48,59,150)',0.188235294117647,0.231372549019608,
0.588235294117647);
ENDSEC;
END-ISO-10303-21;
